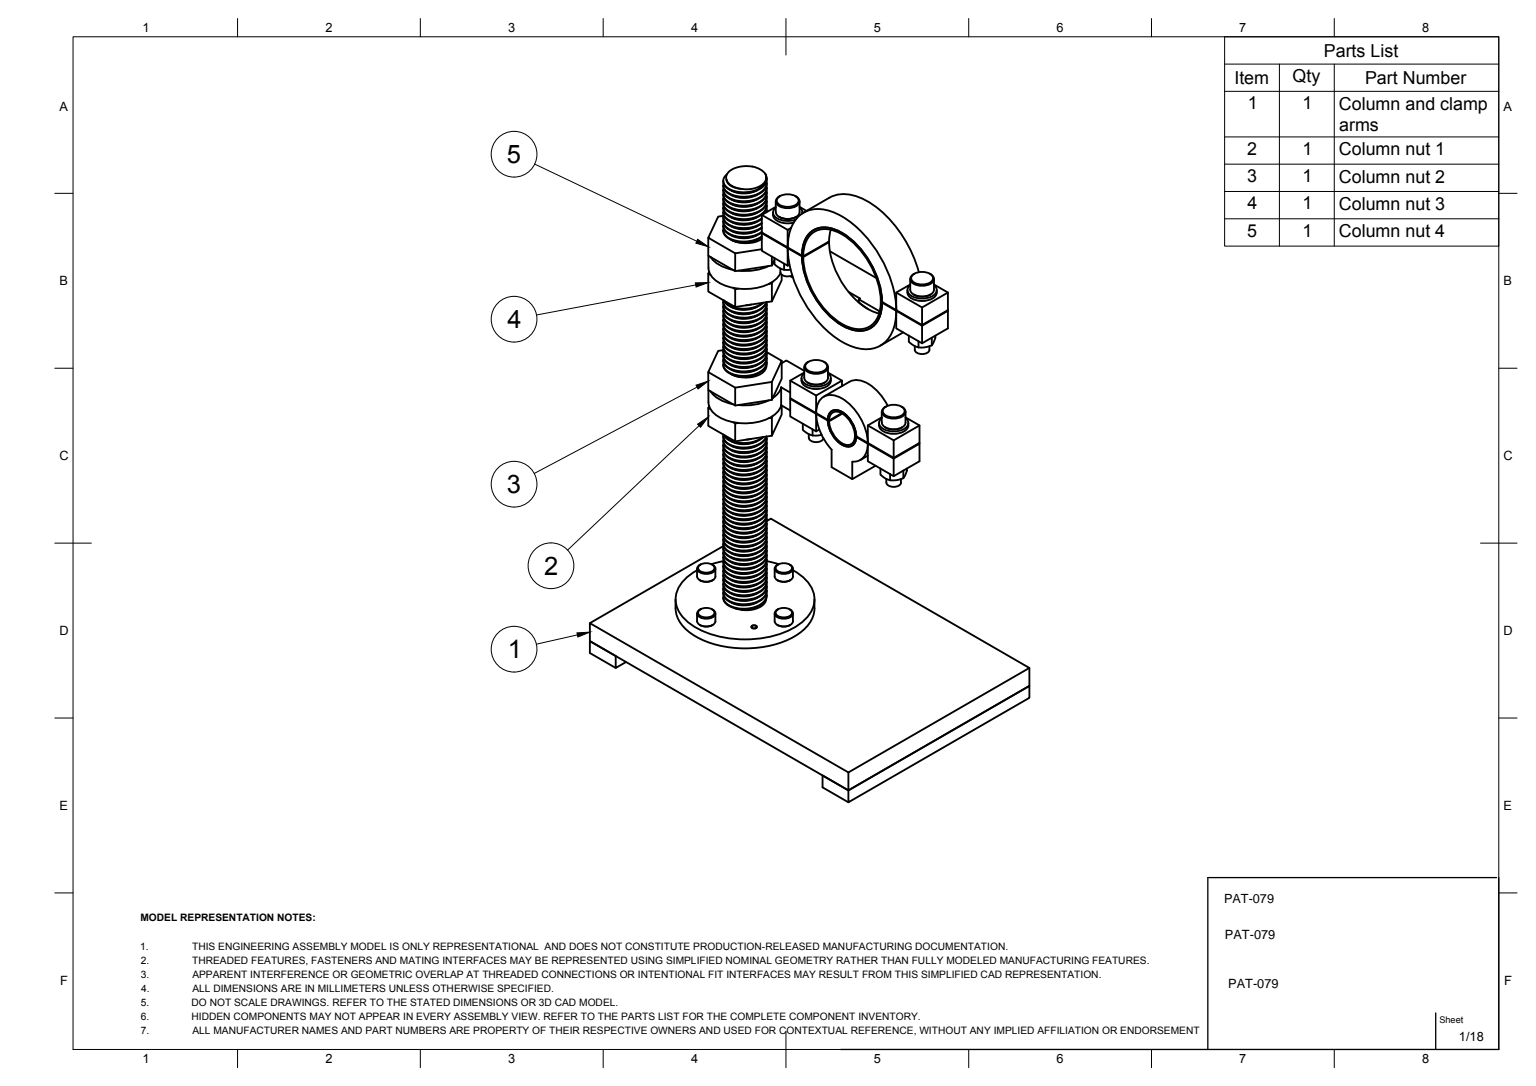
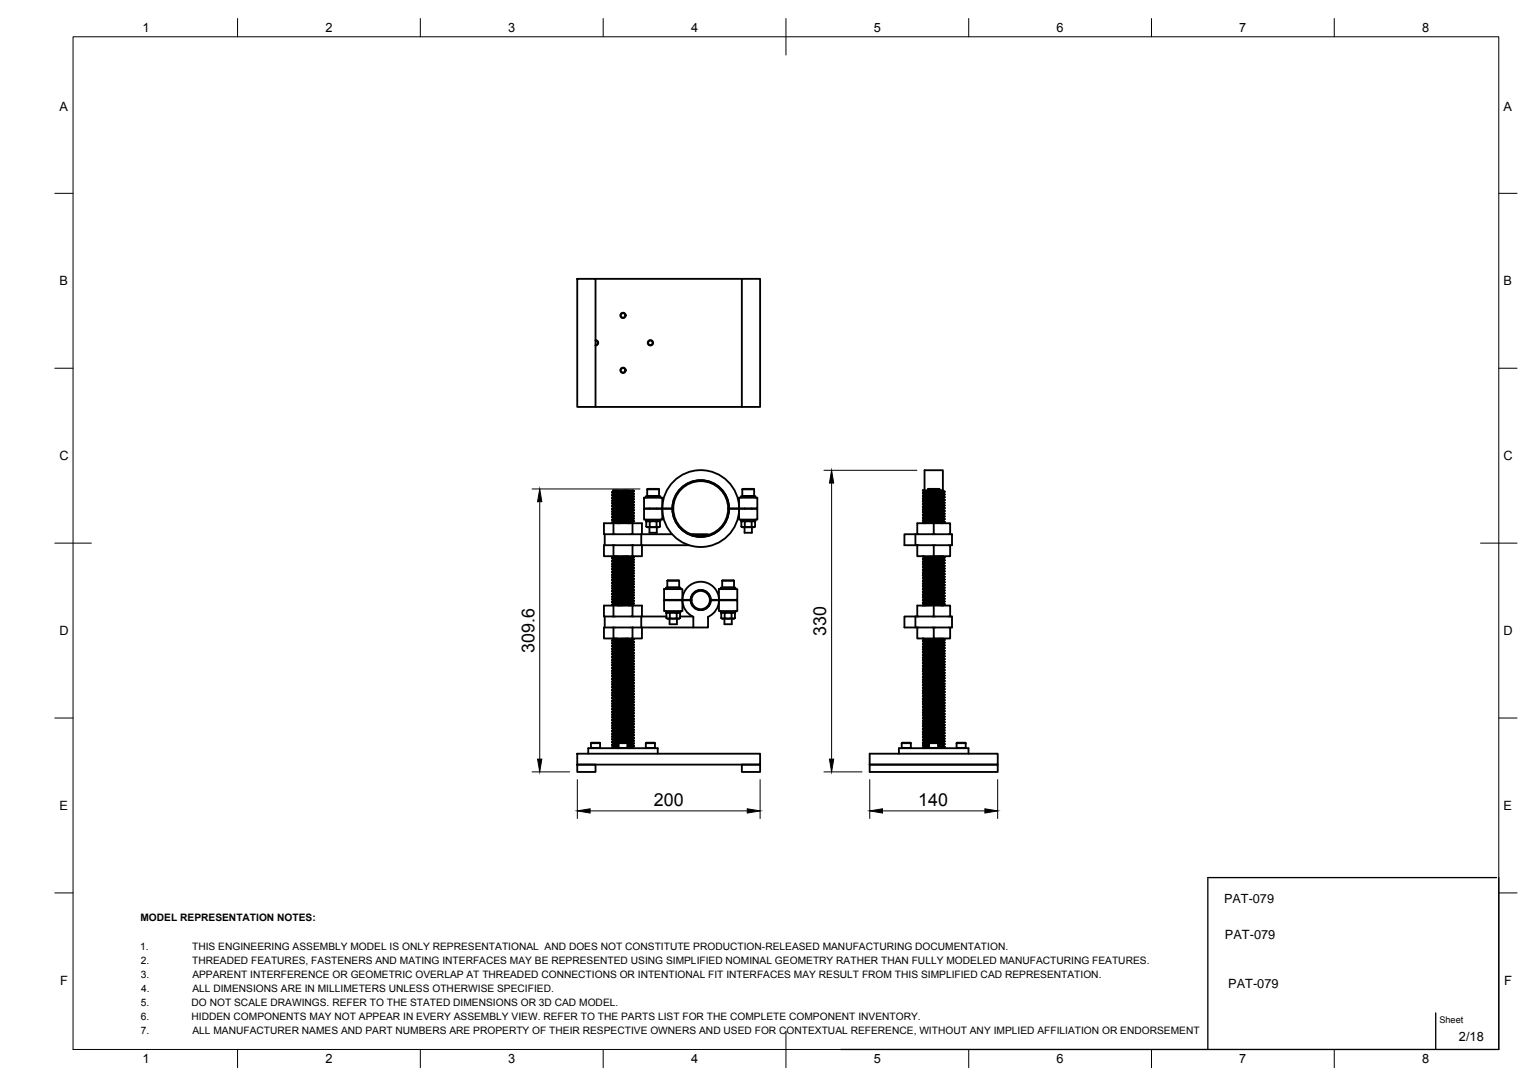
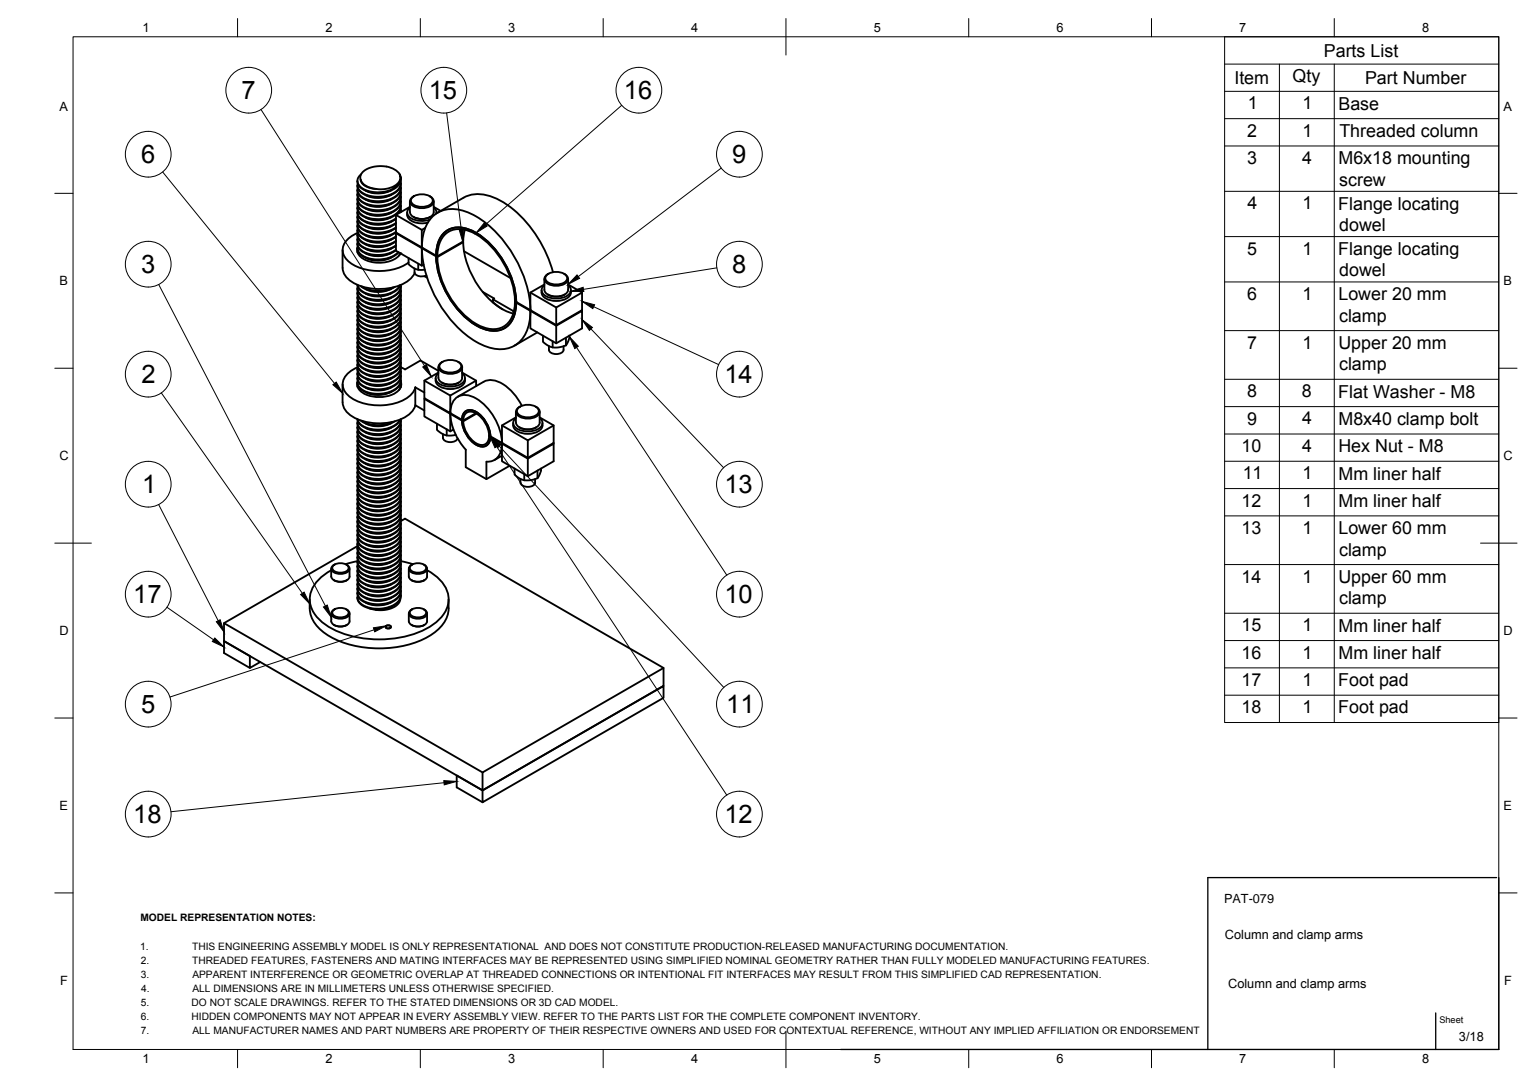
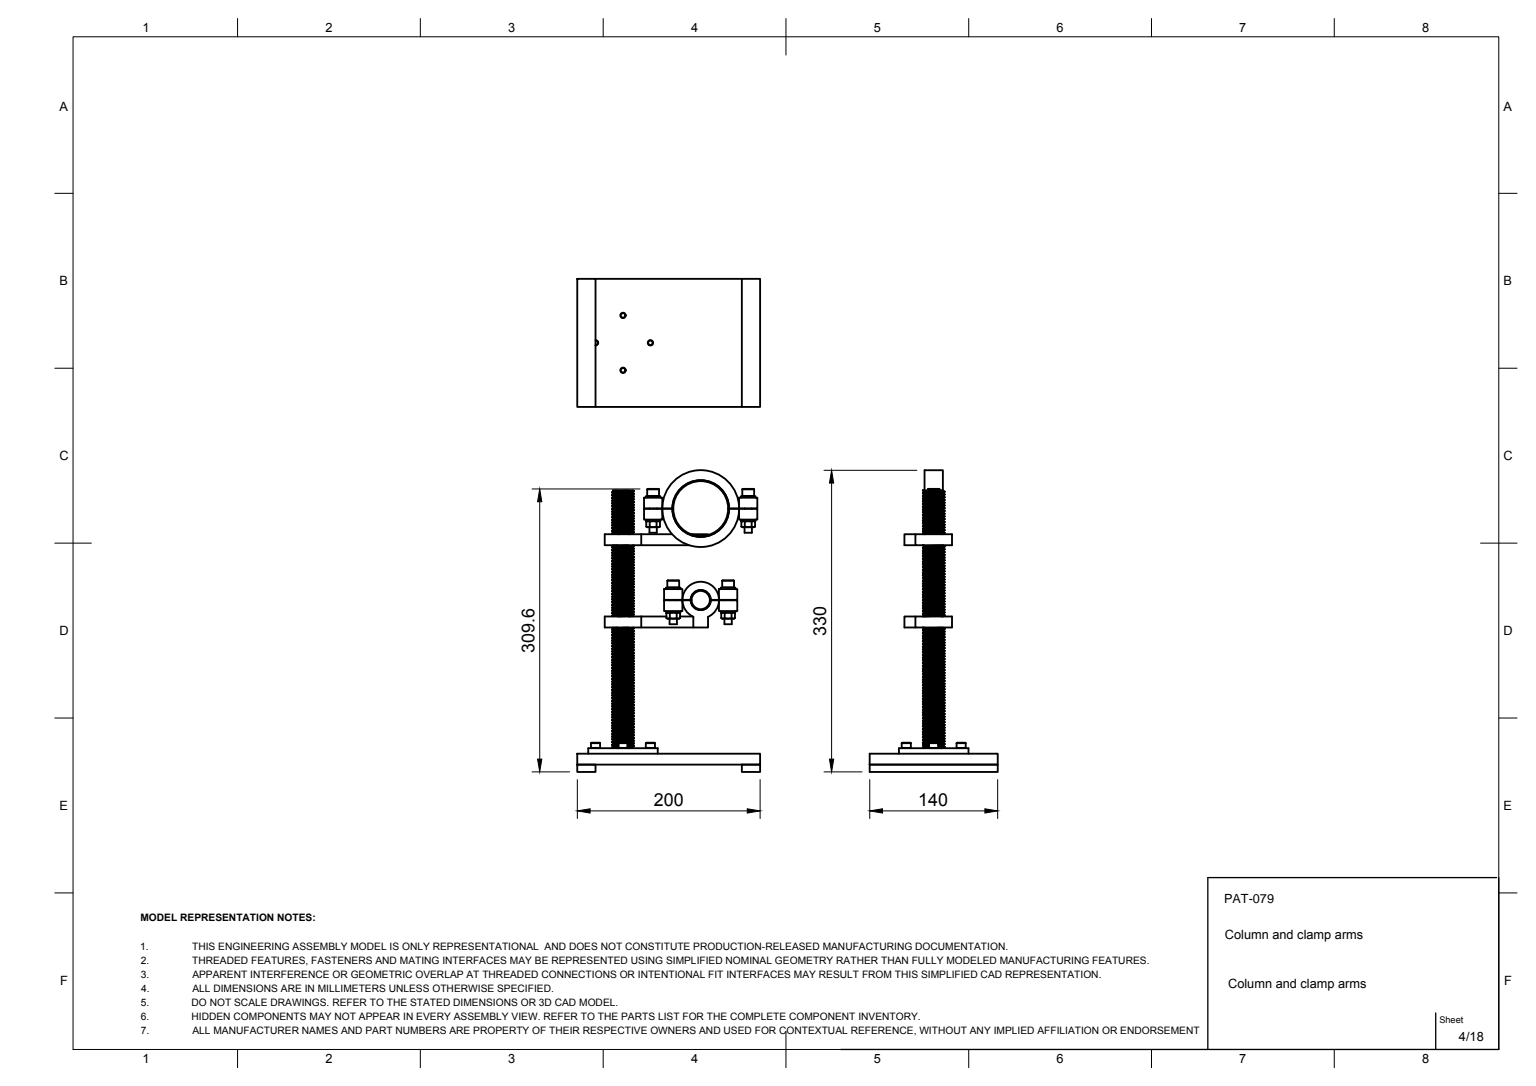
ISO-10303-21;
HEADER;
/* Generated by software containing ST-Developer
 * from STEP Tools, Inc. (www.steptools.com) 
 */

FILE_DESCRIPTION(
/* description */ ('Pipe clamp stand with threaded column'),
/* implementation_level */ '2;1');

FILE_NAME(
/* name */ 'PAT-079',
/* time_stamp */ '2026-10-27T10:55:48-07:00',
/* author */ (''),
/* organization */ (''),
/* preprocessor_version */ 'ST-DEVELOPER v20.2',
/* originating_system */ 'Autodesk Translation Framework v15.17.0.0',
/* authorisation */ '');

FILE_SCHEMA (('AUTOMOTIVE_DESIGN { 1 0 10303 214 3 1 1 }'));
ENDSEC;

DATA;
#10=MECHANICAL_DESIGN_GEOMETRIC_PRESENTATION_REPRESENTATION('',(#741,#742,
#743,#744,#745,#746,#747,#748,#749,#750,#751,#752,#753,#754,#755,#756,#757,
#758,#759,#760,#761,#762,#763,#764,#765,#766,#767,#768,#769,#770),#34433);
#11=ITEM_DEFINED_TRANSFORMATION($,$,#9045,#9586);
#12=ITEM_DEFINED_TRANSFORMATION($,$,#9072,#9587);
#13=ITEM_DEFINED_TRANSFORMATION($,$,#9291,#9588);
#14=ITEM_DEFINED_TRANSFORMATION($,$,#9297,#9589);
#15=ITEM_DEFINED_TRANSFORMATION($,$,#9303,#9590);
#16=ITEM_DEFINED_TRANSFORMATION($,$,#9348,#9591);
#17=ITEM_DEFINED_TRANSFORMATION($,$,#9377,#9592);
#18=ITEM_DEFINED_TRANSFORMATION($,$,#9388,#9593);
#19=ITEM_DEFINED_TRANSFORMATION($,$,#9399,#9594);
#20=ITEM_DEFINED_TRANSFORMATION($,$,#9444,#9595);
#21=ITEM_DEFINED_TRANSFORMATION($,$,#9473,#9596);
#22=ITEM_DEFINED_TRANSFORMATION($,$,#9484,#9597);
#23=ITEM_DEFINED_TRANSFORMATION($,$,#9495,#9598);
#24=ITEM_DEFINED_TRANSFORMATION($,$,#9502,#9599);
#25=ITEM_DEFINED_TRANSFORMATION($,$,#9509,#9600);
#26=ITEM_DEFINED_TRANSFORMATION($,$,#9509,#9601);
#27=ITEM_DEFINED_TRANSFORMATION($,$,#9509,#9602);
#28=ITEM_DEFINED_TRANSFORMATION($,$,#9509,#9603);
#29=ITEM_DEFINED_TRANSFORMATION($,$,#9561,#9604);
#30=ITEM_DEFINED_TRANSFORMATION($,$,#9533,#9605);
#31=ITEM_DEFINED_TRANSFORMATION($,$,#9561,#9606);
#32=ITEM_DEFINED_TRANSFORMATION($,$,#9570,#9607);
#33=ITEM_DEFINED_TRANSFORMATION($,$,#9561,#9608);
#34=ITEM_DEFINED_TRANSFORMATION($,$,#9533,#9609);
#35=ITEM_DEFINED_TRANSFORMATION($,$,#9561,#9610);
#36=ITEM_DEFINED_TRANSFORMATION($,$,#9570,#9611);
#37=ITEM_DEFINED_TRANSFORMATION($,$,#9561,#9612);
#38=ITEM_DEFINED_TRANSFORMATION($,$,#9533,#9613);
#39=ITEM_DEFINED_TRANSFORMATION($,$,#9561,#9614);
#40=ITEM_DEFINED_TRANSFORMATION($,$,#9570,#9615);
#41=ITEM_DEFINED_TRANSFORMATION($,$,#9561,#9616);
#42=ITEM_DEFINED_TRANSFORMATION($,$,#9533,#9617);
#43=ITEM_DEFINED_TRANSFORMATION($,$,#9561,#9618);
#44=ITEM_DEFINED_TRANSFORMATION($,$,#9570,#9619);
#45=ITEM_DEFINED_TRANSFORMATION($,$,#9621,#9644);
#46=ITEM_DEFINED_TRANSFORMATION($,$,#9646,#9669);
#47=ITEM_DEFINED_TRANSFORMATION($,$,#9671,#9694);
#48=ITEM_DEFINED_TRANSFORMATION($,$,#9696,#9719);
#49=ITEM_DEFINED_TRANSFORMATION($,$,#9044,#9720);
#50=ITEM_DEFINED_TRANSFORMATION($,$,#9620,#9721);
#51=ITEM_DEFINED_TRANSFORMATION($,$,#9645,#9722);
#52=ITEM_DEFINED_TRANSFORMATION($,$,#9670,#9723);
#53=ITEM_DEFINED_TRANSFORMATION($,$,#9695,#9724);
#54=(
REPRESENTATION_RELATIONSHIP($,$,#34539,#34538)
REPRESENTATION_RELATIONSHIP_WITH_TRANSFORMATION(#11)
SHAPE_REPRESENTATION_RELATIONSHIP()
);
#55=(
REPRESENTATION_RELATIONSHIP($,$,#34540,#34538)
REPRESENTATION_RELATIONSHIP_WITH_TRANSFORMATION(#12)
SHAPE_REPRESENTATION_RELATIONSHIP()
);
#56=(
REPRESENTATION_RELATIONSHIP($,$,#34541,#34538)
REPRESENTATION_RELATIONSHIP_WITH_TRANSFORMATION(#13)
SHAPE_REPRESENTATION_RELATIONSHIP()
);
#57=(
REPRESENTATION_RELATIONSHIP($,$,#34542,#34538)
REPRESENTATION_RELATIONSHIP_WITH_TRANSFORMATION(#14)
SHAPE_REPRESENTATION_RELATIONSHIP()
);
#58=(
REPRESENTATION_RELATIONSHIP($,$,#34543,#34538)
REPRESENTATION_RELATIONSHIP_WITH_TRANSFORMATION(#15)
SHAPE_REPRESENTATION_RELATIONSHIP()
);
#59=(
REPRESENTATION_RELATIONSHIP($,$,#34544,#34538)
REPRESENTATION_RELATIONSHIP_WITH_TRANSFORMATION(#16)
SHAPE_REPRESENTATION_RELATIONSHIP()
);
#60=(
REPRESENTATION_RELATIONSHIP($,$,#34545,#34538)
REPRESENTATION_RELATIONSHIP_WITH_TRANSFORMATION(#17)
SHAPE_REPRESENTATION_RELATIONSHIP()
);
#61=(
REPRESENTATION_RELATIONSHIP($,$,#34546,#34538)
REPRESENTATION_RELATIONSHIP_WITH_TRANSFORMATION(#18)
SHAPE_REPRESENTATION_RELATIONSHIP()
);
#62=(
REPRESENTATION_RELATIONSHIP($,$,#34547,#34538)
REPRESENTATION_RELATIONSHIP_WITH_TRANSFORMATION(#19)
SHAPE_REPRESENTATION_RELATIONSHIP()
);
#63=(
REPRESENTATION_RELATIONSHIP($,$,#34548,#34538)
REPRESENTATION_RELATIONSHIP_WITH_TRANSFORMATION(#20)
SHAPE_REPRESENTATION_RELATIONSHIP()
);
#64=(
REPRESENTATION_RELATIONSHIP($,$,#34549,#34538)
REPRESENTATION_RELATIONSHIP_WITH_TRANSFORMATION(#21)
SHAPE_REPRESENTATION_RELATIONSHIP()
);
#65=(
REPRESENTATION_RELATIONSHIP($,$,#34550,#34538)
REPRESENTATION_RELATIONSHIP_WITH_TRANSFORMATION(#22)
SHAPE_REPRESENTATION_RELATIONSHIP()
);
#66=(
REPRESENTATION_RELATIONSHIP($,$,#34551,#34538)
REPRESENTATION_RELATIONSHIP_WITH_TRANSFORMATION(#23)
SHAPE_REPRESENTATION_RELATIONSHIP()
);
#67=(
REPRESENTATION_RELATIONSHIP($,$,#34552,#34538)
REPRESENTATION_RELATIONSHIP_WITH_TRANSFORMATION(#24)
SHAPE_REPRESENTATION_RELATIONSHIP()
);
#68=(
REPRESENTATION_RELATIONSHIP($,$,#34553,#34538)
REPRESENTATION_RELATIONSHIP_WITH_TRANSFORMATION(#25)
SHAPE_REPRESENTATION_RELATIONSHIP()
);
#69=(
REPRESENTATION_RELATIONSHIP($,$,#34553,#34538)
REPRESENTATION_RELATIONSHIP_WITH_TRANSFORMATION(#26)
SHAPE_REPRESENTATION_RELATIONSHIP()
);
#70=(
REPRESENTATION_RELATIONSHIP($,$,#34553,#34538)
REPRESENTATION_RELATIONSHIP_WITH_TRANSFORMATION(#27)
SHAPE_REPRESENTATION_RELATIONSHIP()
);
#71=(
REPRESENTATION_RELATIONSHIP($,$,#34553,#34538)
REPRESENTATION_RELATIONSHIP_WITH_TRANSFORMATION(#28)
SHAPE_REPRESENTATION_RELATIONSHIP()
);
#72=(
REPRESENTATION_RELATIONSHIP($,$,#34555,#34538)
REPRESENTATION_RELATIONSHIP_WITH_TRANSFORMATION(#29)
SHAPE_REPRESENTATION_RELATIONSHIP()
);
#73=(
REPRESENTATION_RELATIONSHIP($,$,#34554,#34538)
REPRESENTATION_RELATIONSHIP_WITH_TRANSFORMATION(#30)
SHAPE_REPRESENTATION_RELATIONSHIP()
);
#74=(
REPRESENTATION_RELATIONSHIP($,$,#34555,#34538)
REPRESENTATION_RELATIONSHIP_WITH_TRANSFORMATION(#31)
SHAPE_REPRESENTATION_RELATIONSHIP()
);
#75=(
REPRESENTATION_RELATIONSHIP($,$,#34556,#34538)
REPRESENTATION_RELATIONSHIP_WITH_TRANSFORMATION(#32)
SHAPE_REPRESENTATION_RELATIONSHIP()
);
#76=(
REPRESENTATION_RELATIONSHIP($,$,#34555,#34538)
REPRESENTATION_RELATIONSHIP_WITH_TRANSFORMATION(#33)
SHAPE_REPRESENTATION_RELATIONSHIP()
);
#77=(
REPRESENTATION_RELATIONSHIP($,$,#34554,#34538)
REPRESENTATION_RELATIONSHIP_WITH_TRANSFORMATION(#34)
SHAPE_REPRESENTATION_RELATIONSHIP()
);
#78=(
REPRESENTATION_RELATIONSHIP($,$,#34555,#34538)
REPRESENTATION_RELATIONSHIP_WITH_TRANSFORMATION(#35)
SHAPE_REPRESENTATION_RELATIONSHIP()
);
#79=(
REPRESENTATION_RELATIONSHIP($,$,#34556,#34538)
REPRESENTATION_RELATIONSHIP_WITH_TRANSFORMATION(#36)
SHAPE_REPRESENTATION_RELATIONSHIP()
);
#80=(
REPRESENTATION_RELATIONSHIP($,$,#34555,#34538)
REPRESENTATION_RELATIONSHIP_WITH_TRANSFORMATION(#37)
SHAPE_REPRESENTATION_RELATIONSHIP()
);
#81=(
REPRESENTATION_RELATIONSHIP($,$,#34554,#34538)
REPRESENTATION_RELATIONSHIP_WITH_TRANSFORMATION(#38)
SHAPE_REPRESENTATION_RELATIONSHIP()
);
#82=(
REPRESENTATION_RELATIONSHIP($,$,#34555,#34538)
REPRESENTATION_RELATIONSHIP_WITH_TRANSFORMATION(#39)
SHAPE_REPRESENTATION_RELATIONSHIP()
);
#83=(
REPRESENTATION_RELATIONSHIP($,$,#34556,#34538)
REPRESENTATION_RELATIONSHIP_WITH_TRANSFORMATION(#40)
SHAPE_REPRESENTATION_RELATIONSHIP()
);
#84=(
REPRESENTATION_RELATIONSHIP($,$,#34555,#34538)
REPRESENTATION_RELATIONSHIP_WITH_TRANSFORMATION(#41)
SHAPE_REPRESENTATION_RELATIONSHIP()
);
#85=(
REPRESENTATION_RELATIONSHIP($,$,#34554,#34538)
REPRESENTATION_RELATIONSHIP_WITH_TRANSFORMATION(#42)
SHAPE_REPRESENTATION_RELATIONSHIP()
);
#86=(
REPRESENTATION_RELATIONSHIP($,$,#34555,#34538)
REPRESENTATION_RELATIONSHIP_WITH_TRANSFORMATION(#43)
SHAPE_REPRESENTATION_RELATIONSHIP()
);
#87=(
REPRESENTATION_RELATIONSHIP($,$,#34556,#34538)
REPRESENTATION_RELATIONSHIP_WITH_TRANSFORMATION(#44)
SHAPE_REPRESENTATION_RELATIONSHIP()
);
#88=(
REPRESENTATION_RELATIONSHIP($,$,#34558,#34557)
REPRESENTATION_RELATIONSHIP_WITH_TRANSFORMATION(#45)
SHAPE_REPRESENTATION_RELATIONSHIP()
);
#89=(
REPRESENTATION_RELATIONSHIP($,$,#34560,#34559)
REPRESENTATION_RELATIONSHIP_WITH_TRANSFORMATION(#46)
SHAPE_REPRESENTATION_RELATIONSHIP()
);
#90=(
REPRESENTATION_RELATIONSHIP($,$,#34562,#34561)
REPRESENTATION_RELATIONSHIP_WITH_TRANSFORMATION(#47)
SHAPE_REPRESENTATION_RELATIONSHIP()
);
#91=(
REPRESENTATION_RELATIONSHIP($,$,#34564,#34563)
REPRESENTATION_RELATIONSHIP_WITH_TRANSFORMATION(#48)
SHAPE_REPRESENTATION_RELATIONSHIP()
);
#92=(
REPRESENTATION_RELATIONSHIP($,$,#34538,#34537)
REPRESENTATION_RELATIONSHIP_WITH_TRANSFORMATION(#49)
SHAPE_REPRESENTATION_RELATIONSHIP()
);
#93=(
REPRESENTATION_RELATIONSHIP($,$,#34557,#34537)
REPRESENTATION_RELATIONSHIP_WITH_TRANSFORMATION(#50)
SHAPE_REPRESENTATION_RELATIONSHIP()
);
#94=(
REPRESENTATION_RELATIONSHIP($,$,#34559,#34537)
REPRESENTATION_RELATIONSHIP_WITH_TRANSFORMATION(#51)
SHAPE_REPRESENTATION_RELATIONSHIP()
);
#95=(
REPRESENTATION_RELATIONSHIP($,$,#34561,#34537)
REPRESENTATION_RELATIONSHIP_WITH_TRANSFORMATION(#52)
SHAPE_REPRESENTATION_RELATIONSHIP()
);
#96=(
REPRESENTATION_RELATIONSHIP($,$,#34563,#34537)
REPRESENTATION_RELATIONSHIP_WITH_TRANSFORMATION(#53)
SHAPE_REPRESENTATION_RELATIONSHIP()
);
#97=CONTEXT_DEPENDENT_SHAPE_REPRESENTATION(#54,#34486);
#98=CONTEXT_DEPENDENT_SHAPE_REPRESENTATION(#55,#34487);
#99=CONTEXT_DEPENDENT_SHAPE_REPRESENTATION(#56,#34488);
#100=CONTEXT_DEPENDENT_SHAPE_REPRESENTATION(#57,#34489);
#101=CONTEXT_DEPENDENT_SHAPE_REPRESENTATION(#58,#34490);
#102=CONTEXT_DEPENDENT_SHAPE_REPRESENTATION(#59,#34491);
#103=CONTEXT_DEPENDENT_SHAPE_REPRESENTATION(#60,#34492);
#104=CONTEXT_DEPENDENT_SHAPE_REPRESENTATION(#61,#34493);
#105=CONTEXT_DEPENDENT_SHAPE_REPRESENTATION(#62,#34494);
#106=CONTEXT_DEPENDENT_SHAPE_REPRESENTATION(#63,#34495);
#107=CONTEXT_DEPENDENT_SHAPE_REPRESENTATION(#64,#34496);
#108=CONTEXT_DEPENDENT_SHAPE_REPRESENTATION(#65,#34497);
#109=CONTEXT_DEPENDENT_SHAPE_REPRESENTATION(#66,#34498);
#110=CONTEXT_DEPENDENT_SHAPE_REPRESENTATION(#67,#34499);
#111=CONTEXT_DEPENDENT_SHAPE_REPRESENTATION(#68,#34500);
#112=CONTEXT_DEPENDENT_SHAPE_REPRESENTATION(#69,#34501);
#113=CONTEXT_DEPENDENT_SHAPE_REPRESENTATION(#70,#34502);
#114=CONTEXT_DEPENDENT_SHAPE_REPRESENTATION(#71,#34503);
#115=CONTEXT_DEPENDENT_SHAPE_REPRESENTATION(#72,#34504);
#116=CONTEXT_DEPENDENT_SHAPE_REPRESENTATION(#73,#34505);
#117=CONTEXT_DEPENDENT_SHAPE_REPRESENTATION(#74,#34506);
#118=CONTEXT_DEPENDENT_SHAPE_REPRESENTATION(#75,#34507);
#119=CONTEXT_DEPENDENT_SHAPE_REPRESENTATION(#76,#34508);
#120=CONTEXT_DEPENDENT_SHAPE_REPRESENTATION(#77,#34509);
#121=CONTEXT_DEPENDENT_SHAPE_REPRESENTATION(#78,#34510);
#122=CONTEXT_DEPENDENT_SHAPE_REPRESENTATION(#79,#34511);
#123=CONTEXT_DEPENDENT_SHAPE_REPRESENTATION(#80,#34512);
#124=CONTEXT_DEPENDENT_SHAPE_REPRESENTATION(#81,#34513);
#125=CONTEXT_DEPENDENT_SHAPE_REPRESENTATION(#82,#34514);
#126=CONTEXT_DEPENDENT_SHAPE_REPRESENTATION(#83,#34515);
#127=CONTEXT_DEPENDENT_SHAPE_REPRESENTATION(#84,#34516);
#128=CONTEXT_DEPENDENT_SHAPE_REPRESENTATION(#85,#34517);
#129=CONTEXT_DEPENDENT_SHAPE_REPRESENTATION(#86,#34518);
#130=CONTEXT_DEPENDENT_SHAPE_REPRESENTATION(#87,#34519);
#131=CONTEXT_DEPENDENT_SHAPE_REPRESENTATION(#88,#34522);
#132=CONTEXT_DEPENDENT_SHAPE_REPRESENTATION(#89,#34525);
#133=CONTEXT_DEPENDENT_SHAPE_REPRESENTATION(#90,#34528);
#134=CONTEXT_DEPENDENT_SHAPE_REPRESENTATION(#91,#34531);
#135=CONTEXT_DEPENDENT_SHAPE_REPRESENTATION(#92,#34532);
#136=CONTEXT_DEPENDENT_SHAPE_REPRESENTATION(#93,#34533);
#137=CONTEXT_DEPENDENT_SHAPE_REPRESENTATION(#94,#34534);
#138=CONTEXT_DEPENDENT_SHAPE_REPRESENTATION(#95,#34535);
#139=CONTEXT_DEPENDENT_SHAPE_REPRESENTATION(#96,#34536);
#140=NEXT_ASSEMBLY_USAGE_OCCURRENCE('Base:1','Base:1','Base:1',#34567,#34568,
'Base:1');
#141=NEXT_ASSEMBLY_USAGE_OCCURRENCE('Threaded column:1',
'Threaded column:1','Threaded column:1',#34567,#34569,
'Threaded column:1');
#142=NEXT_ASSEMBLY_USAGE_OCCURRENCE('Flange locating dowel:1',
'Flange locating dowel:1','Flange locating dowel:1',#34567,#34570,
'Flange locating dowel:1');
#143=NEXT_ASSEMBLY_USAGE_OCCURRENCE('Flange locating dowel (1):1',
'Flange locating dowel (1):1','Flange locating dowel (1):1',#34567,#34571,
'Flange locating dowel (1):1');
#144=NEXT_ASSEMBLY_USAGE_OCCURRENCE('Lower 20 mm clamp:1',
'Lower 20 mm clamp:1','Lower 20 mm clamp:1',#34567,#34572,
'Lower 20 mm clamp:1');
#145=NEXT_ASSEMBLY_USAGE_OCCURRENCE('Upper 20 mm clamp:1',
'Upper 20 mm clamp:1','Upper 20 mm clamp:1',#34567,#34573,
'Upper 20 mm clamp:1');
#146=NEXT_ASSEMBLY_USAGE_OCCURRENCE('mm liner half:1','mm liner half:1',
'mm liner half:1',#34567,#34574,'mm liner half:1');
#147=NEXT_ASSEMBLY_USAGE_OCCURRENCE('mm liner half (1):1',
'mm liner half (1):1','mm liner half (1):1',#34567,#34575,
'mm liner half (1):1');
#148=NEXT_ASSEMBLY_USAGE_OCCURRENCE('Lower 60 mm clamp:1',
'Lower 60 mm clamp:1','Lower 60 mm clamp:1',#34567,#34576,
'Lower 60 mm clamp:1');
#149=NEXT_ASSEMBLY_USAGE_OCCURRENCE('Upper 60 mm clamp:1',
'Upper 60 mm clamp:1','Upper 60 mm clamp:1',#34567,#34577,
'Upper 60 mm clamp:1');
#150=NEXT_ASSEMBLY_USAGE_OCCURRENCE('mm liner half (2):1',
'mm liner half (2):1','mm liner half (2):1',#34567,#34578,
'mm liner half (2):1');
#151=NEXT_ASSEMBLY_USAGE_OCCURRENCE('mm liner half (3):1',
'mm liner half (3):1','mm liner half (3):1',#34567,#34579,
'mm liner half (3):1');
#152=NEXT_ASSEMBLY_USAGE_OCCURRENCE('Foot pad:1','Foot pad:1',
'Foot pad:1',#34567,#34580,'Foot pad:1');
#153=NEXT_ASSEMBLY_USAGE_OCCURRENCE('Foot pad (1):1','Foot pad (1):1',
'Foot pad (1):1',#34567,#34581,'Foot pad (1):1');
#154=NEXT_ASSEMBLY_USAGE_OCCURRENCE('M6x18 mounting screw:2',
'M6x18 mounting screw:2','M6x18 mounting screw:2',#34567,#34582,
'M6x18 mounting screw:2');
#155=NEXT_ASSEMBLY_USAGE_OCCURRENCE('M6x18 mounting screw:3',
'M6x18 mounting screw:3','M6x18 mounting screw:3',#34567,#34582,
'M6x18 mounting screw:3');
#156=NEXT_ASSEMBLY_USAGE_OCCURRENCE('M6x18 mounting screw:4',
'M6x18 mounting screw:4','M6x18 mounting screw:4',#34567,#34582,
'M6x18 mounting screw:4');
#157=NEXT_ASSEMBLY_USAGE_OCCURRENCE('M6x18 mounting screw:5',
'M6x18 mounting screw:5','M6x18 mounting screw:5',#34567,#34582,
'M6x18 mounting screw:5');
#158=NEXT_ASSEMBLY_USAGE_OCCURRENCE('Flat Washer - M8:2',
'Flat Washer - M8:2','Flat Washer - M8:2',#34567,#34584,
'Flat Washer - M8:2');
#159=NEXT_ASSEMBLY_USAGE_OCCURRENCE('M8x40 clamp bolt:2',
'M8x40 clamp bolt:2','M8x40 clamp bolt:2',#34567,#34583,
'M8x40 clamp bolt:2');
#160=NEXT_ASSEMBLY_USAGE_OCCURRENCE('Flat Washer - M8:3',
'Flat Washer - M8:3','Flat Washer - M8:3',#34567,#34584,
'Flat Washer - M8:3');
#161=NEXT_ASSEMBLY_USAGE_OCCURRENCE('Hex Nut - M8:2','Hex Nut - M8:2',
'Hex Nut - M8:2',#34567,#34585,'Hex Nut - M8:2');
#162=NEXT_ASSEMBLY_USAGE_OCCURRENCE('Flat Washer - M8:4',
'Flat Washer - M8:4','Flat Washer - M8:4',#34567,#34584,
'Flat Washer - M8:4');
#163=NEXT_ASSEMBLY_USAGE_OCCURRENCE('M8x40 clamp bolt:3',
'M8x40 clamp bolt:3','M8x40 clamp bolt:3',#34567,#34583,
'M8x40 clamp bolt:3');
#164=NEXT_ASSEMBLY_USAGE_OCCURRENCE('Flat Washer - M8:5',
'Flat Washer - M8:5','Flat Washer - M8:5',#34567,#34584,
'Flat Washer - M8:5');
#165=NEXT_ASSEMBLY_USAGE_OCCURRENCE('Hex Nut - M8:3','Hex Nut - M8:3',
'Hex Nut - M8:3',#34567,#34585,'Hex Nut - M8:3');
#166=NEXT_ASSEMBLY_USAGE_OCCURRENCE('Flat Washer - M8:6',
'Flat Washer - M8:6','Flat Washer - M8:6',#34567,#34584,
'Flat Washer - M8:6');
#167=NEXT_ASSEMBLY_USAGE_OCCURRENCE('M8x40 clamp bolt:4',
'M8x40 clamp bolt:4','M8x40 clamp bolt:4',#34567,#34583,
'M8x40 clamp bolt:4');
#168=NEXT_ASSEMBLY_USAGE_OCCURRENCE('Flat Washer - M8:7',
'Flat Washer - M8:7','Flat Washer - M8:7',#34567,#34584,
'Flat Washer - M8:7');
#169=NEXT_ASSEMBLY_USAGE_OCCURRENCE('Hex Nut - M8:4','Hex Nut - M8:4',
'Hex Nut - M8:4',#34567,#34585,'Hex Nut - M8:4');
#170=NEXT_ASSEMBLY_USAGE_OCCURRENCE('Flat Washer - M8:8',
'Flat Washer - M8:8','Flat Washer - M8:8',#34567,#34584,
'Flat Washer - M8:8');
#171=NEXT_ASSEMBLY_USAGE_OCCURRENCE('M8x40 clamp bolt:5',
'M8x40 clamp bolt:5','M8x40 clamp bolt:5',#34567,#34583,
'M8x40 clamp bolt:5');
#172=NEXT_ASSEMBLY_USAGE_OCCURRENCE('Flat Washer - M8:9',
'Flat Washer - M8:9','Flat Washer - M8:9',#34567,#34584,
'Flat Washer - M8:9');
#173=NEXT_ASSEMBLY_USAGE_OCCURRENCE('Hex Nut - M8:5','Hex Nut - M8:5',
'Hex Nut - M8:5',#34567,#34585,'Hex Nut - M8:5');
#174=NEXT_ASSEMBLY_USAGE_OCCURRENCE('M24 adjustment nut:1',
'M24 adjustment nut:1','M24 adjustment nut:1',#34586,#34587,
'M24 adjustment nut:1');
#175=NEXT_ASSEMBLY_USAGE_OCCURRENCE('M24 adjustment nut (1):1',
'M24 adjustment nut (1):1','M24 adjustment nut (1):1',#34588,#34589,
'M24 adjustment nut (1):1');
#176=NEXT_ASSEMBLY_USAGE_OCCURRENCE('M24 adjustment nut (2):1',
'M24 adjustment nut (2):1','M24 adjustment nut (2):1',#34590,#34591,
'M24 adjustment nut (2):1');
#177=NEXT_ASSEMBLY_USAGE_OCCURRENCE('M24 adjustment nut (3):1',
'M24 adjustment nut (3):1','M24 adjustment nut (3):1',#34592,#34593,
'M24 adjustment nut (3):1');
#178=NEXT_ASSEMBLY_USAGE_OCCURRENCE('Column and clamp arms:1',
'Column and clamp arms:1','Column and clamp arms:1',#34566,#34567,
'Column and clamp arms:1');
#179=NEXT_ASSEMBLY_USAGE_OCCURRENCE('Column nut 1:1','Column nut 1:1',
'Column nut 1:1',#34566,#34586,'Column nut 1:1');
#180=NEXT_ASSEMBLY_USAGE_OCCURRENCE('Column nut 2:1','Column nut 2:1',
'Column nut 2:1',#34566,#34588,'Column nut 2:1');
#181=NEXT_ASSEMBLY_USAGE_OCCURRENCE('Column nut 3:1','Column nut 3:1',
'Column nut 3:1',#34566,#34590,'Column nut 3:1');
#182=NEXT_ASSEMBLY_USAGE_OCCURRENCE('Column nut 4:1','Column nut 4:1',
'Column nut 4:1',#34566,#34592,'Column nut 4:1');
#183=(
BOUNDED_CURVE()
B_SPLINE_CURVE(2,(#28836,#28837,#28838),.UNSPECIFIED.,.F.,.F.)
B_SPLINE_CURVE_WITH_KNOTS((3,3),(0.14973948338295,0.97160236658079),
 .UNSPECIFIED.)
CURVE()
GEOMETRIC_REPRESENTATION_ITEM()
RATIONAL_B_SPLINE_CURVE((1.07140024848292,1.23714644374248,1.07140024848292))
REPRESENTATION_ITEM('')
);
#184=(
BOUNDED_CURVE()
B_SPLINE_CURVE(2,(#28840,#28841,#28842),.UNSPECIFIED.,.F.,.F.)
B_SPLINE_CURVE_WITH_KNOTS((3,3),(0.14973948338295,0.971602366580789),
 .UNSPECIFIED.)
CURVE()
GEOMETRIC_REPRESENTATION_ITEM()
RATIONAL_B_SPLINE_CURVE((1.07140024848292,1.23714644374248,1.07140024848292))
REPRESENTATION_ITEM('')
);
#185=(
BOUNDED_CURVE()
B_SPLINE_CURVE(2,(#28847,#28848,#28849),.UNSPECIFIED.,.F.,.F.)
B_SPLINE_CURVE_WITH_KNOTS((3,3),(0.14973948338295,0.97160236658079),
 .UNSPECIFIED.)
CURVE()
GEOMETRIC_REPRESENTATION_ITEM()
RATIONAL_B_SPLINE_CURVE((1.07140024848292,1.23714644374248,1.07140024848292))
REPRESENTATION_ITEM('')
);
#186=(
BOUNDED_CURVE()
B_SPLINE_CURVE(2,(#28851,#28852,#28853),.UNSPECIFIED.,.F.,.F.)
B_SPLINE_CURVE_WITH_KNOTS((3,3),(0.14973948338295,0.97160236658079),
 .UNSPECIFIED.)
CURVE()
GEOMETRIC_REPRESENTATION_ITEM()
RATIONAL_B_SPLINE_CURVE((1.07140024848292,1.23714644374248,1.07140024848292))
REPRESENTATION_ITEM('')
);
#187=(
BOUNDED_CURVE()
B_SPLINE_CURVE(2,(#28855,#28856,#28857),.UNSPECIFIED.,.F.,.F.)
B_SPLINE_CURVE_WITH_KNOTS((3,3),(0.14973948338295,0.971602366580789),
 .UNSPECIFIED.)
CURVE()
GEOMETRIC_REPRESENTATION_ITEM()
RATIONAL_B_SPLINE_CURVE((1.07140024848292,1.23714644374248,1.07140024848292))
REPRESENTATION_ITEM('')
);
#188=(
BOUNDED_CURVE()
B_SPLINE_CURVE(2,(#28858,#28859,#28860),.UNSPECIFIED.,.F.,.F.)
B_SPLINE_CURVE_WITH_KNOTS((3,3),(0.14973948338295,0.97160236658079),
 .UNSPECIFIED.)
CURVE()
GEOMETRIC_REPRESENTATION_ITEM()
RATIONAL_B_SPLINE_CURVE((1.07140024848292,1.23714644374248,1.07140024848292))
REPRESENTATION_ITEM('')
);
#189=(
BOUNDED_CURVE()
B_SPLINE_CURVE(2,(#28867,#28868,#28869),.UNSPECIFIED.,.F.,.F.)
B_SPLINE_CURVE_WITH_KNOTS((3,3),(0.14973948338295,0.97160236658079),
 .UNSPECIFIED.)
CURVE()
GEOMETRIC_REPRESENTATION_ITEM()
RATIONAL_B_SPLINE_CURVE((1.07140024848292,1.23714644374248,1.07140024848292))
REPRESENTATION_ITEM('')
);
#190=(
BOUNDED_CURVE()
B_SPLINE_CURVE(2,(#28871,#28872,#28873),.UNSPECIFIED.,.F.,.F.)
B_SPLINE_CURVE_WITH_KNOTS((3,3),(0.14973948338295,0.97160236658079),
 .UNSPECIFIED.)
CURVE()
GEOMETRIC_REPRESENTATION_ITEM()
RATIONAL_B_SPLINE_CURVE((1.07140024848292,1.23714644374248,1.07140024848292))
REPRESENTATION_ITEM('')
);
#191=(
BOUNDED_CURVE()
B_SPLINE_CURVE(2,(#28875,#28876,#28877),.UNSPECIFIED.,.F.,.F.)
B_SPLINE_CURVE_WITH_KNOTS((3,3),(0.14973948338295,0.971602366580789),
 .UNSPECIFIED.)
CURVE()
GEOMETRIC_REPRESENTATION_ITEM()
RATIONAL_B_SPLINE_CURVE((1.07140024848292,1.23714644374248,1.07140024848292))
REPRESENTATION_ITEM('')
);
#192=(
BOUNDED_CURVE()
B_SPLINE_CURVE(2,(#28879,#28880,#28881),.UNSPECIFIED.,.F.,.F.)
B_SPLINE_CURVE_WITH_KNOTS((3,3),(0.14973948338295,0.97160236658079),
 .UNSPECIFIED.)
CURVE()
GEOMETRIC_REPRESENTATION_ITEM()
RATIONAL_B_SPLINE_CURVE((1.07140024848292,1.23714644374248,1.07140024848292))
REPRESENTATION_ITEM('')
);
#193=(
BOUNDED_CURVE()
B_SPLINE_CURVE(2,(#28883,#28884,#28885),.UNSPECIFIED.,.F.,.F.)
B_SPLINE_CURVE_WITH_KNOTS((3,3),(0.14973948338295,0.97160236658079),
 .UNSPECIFIED.)
CURVE()
GEOMETRIC_REPRESENTATION_ITEM()
RATIONAL_B_SPLINE_CURVE((1.07140024848292,1.23714644374248,1.07140024848292))
REPRESENTATION_ITEM('')
);
#194=(
BOUNDED_CURVE()
B_SPLINE_CURVE(2,(#28886,#28887,#28888),.UNSPECIFIED.,.F.,.F.)
B_SPLINE_CURVE_WITH_KNOTS((3,3),(0.14973948338295,0.971602366580789),
 .UNSPECIFIED.)
CURVE()
GEOMETRIC_REPRESENTATION_ITEM()
RATIONAL_B_SPLINE_CURVE((1.07140024848292,1.23714644374248,1.07140024848292))
REPRESENTATION_ITEM('')
);
#195=CONICAL_SURFACE('',#9522,0.475,0.785398163397449);
#196=CONICAL_SURFACE('',#9526,0.485,0.785398163397448);
#197=CONICAL_SURFACE('',#9530,0.31,0.463647609000806);
#198=CONICAL_SURFACE('',#9550,0.625,0.785398163397448);
#199=CONICAL_SURFACE('',#9554,0.635,0.785398163397449);
#200=CONICAL_SURFACE('',#9558,0.41,0.463647609000806);
#201=CONICAL_SURFACE('',#9571,0.734027674973257,1.0471975511966);
#202=CONICAL_SURFACE('',#9573,0.734027674973257,1.0471975511966);
#203=ORIENTED_CLOSED_SHELL('',*,#8790,.F.);
#204=ORIENTED_CLOSED_SHELL('',*,#8792,.F.);
#205=BREP_WITH_VOIDS('Body1',#8791,(#203));
#206=BREP_WITH_VOIDS('Body1',#8793,(#204));
#207=B_SPLINE_SURFACE_WITH_KNOTS('',3,3,((#22386,#22387,#22388,#22389,#22390,
#22391,#22392,#22393,#22394,#22395,#22396,#22397,#22398,#22399,#22400,#22401,
#22402,#22403,#22404,#22405,#22406,#22407,#22408,#22409,#22410,#22411,#22412,
#22413,#22414,#22415,#22416,#22417,#22418,#22419,#22420,#22421,#22422,#22423,
#22424,#22425,#22426,#22427,#22428,#22429,#22430,#22431,#22432,#22433,#22434,
#22435,#22436,#22437,#22438,#22439,#22440,#22441,#22442,#22443,#22444,#22445,
#22446,#22447,#22448,#22449,#22450,#22451,#22452,#22453,#22454,#22455,#22456,
#22457,#22458,#22459,#22460,#22461,#22462,#22463,#22464,#22465,#22466,#22467,
#22468,#22469,#22470,#22471,#22472,#22473,#22474,#22475,#22476,#22477,#22478,
#22479,#22480,#22481,#22482,#22483,#22484,#22485,#22486,#22487,#22488,#22489,
#22490,#22491,#22492,#22493,#22494,#22495,#22496,#22497,#22498,#22499,#22500,
#22501,#22502,#22503,#22504,#22505,#22506,#22507,#22508,#22509,#22510,#22511,
#22512,#22513,#22514,#22515,#22516,#22517,#22518,#22519,#22520,#22521,#22522,
#22523,#22524,#22525,#22526,#22527,#22528,#22529,#22530,#22531,#22532,#22533,
#22534,#22535,#22536,#22537,#22538,#22539,#22540,#22541,#22542,#22543,#22544,
#22545,#22546,#22547,#22548,#22549,#22550,#22551,#22552,#22553,#22554,#22555,
#22556,#22557,#22558,#22559,#22560,#22561,#22562,#22563,#22564,#22565,#22566,
#22567,#22568,#22569,#22570,#22571,#22572,#22573,#22574,#22575,#22576,#22577,
#22578,#22579,#22580,#22581,#22582,#22583,#22584,#22585,#22586,#22587,#22588,
#22589,#22590,#22591,#22592,#22593,#22594,#22595,#22596,#22597,#22598,#22599,
#22600,#22601,#22602,#22603,#22604,#22605,#22606,#22607,#22608,#22609,#22610,
#22611,#22612,#22613,#22614,#22615,#22616,#22617,#22618,#22619,#22620,#22621,
#22622,#22623,#22624,#22625,#22626,#22627,#22628,#22629,#22630,#22631,#22632,
#22633,#22634,#22635,#22636,#22637,#22638,#22639,#22640,#22641,#22642,#22643,
#22644,#22645,#22646,#22647,#22648,#22649,#22650,#22651,#22652,#22653,#22654,
#22655,#22656,#22657,#22658,#22659,#22660,#22661,#22662,#22663,#22664,#22665,
#22666,#22667,#22668,#22669,#22670,#22671,#22672,#22673,#22674,#22675,#22676,
#22677,#22678,#22679,#22680,#22681,#22682,#22683,#22684,#22685,#22686,#22687,
#22688,#22689,#22690,#22691,#22692,#22693,#22694,#22695,#22696,#22697,#22698,
#22699,#22700,#22701,#22702,#22703,#22704,#22705,#22706,#22707,#22708,#22709,
#22710,#22711,#22712,#22713,#22714,#22715,#22716,#22717,#22718,#22719,#22720,
#22721,#22722,#22723,#22724,#22725,#22726,#22727,#22728,#22729,#22730,#22731,
#22732,#22733,#22734,#22735,#22736,#22737,#22738,#22739,#22740,#22741,#22742,
#22743,#22744,#22745,#22746,#22747,#22748,#22749,#22750,#22751,#22752,#22753,
#22754,#22755,#22756,#22757,#22758,#22759,#22760,#22761,#22762,#22763,#22764,
#22765,#22766,#22767,#22768,#22769,#22770,#22771,#22772,#22773,#22774,#22775,
#22776,#22777,#22778,#22779,#22780,#22781,#22782,#22783,#22784,#22785,#22786,
#22787,#22788,#22789,#22790,#22791,#22792,#22793,#22794,#22795,#22796,#22797,
#22798,#22799,#22800,#22801,#22802,#22803,#22804,#22805,#22806,#22807,#22808,
#22809,#22810,#22811,#22812,#22813,#22814,#22815,#22816,#22817,#22818,#22819,
#22820,#22821,#22822,#22823,#22824,#22825,#22826,#22827,#22828,#22829,#22830,
#22831,#22832,#22833,#22834,#22835,#22836,#22837,#22838,#22839,#22840,#22841,
#22842,#22843,#22844,#22845,#22846,#22847,#22848,#22849,#22850,#22851,#22852,
#22853,#22854,#22855,#22856,#22857,#22858,#22859,#22860,#22861,#22862,#22863,
#22864,#22865,#22866,#22867,#22868,#22869,#22870,#22871,#22872,#22873,#22874,
#22875,#22876,#22877,#22878,#22879,#22880,#22881,#22882,#22883,#22884,#22885,
#22886,#22887,#22888,#22889,#22890,#22891,#22892,#22893,#22894,#22895,#22896,
#22897,#22898,#22899,#22900,#22901,#22902,#22903,#22904,#22905,#22906,#22907,
#22908,#22909,#22910,#22911,#22912,#22913,#22914,#22915,#22916,#22917,#22918,
#22919,#22920,#22921,#22922,#22923,#22924,#22925,#22926,#22927,#22928,#22929,
#22930,#22931,#22932,#22933,#22934,#22935,#22936,#22937,#22938,#22939,#22940,
#22941,#22942,#22943,#22944,#22945,#22946,#22947,#22948,#22949,#22950,#22951,
#22952,#22953,#22954,#22955,#22956,#22957,#22958,#22959,#22960,#22961,#22962,
#22963,#22964,#22965,#22966,#22967,#22968,#22969,#22970,#22971,#22972,#22973,
#22974,#22975,#22976,#22977,#22978,#22979,#22980,#22981,#22982,#22983,#22984,
#22985,#22986,#22987,#22988,#22989,#22990,#22991,#22992,#22993,#22994,#22995,
#22996,#22997,#22998,#22999,#23000,#23001,#23002,#23003,#23004,#23005,#23006,
#23007,#23008,#23009,#23010,#23011,#23012,#23013,#23014,#23015,#23016,#23017,
#23018,#23019,#23020,#23021,#23022,#23023,#23024,#23025,#23026,#23027,#23028,
#23029,#23030,#23031,#23032,#23033,#23034,#23035,#23036,#23037,#23038,#23039,
#23040,#23041,#23042,#23043,#23044,#23045,#23046,#23047,#23048,#23049,#23050,
#23051,#23052,#23053,#23054,#23055,#23056,#23057,#23058,#23059,#23060,#23061,
#23062,#23063,#23064,#23065,#23066,#23067),(#23068,#23069,#23070,#23071,
#23072,#23073,#23074,#23075,#23076,#23077,#23078,#23079,#23080,#23081,#23082,
#23083,#23084,#23085,#23086,#23087,#23088,#23089,#23090,#23091,#23092,#23093,
#23094,#23095,#23096,#23097,#23098,#23099,#23100,#23101,#23102,#23103,#23104,
#23105,#23106,#23107,#23108,#23109,#23110,#23111,#23112,#23113,#23114,#23115,
#23116,#23117,#23118,#23119,#23120,#23121,#23122,#23123,#23124,#23125,#23126,
#23127,#23128,#23129,#23130,#23131,#23132,#23133,#23134,#23135,#23136,#23137,
#23138,#23139,#23140,#23141,#23142,#23143,#23144,#23145,#23146,#23147,#23148,
#23149,#23150,#23151,#23152,#23153,#23154,#23155,#23156,#23157,#23158,#23159,
#23160,#23161,#23162,#23163,#23164,#23165,#23166,#23167,#23168,#23169,#23170,
#23171,#23172,#23173,#23174,#23175,#23176,#23177,#23178,#23179,#23180,#23181,
#23182,#23183,#23184,#23185,#23186,#23187,#23188,#23189,#23190,#23191,#23192,
#23193,#23194,#23195,#23196,#23197,#23198,#23199,#23200,#23201,#23202,#23203,
#23204,#23205,#23206,#23207,#23208,#23209,#23210,#23211,#23212,#23213,#23214,
#23215,#23216,#23217,#23218,#23219,#23220,#23221,#23222,#23223,#23224,#23225,
#23226,#23227,#23228,#23229,#23230,#23231,#23232,#23233,#23234,#23235,#23236,
#23237,#23238,#23239,#23240,#23241,#23242,#23243,#23244,#23245,#23246,#23247,
#23248,#23249,#23250,#23251,#23252,#23253,#23254,#23255,#23256,#23257,#23258,
#23259,#23260,#23261,#23262,#23263,#23264,#23265,#23266,#23267,#23268,#23269,
#23270,#23271,#23272,#23273,#23274,#23275,#23276,#23277,#23278,#23279,#23280,
#23281,#23282,#23283,#23284,#23285,#23286,#23287,#23288,#23289,#23290,#23291,
#23292,#23293,#23294,#23295,#23296,#23297,#23298,#23299,#23300,#23301,#23302,
#23303,#23304,#23305,#23306,#23307,#23308,#23309,#23310,#23311,#23312,#23313,
#23314,#23315,#23316,#23317,#23318,#23319,#23320,#23321,#23322,#23323,#23324,
#23325,#23326,#23327,#23328,#23329,#23330,#23331,#23332,#23333,#23334,#23335,
#23336,#23337,#23338,#23339,#23340,#23341,#23342,#23343,#23344,#23345,#23346,
#23347,#23348,#23349,#23350,#23351,#23352,#23353,#23354,#23355,#23356,#23357,
#23358,#23359,#23360,#23361,#23362,#23363,#23364,#23365,#23366,#23367,#23368,
#23369,#23370,#23371,#23372,#23373,#23374,#23375,#23376,#23377,#23378,#23379,
#23380,#23381,#23382,#23383,#23384,#23385,#23386,#23387,#23388,#23389,#23390,
#23391,#23392,#23393,#23394,#23395,#23396,#23397,#23398,#23399,#23400,#23401,
#23402,#23403,#23404,#23405,#23406,#23407,#23408,#23409,#23410,#23411,#23412,
#23413,#23414,#23415,#23416,#23417,#23418,#23419,#23420,#23421,#23422,#23423,
#23424,#23425,#23426,#23427,#23428,#23429,#23430,#23431,#23432,#23433,#23434,
#23435,#23436,#23437,#23438,#23439,#23440,#23441,#23442,#23443,#23444,#23445,
#23446,#23447,#23448,#23449,#23450,#23451,#23452,#23453,#23454,#23455,#23456,
#23457,#23458,#23459,#23460,#23461,#23462,#23463,#23464,#23465,#23466,#23467,
#23468,#23469,#23470,#23471,#23472,#23473,#23474,#23475,#23476,#23477,#23478,
#23479,#23480,#23481,#23482,#23483,#23484,#23485,#23486,#23487,#23488,#23489,
#23490,#23491,#23492,#23493,#23494,#23495,#23496,#23497,#23498,#23499,#23500,
#23501,#23502,#23503,#23504,#23505,#23506,#23507,#23508,#23509,#23510,#23511,
#23512,#23513,#23514,#23515,#23516,#23517,#23518,#23519,#23520,#23521,#23522,
#23523,#23524,#23525,#23526,#23527,#23528,#23529,#23530,#23531,#23532,#23533,
#23534,#23535,#23536,#23537,#23538,#23539,#23540,#23541,#23542,#23543,#23544,
#23545,#23546,#23547,#23548,#23549,#23550,#23551,#23552,#23553,#23554,#23555,
#23556,#23557,#23558,#23559,#23560,#23561,#23562,#23563,#23564,#23565,#23566,
#23567,#23568,#23569,#23570,#23571,#23572,#23573,#23574,#23575,#23576,#23577,
#23578,#23579,#23580,#23581,#23582,#23583,#23584,#23585,#23586,#23587,#23588,
#23589,#23590,#23591,#23592,#23593,#23594,#23595,#23596,#23597,#23598,#23599,
#23600,#23601,#23602,#23603,#23604,#23605,#23606,#23607,#23608,#23609,#23610,
#23611,#23612,#23613,#23614,#23615,#23616,#23617,#23618,#23619,#23620,#23621,
#23622,#23623,#23624,#23625,#23626,#23627,#23628,#23629,#23630,#23631,#23632,
#23633,#23634,#23635,#23636,#23637,#23638,#23639,#23640,#23641,#23642,#23643,
#23644,#23645,#23646,#23647,#23648,#23649,#23650,#23651,#23652,#23653,#23654,
#23655,#23656,#23657,#23658,#23659,#23660,#23661,#23662,#23663,#23664,#23665,
#23666,#23667,#23668,#23669,#23670,#23671,#23672,#23673,#23674,#23675,#23676,
#23677,#23678,#23679,#23680,#23681,#23682,#23683,#23684,#23685,#23686,#23687,
#23688,#23689,#23690,#23691,#23692,#23693,#23694,#23695,#23696,#23697,#23698,
#23699,#23700,#23701,#23702,#23703,#23704,#23705,#23706,#23707,#23708,#23709,
#23710,#23711,#23712,#23713,#23714,#23715,#23716,#23717,#23718,#23719,#23720,
#23721,#23722,#23723,#23724,#23725,#23726,#23727,#23728,#23729,#23730,#23731,
#23732,#23733,#23734,#23735,#23736,#23737,#23738,#23739,#23740,#23741,#23742,
#23743,#23744,#23745,#23746,#23747,#23748,#23749),(#23750,#23751,#23752,
#23753,#23754,#23755,#23756,#23757,#23758,#23759,#23760,#23761,#23762,#23763,
#23764,#23765,#23766,#23767,#23768,#23769,#23770,#23771,#23772,#23773,#23774,
#23775,#23776,#23777,#23778,#23779,#23780,#23781,#23782,#23783,#23784,#23785,
#23786,#23787,#23788,#23789,#23790,#23791,#23792,#23793,#23794,#23795,#23796,
#23797,#23798,#23799,#23800,#23801,#23802,#23803,#23804,#23805,#23806,#23807,
#23808,#23809,#23810,#23811,#23812,#23813,#23814,#23815,#23816,#23817,#23818,
#23819,#23820,#23821,#23822,#23823,#23824,#23825,#23826,#23827,#23828,#23829,
#23830,#23831,#23832,#23833,#23834,#23835,#23836,#23837,#23838,#23839,#23840,
#23841,#23842,#23843,#23844,#23845,#23846,#23847,#23848,#23849,#23850,#23851,
#23852,#23853,#23854,#23855,#23856,#23857,#23858,#23859,#23860,#23861,#23862,
#23863,#23864,#23865,#23866,#23867,#23868,#23869,#23870,#23871,#23872,#23873,
#23874,#23875,#23876,#23877,#23878,#23879,#23880,#23881,#23882,#23883,#23884,
#23885,#23886,#23887,#23888,#23889,#23890,#23891,#23892,#23893,#23894,#23895,
#23896,#23897,#23898,#23899,#23900,#23901,#23902,#23903,#23904,#23905,#23906,
#23907,#23908,#23909,#23910,#23911,#23912,#23913,#23914,#23915,#23916,#23917,
#23918,#23919,#23920,#23921,#23922,#23923,#23924,#23925,#23926,#23927,#23928,
#23929,#23930,#23931,#23932,#23933,#23934,#23935,#23936,#23937,#23938,#23939,
#23940,#23941,#23942,#23943,#23944,#23945,#23946,#23947,#23948,#23949,#23950,
#23951,#23952,#23953,#23954,#23955,#23956,#23957,#23958,#23959,#23960,#23961,
#23962,#23963,#23964,#23965,#23966,#23967,#23968,#23969,#23970,#23971,#23972,
#23973,#23974,#23975,#23976,#23977,#23978,#23979,#23980,#23981,#23982,#23983,
#23984,#23985,#23986,#23987,#23988,#23989,#23990,#23991,#23992,#23993,#23994,
#23995,#23996,#23997,#23998,#23999,#24000,#24001,#24002,#24003,#24004,#24005,
#24006,#24007,#24008,#24009,#24010,#24011,#24012,#24013,#24014,#24015,#24016,
#24017,#24018,#24019,#24020,#24021,#24022,#24023,#24024,#24025,#24026,#24027,
#24028,#24029,#24030,#24031,#24032,#24033,#24034,#24035,#24036,#24037,#24038,
#24039,#24040,#24041,#24042,#24043,#24044,#24045,#24046,#24047,#24048,#24049,
#24050,#24051,#24052,#24053,#24054,#24055,#24056,#24057,#24058,#24059,#24060,
#24061,#24062,#24063,#24064,#24065,#24066,#24067,#24068,#24069,#24070,#24071,
#24072,#24073,#24074,#24075,#24076,#24077,#24078,#24079,#24080,#24081,#24082,
#24083,#24084,#24085,#24086,#24087,#24088,#24089,#24090,#24091,#24092,#24093,
#24094,#24095,#24096,#24097,#24098,#24099,#24100,#24101,#24102,#24103,#24104,
#24105,#24106,#24107,#24108,#24109,#24110,#24111,#24112,#24113,#24114,#24115,
#24116,#24117,#24118,#24119,#24120,#24121,#24122,#24123,#24124,#24125,#24126,
#24127,#24128,#24129,#24130,#24131,#24132,#24133,#24134,#24135,#24136,#24137,
#24138,#24139,#24140,#24141,#24142,#24143,#24144,#24145,#24146,#24147,#24148,
#24149,#24150,#24151,#24152,#24153,#24154,#24155,#24156,#24157,#24158,#24159,
#24160,#24161,#24162,#24163,#24164,#24165,#24166,#24167,#24168,#24169,#24170,
#24171,#24172,#24173,#24174,#24175,#24176,#24177,#24178,#24179,#24180,#24181,
#24182,#24183,#24184,#24185,#24186,#24187,#24188,#24189,#24190,#24191,#24192,
#24193,#24194,#24195,#24196,#24197,#24198,#24199,#24200,#24201,#24202,#24203,
#24204,#24205,#24206,#24207,#24208,#24209,#24210,#24211,#24212,#24213,#24214,
#24215,#24216,#24217,#24218,#24219,#24220,#24221,#24222,#24223,#24224,#24225,
#24226,#24227,#24228,#24229,#24230,#24231,#24232,#24233,#24234,#24235,#24236,
#24237,#24238,#24239,#24240,#24241,#24242,#24243,#24244,#24245,#24246,#24247,
#24248,#24249,#24250,#24251,#24252,#24253,#24254,#24255,#24256,#24257,#24258,
#24259,#24260,#24261,#24262,#24263,#24264,#24265,#24266,#24267,#24268,#24269,
#24270,#24271,#24272,#24273,#24274,#24275,#24276,#24277,#24278,#24279,#24280,
#24281,#24282,#24283,#24284,#24285,#24286,#24287,#24288,#24289,#24290,#24291,
#24292,#24293,#24294,#24295,#24296,#24297,#24298,#24299,#24300,#24301,#24302,
#24303,#24304,#24305,#24306,#24307,#24308,#24309,#24310,#24311,#24312,#24313,
#24314,#24315,#24316,#24317,#24318,#24319,#24320,#24321,#24322,#24323,#24324,
#24325,#24326,#24327,#24328,#24329,#24330,#24331,#24332,#24333,#24334,#24335,
#24336,#24337,#24338,#24339,#24340,#24341,#24342,#24343,#24344,#24345,#24346,
#24347,#24348,#24349,#24350,#24351,#24352,#24353,#24354,#24355,#24356,#24357,
#24358,#24359,#24360,#24361,#24362,#24363,#24364,#24365,#24366,#24367,#24368,
#24369,#24370,#24371,#24372,#24373,#24374,#24375,#24376,#24377,#24378,#24379,
#24380,#24381,#24382,#24383,#24384,#24385,#24386,#24387,#24388,#24389,#24390,
#24391,#24392,#24393,#24394,#24395,#24396,#24397,#24398,#24399,#24400,#24401,
#24402,#24403,#24404,#24405,#24406,#24407,#24408,#24409,#24410,#24411,#24412,
#24413,#24414,#24415,#24416,#24417,#24418,#24419,#24420,#24421,#24422,#24423,
#24424,#24425,#24426,#24427,#24428,#24429,#24430,#24431),(#24432,#24433,
#24434,#24435,#24436,#24437,#24438,#24439,#24440,#24441,#24442,#24443,#24444,
#24445,#24446,#24447,#24448,#24449,#24450,#24451,#24452,#24453,#24454,#24455,
#24456,#24457,#24458,#24459,#24460,#24461,#24462,#24463,#24464,#24465,#24466,
#24467,#24468,#24469,#24470,#24471,#24472,#24473,#24474,#24475,#24476,#24477,
#24478,#24479,#24480,#24481,#24482,#24483,#24484,#24485,#24486,#24487,#24488,
#24489,#24490,#24491,#24492,#24493,#24494,#24495,#24496,#24497,#24498,#24499,
#24500,#24501,#24502,#24503,#24504,#24505,#24506,#24507,#24508,#24509,#24510,
#24511,#24512,#24513,#24514,#24515,#24516,#24517,#24518,#24519,#24520,#24521,
#24522,#24523,#24524,#24525,#24526,#24527,#24528,#24529,#24530,#24531,#24532,
#24533,#24534,#24535,#24536,#24537,#24538,#24539,#24540,#24541,#24542,#24543,
#24544,#24545,#24546,#24547,#24548,#24549,#24550,#24551,#24552,#24553,#24554,
#24555,#24556,#24557,#24558,#24559,#24560,#24561,#24562,#24563,#24564,#24565,
#24566,#24567,#24568,#24569,#24570,#24571,#24572,#24573,#24574,#24575,#24576,
#24577,#24578,#24579,#24580,#24581,#24582,#24583,#24584,#24585,#24586,#24587,
#24588,#24589,#24590,#24591,#24592,#24593,#24594,#24595,#24596,#24597,#24598,
#24599,#24600,#24601,#24602,#24603,#24604,#24605,#24606,#24607,#24608,#24609,
#24610,#24611,#24612,#24613,#24614,#24615,#24616,#24617,#24618,#24619,#24620,
#24621,#24622,#24623,#24624,#24625,#24626,#24627,#24628,#24629,#24630,#24631,
#24632,#24633,#24634,#24635,#24636,#24637,#24638,#24639,#24640,#24641,#24642,
#24643,#24644,#24645,#24646,#24647,#24648,#24649,#24650,#24651,#24652,#24653,
#24654,#24655,#24656,#24657,#24658,#24659,#24660,#24661,#24662,#24663,#24664,
#24665,#24666,#24667,#24668,#24669,#24670,#24671,#24672,#24673,#24674,#24675,
#24676,#24677,#24678,#24679,#24680,#24681,#24682,#24683,#24684,#24685,#24686,
#24687,#24688,#24689,#24690,#24691,#24692,#24693,#24694,#24695,#24696,#24697,
#24698,#24699,#24700,#24701,#24702,#24703,#24704,#24705,#24706,#24707,#24708,
#24709,#24710,#24711,#24712,#24713,#24714,#24715,#24716,#24717,#24718,#24719,
#24720,#24721,#24722,#24723,#24724,#24725,#24726,#24727,#24728,#24729,#24730,
#24731,#24732,#24733,#24734,#24735,#24736,#24737,#24738,#24739,#24740,#24741,
#24742,#24743,#24744,#24745,#24746,#24747,#24748,#24749,#24750,#24751,#24752,
#24753,#24754,#24755,#24756,#24757,#24758,#24759,#24760,#24761,#24762,#24763,
#24764,#24765,#24766,#24767,#24768,#24769,#24770,#24771,#24772,#24773,#24774,
#24775,#24776,#24777,#24778,#24779,#24780,#24781,#24782,#24783,#24784,#24785,
#24786,#24787,#24788,#24789,#24790,#24791,#24792,#24793,#24794,#24795,#24796,
#24797,#24798,#24799,#24800,#24801,#24802,#24803,#24804,#24805,#24806,#24807,
#24808,#24809,#24810,#24811,#24812,#24813,#24814,#24815,#24816,#24817,#24818,
#24819,#24820,#24821,#24822,#24823,#24824,#24825,#24826,#24827,#24828,#24829,
#24830,#24831,#24832,#24833,#24834,#24835,#24836,#24837,#24838,#24839,#24840,
#24841,#24842,#24843,#24844,#24845,#24846,#24847,#24848,#24849,#24850,#24851,
#24852,#24853,#24854,#24855,#24856,#24857,#24858,#24859,#24860,#24861,#24862,
#24863,#24864,#24865,#24866,#24867,#24868,#24869,#24870,#24871,#24872,#24873,
#24874,#24875,#24876,#24877,#24878,#24879,#24880,#24881,#24882,#24883,#24884,
#24885,#24886,#24887,#24888,#24889,#24890,#24891,#24892,#24893,#24894,#24895,
#24896,#24897,#24898,#24899,#24900,#24901,#24902,#24903,#24904,#24905,#24906,
#24907,#24908,#24909,#24910,#24911,#24912,#24913,#24914,#24915,#24916,#24917,
#24918,#24919,#24920,#24921,#24922,#24923,#24924,#24925,#24926,#24927,#24928,
#24929,#24930,#24931,#24932,#24933,#24934,#24935,#24936,#24937,#24938,#24939,
#24940,#24941,#24942,#24943,#24944,#24945,#24946,#24947,#24948,#24949,#24950,
#24951,#24952,#24953,#24954,#24955,#24956,#24957,#24958,#24959,#24960,#24961,
#24962,#24963,#24964,#24965,#24966,#24967,#24968,#24969,#24970,#24971,#24972,
#24973,#24974,#24975,#24976,#24977,#24978,#24979,#24980,#24981,#24982,#24983,
#24984,#24985,#24986,#24987,#24988,#24989,#24990,#24991,#24992,#24993,#24994,
#24995,#24996,#24997,#24998,#24999,#25000,#25001,#25002,#25003,#25004,#25005,
#25006,#25007,#25008,#25009,#25010,#25011,#25012,#25013,#25014,#25015,#25016,
#25017,#25018,#25019,#25020,#25021,#25022,#25023,#25024,#25025,#25026,#25027,
#25028,#25029,#25030,#25031,#25032,#25033,#25034,#25035,#25036,#25037,#25038,
#25039,#25040,#25041,#25042,#25043,#25044,#25045,#25046,#25047,#25048,#25049,
#25050,#25051,#25052,#25053,#25054,#25055,#25056,#25057,#25058,#25059,#25060,
#25061,#25062,#25063,#25064,#25065,#25066,#25067,#25068,#25069,#25070,#25071,
#25072,#25073,#25074,#25075,#25076,#25077,#25078,#25079,#25080,#25081,#25082,
#25083,#25084,#25085,#25086,#25087,#25088,#25089,#25090,#25091,#25092,#25093,
#25094,#25095,#25096,#25097,#25098,#25099,#25100,#25101,#25102,#25103,#25104,
#25105,#25106,#25107,#25108,#25109,#25110,#25111,#25112,#25113)),
 .UNSPECIFIED.,.F.,.F.,.F.,(4,4),(4,1,1,1,1,1,1,1,1,1,1,1,1,1,1,1,1,1,1,
1,1,1,1,1,1,1,1,1,1,1,1,1,1,1,1,1,1,1,1,1,1,1,1,1,1,1,1,1,1,1,1,1,1,1,1,
1,1,1,1,1,1,1,1,1,1,1,1,1,1,1,1,1,1,1,1,1,1,1,1,1,1,1,1,1,1,1,1,1,1,1,1,
1,1,1,1,1,1,1,1,1,1,1,1,1,1,1,1,1,1,1,1,1,1,1,1,1,1,1,1,1,1,1,1,1,1,1,1,
1,1,1,1,1,1,1,1,1,1,1,1,1,1,1,1,1,1,1,1,1,1,1,1,1,1,1,1,1,1,1,1,1,1,1,1,
1,1,1,1,1,1,1,1,1,1,1,1,1,1,1,1,1,1,1,1,1,1,1,1,1,1,1,1,1,1,1,1,1,1,1,1,
1,1,1,1,1,1,1,1,1,1,1,1,1,1,1,1,1,1,1,1,1,1,1,1,1,1,1,1,1,1,1,1,1,1,1,1,
1,1,1,1,1,1,1,1,1,1,1,1,1,1,1,1,1,1,1,1,1,1,1,1,1,1,1,1,1,1,1,1,1,1,1,1,
1,1,1,1,1,1,1,1,1,1,1,1,1,1,1,1,1,1,1,1,1,1,1,1,1,1,1,1,1,1,1,1,1,1,1,1,
1,1,1,1,1,1,1,1,1,1,1,1,1,1,1,1,1,1,1,1,1,1,1,1,1,1,1,1,1,1,1,1,1,1,1,1,
1,1,1,1,1,1,1,1,1,1,1,1,1,1,1,1,1,1,1,1,1,1,1,1,1,1,1,1,1,1,1,1,1,1,1,1,
1,1,1,1,1,1,1,1,1,1,1,1,1,1,1,1,1,1,1,1,1,1,1,1,1,1,1,1,1,1,1,1,1,1,1,1,
1,1,1,1,1,1,1,1,1,1,1,1,1,1,1,1,1,1,1,1,1,1,1,1,1,1,1,1,1,1,1,1,1,1,1,1,
1,1,1,1,1,1,1,1,1,1,1,1,1,1,1,1,1,1,1,1,1,1,1,1,1,1,1,1,1,1,1,1,1,1,1,1,
1,1,1,1,1,1,1,1,1,1,1,1,1,1,1,1,1,1,1,1,1,1,1,1,1,1,1,1,1,1,1,1,1,1,1,1,
1,1,1,1,1,1,1,1,1,1,1,1,1,1,1,1,1,1,1,1,1,1,1,1,1,1,1,1,1,1,1,1,1,1,1,1,
1,1,1,1,1,1,1,1,1,1,1,1,1,1,1,1,1,1,1,1,1,1,1,1,1,1,1,1,1,1,1,1,1,1,1,1,
1,1,1,1,1,1,1,1,1,1,1,1,1,1,1,1,1,1,1,1,1,1,1,1,1,1,1,1,1,1,1,1,1,1,1,1,
1,1,1,1,1,1,1,1,1,1,1,1,1,1,1,1,1,1,1,1,1,1,1,1,1,1,1,1,1,1,1,1,1,1,1,1,
1,1,1,1,1,1,1,1,1,1,1,1,4),(0.,0.198319817466637),(8.29931545526329,8.79905931626407,
9.29880317726486,10.2982908992664,11.297778621268,12.2972663432696,12.7970102042703,
13.2967540652711,14.2962417872727,15.2957295092743,16.2952172312758,17.2947049532774,
18.294192675279,18.7939365362798,19.2936803972805,20.2931681192821,21.2926558412837,
22.2921435632852,23.2916312852868,24.2911190072884,25.2906067292899,25.7903505902907,
26.2900944512915,27.2895821732931,28.2890698952946,29.2885576172962,30.2880453392978,
31.2875330612993,32.2870207833009,32.7867646443017,33.2865085053025,34.2859962273041,
35.2854839493056,36.2849716713072,37.2844593933088,38.2839471153103,39.2834348373119,
39.7831786983127,40.2829225593135,41.282410281315,42.2818980033166,43.2813857253182,
44.2808734473197,45.2803611693213,46.2798488913229,46.7795927523237,47.2793366133244,
48.278824335326,49.2783120573276,50.2777997793291,51.2772875013307,52.2767752233323,
53.2762629453338,53.7760068063346,54.2757506673354,55.275238389337,56.2747261113385,
57.2742138333401,58.2737015553417,59.2731892773432,60.2726769993448,60.7724208603456,
61.2721647213464,62.2716524433479,63.2711401653495,64.2706278873511,65.2701156093526,
66.2696033313542,67.2690910533558,67.7688349143566,68.2685787753574,69.2680664973589,
70.2675542193605,71.2670419413621,72.2665296633636,73.2660173853652,74.2655051073667,
74.7652489683675,75.2649928293683,76.2644805513699,77.2639682733715,78.263455995373,
79.2629437173746,80.2624314393762,81.2619191613777,81.7616630223785,82.2614068833793,
83.2608946053809,84.2603823273824,85.259870049384,86.2593577713856,87.2588454933872,
88.2583332153887,88.7580770763895,89.2578209373903,90.2573086593918,91.2567963813934,
92.256284103395,93.2557718253966,94.2552595473981,95.2547472693997,95.7544911304005,
96.2542349914013,97.2537227134028,98.2532104354044,99.2526981574059,100.252185879408,
101.251673601409,102.251161323411,102.750905184411,103.250649045412,104.250136767414,
105.249624489415,106.249112211417,107.248599933418,108.24808765542,109.247575377422,
109.747319238422,110.247063099423,111.246550821425,112.246038543426,113.245526265428,
114.245013987429,115.244501709431,116.243989431433,116.743733292433,117.243477153434,
118.242964875436,119.242452597437,120.241940319439,121.24142804144,122.240915763442,
123.240403485444,123.740147346444,124.239891207445,125.239378929447,126.238866651448,
127.23835437345,128.237842095451,129.237329817453,130.236817539455,130.736561400455,
131.236305261456,132.235792983458,133.235280705459,134.234768427461,135.234256149462,
136.233743871464,137.233231593466,137.732975454466,138.232719315467,139.232207037469,
140.23169475947,141.231182481472,142.230670203473,143.230157925475,144.229645647477,
144.729389508477,145.229133369478,146.22862109148,147.228108813481,148.227596535483,
149.227084257484,150.226571979486,151.226059701487,151.725803562488,152.225547423489,
153.225035145491,154.224522867492,155.224010589494,156.223498311495,157.222986033497,
158.222473755498,158.722217616499,159.2219614775,160.221449199502,161.220936921503,
162.220424643505,163.219912365506,164.219400087508,165.218887809509,165.71863167051,
166.218375531511,167.217863253513,168.217350975514,169.216838697516,170.216326419517,
171.215814141519,172.21530186352,172.715045724521,173.214789585522,174.214277307524,
175.213765029525,176.213252751527,177.212740473528,178.21222819553,179.211715917531,
179.711459778532,180.211203639533,181.210691361535,182.210179083536,183.209666805538,
184.209154527539,185.208642249541,186.208129971542,186.707873832543,187.207617693544,
188.207105415545,189.206593137547,190.206080859549,191.20556858155,192.205056303552,
193.204544025553,193.704287886554,194.204031747555,195.203519469556,196.203007191558,
197.20249491356,198.201982635561,199.201470357563,200.200958079564,200.700701940565,
201.200445801566,202.199933523567,203.199421245569,204.198908967571,205.198396689572,
206.197884411574,207.197372133575,207.697115994576,208.196859855577,209.196347577578,
210.19583529958,211.195323021582,212.194810743583,213.194298465585,214.193786187586,
214.693530048587,215.193273909588,216.192761631589,217.192249353591,218.191737075593,
219.191224797594,220.190712519596,221.190200241597,221.689944102598,222.189687963599,
223.1891756856,224.188663407602,225.188151129604,226.187638851605,227.187126573607,
228.186614295608,228.686358156609,229.18610201761,230.185589739611,231.185077461613,
232.184565183614,233.184052905616,234.183540627618,235.183028349619,235.68277221062,
236.182516071621,237.182003793622,238.181491515624,239.180979237625,240.180466959627,
241.179954681629,242.17944240363,242.679186264631,243.178930125632,244.178417847633,
245.177905569635,246.177393291636,247.176881013638,248.17636873564,249.175856457641,
249.675600318642,250.175344179643,251.174831901644,252.174319623646,253.173807345647,
254.173295067649,255.172782789651,256.172270511652,256.672014372653,257.171758233654,
258.171245955655,259.170733677657,260.170221399658,261.16970912166,262.169196843661,
263.168684565663,263.668428426664,264.168172287665,265.167660009666,266.167147731668,
267.166635453669,268.166123175671,269.165610897672,270.165098619674,270.664842480675,
271.164586341676,272.164074063677,273.163561785679,274.16304950768,275.162537229682,
276.162024951683,277.161512673685,277.661256534686,278.161000395687,279.160488117688,
280.15997583969,281.159463561691,282.158951283693,283.158439005694,284.157926727696,
284.657670588697,285.157414449698,286.156902171699,287.156389893701,288.155877615702,
289.155365337704,290.154853059705,291.154340781707,291.654084642708,292.153828503709,
293.15331622571,294.152803947712,295.152291669713,296.151779391715,297.151267113716,
298.150754835718,298.650498696719,299.15024255772,300.149730279721,301.149218001723,
302.148705723724,303.148193445726,304.147681167727,305.147168889729,306.146656611731,
307.146144333732,308.145632055734,309.145119777735,310.144607499737,310.644351360738,
311.144095221738,312.14358294374,313.143070665741,314.142558387743,315.142046109745,
316.141533831746,317.141021553748,317.640765414749,318.140509275749,319.139996997751,
320.139484719752,321.138972441754,322.138460163756,323.137947885757,324.137435607759,
324.63717946876,325.13692332976,326.136411051762,327.135898773763,328.135386495765,
329.134874217767,330.134361939768,331.13384966177,331.63359352277,332.133337383771,
333.132825105773,334.132312827774,335.131800549776,336.131288271778,337.130775993779,
338.130263715781,338.630007576781,339.129751437782,340.129239159784,341.128726881785,
342.128214603787,343.127702325789,344.12719004779,345.126677769792,345.626421630792,
346.126165491793,347.125653213795,348.125140935796,349.124628657798,350.124116379799,
351.123604101801,352.123091823803,352.622835684803,353.122579545804,354.122067267806,
355.121554989807,356.121042711809,357.12053043381,358.120018155812,359.119505877814,
359.619249738814,360.118993599815,361.118481321817,362.117969043818,363.11745676582,
364.116944487821,365.116432209823,366.115919931825,366.615663792825,367.115407653826,
368.114895375828,369.114383097829,370.113870819831,371.113358541832,372.112846263834,
373.112333985836,373.612077846836,374.111821707837,375.111309429839,376.11079715184,
377.110284873842,378.109772595843,379.109260317845,380.108748039846,380.608491900847,
381.108235761848,382.10772348385,383.107211205851,384.106698927853,385.106186649854,
386.105674371856,387.105162093857,387.604905954858,388.104649815859,389.104137537861,
390.103625259862,391.103112981864,392.102600703865,393.102088425867,394.101576147868,
394.601320008869,395.10106386987,396.100551591872,397.100039313873,398.099527035875,
399.099014757876,400.098502479878,401.097990201879,401.59773406288,402.097477923881,
403.096965645883,404.096453367884,405.095941089886,406.095428811887,407.094916533889,
408.09440425589,408.594148116891,409.093891977892,410.093379699894,411.092867421895,
412.092355143897,413.091842865898,414.0913305879,415.090818309901,415.590562170902,
416.090306031903,417.089793753905,418.089281475906,419.088769197908,420.088256919909,
421.087744641911,422.087232363912,422.586976224913,423.086720085914,424.086207807916,
425.085695529917,426.085183251919,427.08467097392,428.084158695922,429.083646417923,
429.583390278924,430.083134139925,431.082621861926,432.082109583928,433.08159730593,
434.081085027931,435.080572749933,436.080060471934,436.579804332935,437.079548193936,
438.079035915937,439.078523637939,440.078011359941,441.077499081942,442.076986803944,
443.076474525945,443.576218386946,444.075962247947,445.075449969948,446.07493769195,
447.074425413952,448.073913135953,449.073400857955,450.072888579956,450.572632440957,
451.072376301958,452.071864023959,453.071351745961,454.070839467963,455.070327189964,
456.069814911966,457.069302633967,457.569046494968,458.068790355969,459.06827807797,
460.067765799972,461.067253521973,462.066741243975,463.066228965977,464.065716687978,
464.565460548979,465.06520440998,466.064692131981,467.064179853983,468.063667575984,
469.063155297986,470.062643019988,471.062130741989,471.56187460299,472.061618463991,
473.061106185992,474.060593907994,475.060081629995,476.059569351997,477.059057073999,
478.058544796,478.558288657001,479.058032518002,480.057520240003,481.057007962005,
482.056495684006,483.055983406008,484.05547112801,485.054958850011,485.554702711012,
486.054446572013,487.053934294014,488.053422016016,489.052909738017,490.052397460019,
491.051885182021,492.051372904022,492.551116765023,493.050860626024,494.050348348025,
495.049836070027,496.049323792028,497.04881151403,498.048299236031,499.047786958033,
499.547530819034,500.047274680035,501.046762402036,502.046250124038,503.045737846039,
504.045225568041,505.044713290042,506.044201012044,506.543944873045,507.043688734046,
508.043176456047,509.042664178049,510.04215190005,511.041639622052,512.041127344053,
513.040615066055,513.540358927056,514.040102788057,515.039590510058,516.03907823206,
517.038565954061,518.038053676063,519.037541398064,520.037029120066,520.536772981067,
521.036516842067,522.036004564069,523.035492286071,524.034980008072,525.034467730074,
526.033955452075,527.033443174077,527.533187035078,528.032930896078,529.03241861808,
530.031906340082,531.031394062083,532.030881784085,533.030369506086,534.029857228088,
534.529601089089,535.029344950089,536.028832672091,537.028320394093,538.027808116094,
539.027295838096,540.026783560097,541.026271282099,541.5260151431,542.0257590041,
543.025246726102,544.024734448104,545.024222170105,546.023709892107,547.023197614108,
548.02268533611,548.522429197111,549.022173058111,550.021660780113,551.021148502115,
552.020636224116,553.020123946118,554.019611668119,555.019099390121,555.518843251122,
556.018587112122,557.018074834124,558.017562556126,559.017050278127,560.016538000129,
561.01602572213,562.015513444132,562.515257305133,563.015001166133,564.014488888135,
565.013976610137,566.013464332138,567.01295205414,568.012439776141,569.011927498143,
569.511671359144,570.011415220144,571.010902942146,572.010390664148,573.009878386149,
574.009366108151,575.008853830152,576.008341552154,576.508085413155,577.007829274155,
578.007316996157,579.006804718158,580.00629244016,581.005780162162,582.005267884163,
583.004755606165,583.504499467165,584.004243328166,585.003731050168,586.003218772169,
587.002706494171,588.002194216173,589.001681938174,590.001169660176,590.500913521176,
591.000657382177,592.000145104179,592.99963282618,593.999120548182,594.998608270183,
595.998095992185,596.497839853186,596.997583714187,597.997071436188,598.99655915819,
599.996046880191,600.495790741192,600.995534602193),.UNSPECIFIED.);
#208=B_SPLINE_SURFACE_WITH_KNOTS('',3,3,((#25249,#25250,#25251,#25252,#25253,
#25254,#25255,#25256,#25257,#25258,#25259,#25260,#25261,#25262,#25263,#25264,
#25265,#25266,#25267,#25268,#25269,#25270,#25271,#25272,#25273,#25274,#25275,
#25276,#25277,#25278,#25279,#25280,#25281,#25282,#25283,#25284,#25285,#25286,
#25287,#25288,#25289,#25290,#25291,#25292,#25293,#25294,#25295,#25296,#25297,
#25298,#25299,#25300,#25301,#25302,#25303,#25304,#25305,#25306,#25307,#25308,
#25309,#25310,#25311,#25312,#25313,#25314,#25315,#25316,#25317,#25318,#25319,
#25320,#25321,#25322,#25323,#25324,#25325,#25326,#25327,#25328,#25329,#25330,
#25331,#25332,#25333,#25334,#25335,#25336,#25337,#25338,#25339,#25340,#25341,
#25342,#25343,#25344,#25345,#25346,#25347,#25348,#25349,#25350,#25351,#25352,
#25353,#25354,#25355,#25356,#25357,#25358,#25359,#25360,#25361,#25362,#25363,
#25364,#25365,#25366,#25367,#25368,#25369,#25370,#25371,#25372,#25373,#25374,
#25375,#25376,#25377,#25378,#25379,#25380,#25381,#25382,#25383,#25384,#25385,
#25386,#25387,#25388,#25389,#25390,#25391,#25392,#25393,#25394,#25395,#25396,
#25397,#25398,#25399,#25400,#25401,#25402,#25403,#25404,#25405,#25406,#25407,
#25408,#25409,#25410,#25411,#25412,#25413,#25414,#25415,#25416,#25417,#25418,
#25419,#25420,#25421,#25422,#25423,#25424,#25425,#25426,#25427,#25428,#25429,
#25430,#25431,#25432,#25433,#25434,#25435,#25436,#25437,#25438,#25439,#25440,
#25441,#25442,#25443,#25444,#25445,#25446,#25447,#25448,#25449,#25450,#25451,
#25452,#25453,#25454,#25455,#25456,#25457,#25458,#25459,#25460,#25461,#25462,
#25463,#25464,#25465,#25466,#25467,#25468,#25469,#25470,#25471,#25472,#25473,
#25474,#25475,#25476,#25477,#25478,#25479,#25480,#25481,#25482,#25483,#25484,
#25485,#25486,#25487,#25488,#25489,#25490,#25491,#25492,#25493,#25494,#25495,
#25496,#25497,#25498,#25499,#25500,#25501,#25502,#25503,#25504,#25505,#25506,
#25507,#25508,#25509,#25510,#25511,#25512,#25513,#25514,#25515,#25516,#25517,
#25518,#25519,#25520,#25521,#25522,#25523,#25524,#25525,#25526,#25527,#25528,
#25529,#25530,#25531,#25532,#25533,#25534,#25535,#25536,#25537,#25538,#25539,
#25540,#25541,#25542,#25543,#25544,#25545,#25546,#25547,#25548,#25549,#25550,
#25551,#25552,#25553,#25554,#25555,#25556,#25557,#25558,#25559,#25560,#25561,
#25562,#25563,#25564,#25565,#25566,#25567,#25568,#25569,#25570,#25571,#25572,
#25573,#25574,#25575,#25576,#25577,#25578,#25579,#25580,#25581,#25582,#25583,
#25584,#25585,#25586,#25587,#25588,#25589,#25590,#25591,#25592,#25593,#25594,
#25595,#25596,#25597,#25598,#25599,#25600,#25601,#25602,#25603,#25604,#25605,
#25606,#25607,#25608,#25609,#25610,#25611,#25612,#25613,#25614,#25615,#25616,
#25617,#25618,#25619,#25620,#25621,#25622,#25623,#25624,#25625,#25626,#25627,
#25628,#25629,#25630,#25631,#25632,#25633,#25634,#25635,#25636,#25637,#25638,
#25639,#25640,#25641,#25642,#25643,#25644,#25645,#25646,#25647,#25648,#25649,
#25650,#25651,#25652,#25653,#25654,#25655,#25656,#25657,#25658,#25659,#25660,
#25661,#25662,#25663,#25664,#25665,#25666,#25667,#25668,#25669,#25670,#25671,
#25672,#25673,#25674,#25675,#25676,#25677,#25678,#25679,#25680,#25681,#25682,
#25683,#25684,#25685,#25686,#25687,#25688,#25689,#25690,#25691,#25692,#25693,
#25694,#25695,#25696,#25697,#25698,#25699,#25700,#25701,#25702,#25703,#25704,
#25705,#25706,#25707,#25708,#25709,#25710,#25711,#25712,#25713,#25714,#25715,
#25716,#25717,#25718,#25719,#25720,#25721,#25722,#25723,#25724,#25725,#25726,
#25727,#25728,#25729,#25730,#25731,#25732,#25733,#25734,#25735,#25736,#25737,
#25738,#25739,#25740,#25741,#25742,#25743,#25744,#25745,#25746,#25747,#25748,
#25749,#25750,#25751,#25752,#25753,#25754,#25755,#25756,#25757,#25758,#25759,
#25760,#25761,#25762,#25763,#25764,#25765,#25766,#25767,#25768,#25769,#25770,
#25771,#25772,#25773,#25774,#25775,#25776,#25777,#25778,#25779,#25780,#25781,
#25782,#25783,#25784,#25785,#25786,#25787,#25788,#25789,#25790,#25791,#25792,
#25793,#25794,#25795,#25796,#25797,#25798,#25799,#25800,#25801,#25802,#25803,
#25804,#25805,#25806,#25807,#25808,#25809,#25810,#25811,#25812,#25813,#25814,
#25815,#25816,#25817,#25818,#25819,#25820,#25821,#25822,#25823,#25824,#25825,
#25826,#25827,#25828,#25829,#25830,#25831,#25832,#25833,#25834,#25835,#25836,
#25837,#25838,#25839,#25840,#25841,#25842,#25843,#25844,#25845,#25846,#25847,
#25848,#25849,#25850,#25851,#25852,#25853,#25854,#25855,#25856,#25857,#25858,
#25859,#25860,#25861,#25862,#25863,#25864,#25865,#25866,#25867,#25868,#25869,
#25870,#25871,#25872,#25873,#25874,#25875,#25876,#25877,#25878,#25879,#25880,
#25881,#25882,#25883,#25884,#25885,#25886,#25887,#25888,#25889,#25890,#25891,
#25892,#25893,#25894,#25895,#25896,#25897,#25898,#25899,#25900,#25901,#25902,
#25903,#25904,#25905,#25906,#25907,#25908,#25909,#25910,#25911,#25912,#25913,
#25914,#25915,#25916,#25917,#25918,#25919,#25920,#25921,#25922,#25923,#25924,
#25925,#25926,#25927,#25928,#25929,#25930),(#25931,#25932,#25933,#25934,
#25935,#25936,#25937,#25938,#25939,#25940,#25941,#25942,#25943,#25944,#25945,
#25946,#25947,#25948,#25949,#25950,#25951,#25952,#25953,#25954,#25955,#25956,
#25957,#25958,#25959,#25960,#25961,#25962,#25963,#25964,#25965,#25966,#25967,
#25968,#25969,#25970,#25971,#25972,#25973,#25974,#25975,#25976,#25977,#25978,
#25979,#25980,#25981,#25982,#25983,#25984,#25985,#25986,#25987,#25988,#25989,
#25990,#25991,#25992,#25993,#25994,#25995,#25996,#25997,#25998,#25999,#26000,
#26001,#26002,#26003,#26004,#26005,#26006,#26007,#26008,#26009,#26010,#26011,
#26012,#26013,#26014,#26015,#26016,#26017,#26018,#26019,#26020,#26021,#26022,
#26023,#26024,#26025,#26026,#26027,#26028,#26029,#26030,#26031,#26032,#26033,
#26034,#26035,#26036,#26037,#26038,#26039,#26040,#26041,#26042,#26043,#26044,
#26045,#26046,#26047,#26048,#26049,#26050,#26051,#26052,#26053,#26054,#26055,
#26056,#26057,#26058,#26059,#26060,#26061,#26062,#26063,#26064,#26065,#26066,
#26067,#26068,#26069,#26070,#26071,#26072,#26073,#26074,#26075,#26076,#26077,
#26078,#26079,#26080,#26081,#26082,#26083,#26084,#26085,#26086,#26087,#26088,
#26089,#26090,#26091,#26092,#26093,#26094,#26095,#26096,#26097,#26098,#26099,
#26100,#26101,#26102,#26103,#26104,#26105,#26106,#26107,#26108,#26109,#26110,
#26111,#26112,#26113,#26114,#26115,#26116,#26117,#26118,#26119,#26120,#26121,
#26122,#26123,#26124,#26125,#26126,#26127,#26128,#26129,#26130,#26131,#26132,
#26133,#26134,#26135,#26136,#26137,#26138,#26139,#26140,#26141,#26142,#26143,
#26144,#26145,#26146,#26147,#26148,#26149,#26150,#26151,#26152,#26153,#26154,
#26155,#26156,#26157,#26158,#26159,#26160,#26161,#26162,#26163,#26164,#26165,
#26166,#26167,#26168,#26169,#26170,#26171,#26172,#26173,#26174,#26175,#26176,
#26177,#26178,#26179,#26180,#26181,#26182,#26183,#26184,#26185,#26186,#26187,
#26188,#26189,#26190,#26191,#26192,#26193,#26194,#26195,#26196,#26197,#26198,
#26199,#26200,#26201,#26202,#26203,#26204,#26205,#26206,#26207,#26208,#26209,
#26210,#26211,#26212,#26213,#26214,#26215,#26216,#26217,#26218,#26219,#26220,
#26221,#26222,#26223,#26224,#26225,#26226,#26227,#26228,#26229,#26230,#26231,
#26232,#26233,#26234,#26235,#26236,#26237,#26238,#26239,#26240,#26241,#26242,
#26243,#26244,#26245,#26246,#26247,#26248,#26249,#26250,#26251,#26252,#26253,
#26254,#26255,#26256,#26257,#26258,#26259,#26260,#26261,#26262,#26263,#26264,
#26265,#26266,#26267,#26268,#26269,#26270,#26271,#26272,#26273,#26274,#26275,
#26276,#26277,#26278,#26279,#26280,#26281,#26282,#26283,#26284,#26285,#26286,
#26287,#26288,#26289,#26290,#26291,#26292,#26293,#26294,#26295,#26296,#26297,
#26298,#26299,#26300,#26301,#26302,#26303,#26304,#26305,#26306,#26307,#26308,
#26309,#26310,#26311,#26312,#26313,#26314,#26315,#26316,#26317,#26318,#26319,
#26320,#26321,#26322,#26323,#26324,#26325,#26326,#26327,#26328,#26329,#26330,
#26331,#26332,#26333,#26334,#26335,#26336,#26337,#26338,#26339,#26340,#26341,
#26342,#26343,#26344,#26345,#26346,#26347,#26348,#26349,#26350,#26351,#26352,
#26353,#26354,#26355,#26356,#26357,#26358,#26359,#26360,#26361,#26362,#26363,
#26364,#26365,#26366,#26367,#26368,#26369,#26370,#26371,#26372,#26373,#26374,
#26375,#26376,#26377,#26378,#26379,#26380,#26381,#26382,#26383,#26384,#26385,
#26386,#26387,#26388,#26389,#26390,#26391,#26392,#26393,#26394,#26395,#26396,
#26397,#26398,#26399,#26400,#26401,#26402,#26403,#26404,#26405,#26406,#26407,
#26408,#26409,#26410,#26411,#26412,#26413,#26414,#26415,#26416,#26417,#26418,
#26419,#26420,#26421,#26422,#26423,#26424,#26425,#26426,#26427,#26428,#26429,
#26430,#26431,#26432,#26433,#26434,#26435,#26436,#26437,#26438,#26439,#26440,
#26441,#26442,#26443,#26444,#26445,#26446,#26447,#26448,#26449,#26450,#26451,
#26452,#26453,#26454,#26455,#26456,#26457,#26458,#26459,#26460,#26461,#26462,
#26463,#26464,#26465,#26466,#26467,#26468,#26469,#26470,#26471,#26472,#26473,
#26474,#26475,#26476,#26477,#26478,#26479,#26480,#26481,#26482,#26483,#26484,
#26485,#26486,#26487,#26488,#26489,#26490,#26491,#26492,#26493,#26494,#26495,
#26496,#26497,#26498,#26499,#26500,#26501,#26502,#26503,#26504,#26505,#26506,
#26507,#26508,#26509,#26510,#26511,#26512,#26513,#26514,#26515,#26516,#26517,
#26518,#26519,#26520,#26521,#26522,#26523,#26524,#26525,#26526,#26527,#26528,
#26529,#26530,#26531,#26532,#26533,#26534,#26535,#26536,#26537,#26538,#26539,
#26540,#26541,#26542,#26543,#26544,#26545,#26546,#26547,#26548,#26549,#26550,
#26551,#26552,#26553,#26554,#26555,#26556,#26557,#26558,#26559,#26560,#26561,
#26562,#26563,#26564,#26565,#26566,#26567,#26568,#26569,#26570,#26571,#26572,
#26573,#26574,#26575,#26576,#26577,#26578,#26579,#26580,#26581,#26582,#26583,
#26584,#26585,#26586,#26587,#26588,#26589,#26590,#26591,#26592,#26593,#26594,
#26595,#26596,#26597,#26598,#26599,#26600,#26601,#26602,#26603,#26604,#26605,
#26606,#26607,#26608,#26609,#26610,#26611,#26612),(#26613,#26614,#26615,
#26616,#26617,#26618,#26619,#26620,#26621,#26622,#26623,#26624,#26625,#26626,
#26627,#26628,#26629,#26630,#26631,#26632,#26633,#26634,#26635,#26636,#26637,
#26638,#26639,#26640,#26641,#26642,#26643,#26644,#26645,#26646,#26647,#26648,
#26649,#26650,#26651,#26652,#26653,#26654,#26655,#26656,#26657,#26658,#26659,
#26660,#26661,#26662,#26663,#26664,#26665,#26666,#26667,#26668,#26669,#26670,
#26671,#26672,#26673,#26674,#26675,#26676,#26677,#26678,#26679,#26680,#26681,
#26682,#26683,#26684,#26685,#26686,#26687,#26688,#26689,#26690,#26691,#26692,
#26693,#26694,#26695,#26696,#26697,#26698,#26699,#26700,#26701,#26702,#26703,
#26704,#26705,#26706,#26707,#26708,#26709,#26710,#26711,#26712,#26713,#26714,
#26715,#26716,#26717,#26718,#26719,#26720,#26721,#26722,#26723,#26724,#26725,
#26726,#26727,#26728,#26729,#26730,#26731,#26732,#26733,#26734,#26735,#26736,
#26737,#26738,#26739,#26740,#26741,#26742,#26743,#26744,#26745,#26746,#26747,
#26748,#26749,#26750,#26751,#26752,#26753,#26754,#26755,#26756,#26757,#26758,
#26759,#26760,#26761,#26762,#26763,#26764,#26765,#26766,#26767,#26768,#26769,
#26770,#26771,#26772,#26773,#26774,#26775,#26776,#26777,#26778,#26779,#26780,
#26781,#26782,#26783,#26784,#26785,#26786,#26787,#26788,#26789,#26790,#26791,
#26792,#26793,#26794,#26795,#26796,#26797,#26798,#26799,#26800,#26801,#26802,
#26803,#26804,#26805,#26806,#26807,#26808,#26809,#26810,#26811,#26812,#26813,
#26814,#26815,#26816,#26817,#26818,#26819,#26820,#26821,#26822,#26823,#26824,
#26825,#26826,#26827,#26828,#26829,#26830,#26831,#26832,#26833,#26834,#26835,
#26836,#26837,#26838,#26839,#26840,#26841,#26842,#26843,#26844,#26845,#26846,
#26847,#26848,#26849,#26850,#26851,#26852,#26853,#26854,#26855,#26856,#26857,
#26858,#26859,#26860,#26861,#26862,#26863,#26864,#26865,#26866,#26867,#26868,
#26869,#26870,#26871,#26872,#26873,#26874,#26875,#26876,#26877,#26878,#26879,
#26880,#26881,#26882,#26883,#26884,#26885,#26886,#26887,#26888,#26889,#26890,
#26891,#26892,#26893,#26894,#26895,#26896,#26897,#26898,#26899,#26900,#26901,
#26902,#26903,#26904,#26905,#26906,#26907,#26908,#26909,#26910,#26911,#26912,
#26913,#26914,#26915,#26916,#26917,#26918,#26919,#26920,#26921,#26922,#26923,
#26924,#26925,#26926,#26927,#26928,#26929,#26930,#26931,#26932,#26933,#26934,
#26935,#26936,#26937,#26938,#26939,#26940,#26941,#26942,#26943,#26944,#26945,
#26946,#26947,#26948,#26949,#26950,#26951,#26952,#26953,#26954,#26955,#26956,
#26957,#26958,#26959,#26960,#26961,#26962,#26963,#26964,#26965,#26966,#26967,
#26968,#26969,#26970,#26971,#26972,#26973,#26974,#26975,#26976,#26977,#26978,
#26979,#26980,#26981,#26982,#26983,#26984,#26985,#26986,#26987,#26988,#26989,
#26990,#26991,#26992,#26993,#26994,#26995,#26996,#26997,#26998,#26999,#27000,
#27001,#27002,#27003,#27004,#27005,#27006,#27007,#27008,#27009,#27010,#27011,
#27012,#27013,#27014,#27015,#27016,#27017,#27018,#27019,#27020,#27021,#27022,
#27023,#27024,#27025,#27026,#27027,#27028,#27029,#27030,#27031,#27032,#27033,
#27034,#27035,#27036,#27037,#27038,#27039,#27040,#27041,#27042,#27043,#27044,
#27045,#27046,#27047,#27048,#27049,#27050,#27051,#27052,#27053,#27054,#27055,
#27056,#27057,#27058,#27059,#27060,#27061,#27062,#27063,#27064,#27065,#27066,
#27067,#27068,#27069,#27070,#27071,#27072,#27073,#27074,#27075,#27076,#27077,
#27078,#27079,#27080,#27081,#27082,#27083,#27084,#27085,#27086,#27087,#27088,
#27089,#27090,#27091,#27092,#27093,#27094,#27095,#27096,#27097,#27098,#27099,
#27100,#27101,#27102,#27103,#27104,#27105,#27106,#27107,#27108,#27109,#27110,
#27111,#27112,#27113,#27114,#27115,#27116,#27117,#27118,#27119,#27120,#27121,
#27122,#27123,#27124,#27125,#27126,#27127,#27128,#27129,#27130,#27131,#27132,
#27133,#27134,#27135,#27136,#27137,#27138,#27139,#27140,#27141,#27142,#27143,
#27144,#27145,#27146,#27147,#27148,#27149,#27150,#27151,#27152,#27153,#27154,
#27155,#27156,#27157,#27158,#27159,#27160,#27161,#27162,#27163,#27164,#27165,
#27166,#27167,#27168,#27169,#27170,#27171,#27172,#27173,#27174,#27175,#27176,
#27177,#27178,#27179,#27180,#27181,#27182,#27183,#27184,#27185,#27186,#27187,
#27188,#27189,#27190,#27191,#27192,#27193,#27194,#27195,#27196,#27197,#27198,
#27199,#27200,#27201,#27202,#27203,#27204,#27205,#27206,#27207,#27208,#27209,
#27210,#27211,#27212,#27213,#27214,#27215,#27216,#27217,#27218,#27219,#27220,
#27221,#27222,#27223,#27224,#27225,#27226,#27227,#27228,#27229,#27230,#27231,
#27232,#27233,#27234,#27235,#27236,#27237,#27238,#27239,#27240,#27241,#27242,
#27243,#27244,#27245,#27246,#27247,#27248,#27249,#27250,#27251,#27252,#27253,
#27254,#27255,#27256,#27257,#27258,#27259,#27260,#27261,#27262,#27263,#27264,
#27265,#27266,#27267,#27268,#27269,#27270,#27271,#27272,#27273,#27274,#27275,
#27276,#27277,#27278,#27279,#27280,#27281,#27282,#27283,#27284,#27285,#27286,
#27287,#27288,#27289,#27290,#27291,#27292,#27293,#27294),(#27295,#27296,
#27297,#27298,#27299,#27300,#27301,#27302,#27303,#27304,#27305,#27306,#27307,
#27308,#27309,#27310,#27311,#27312,#27313,#27314,#27315,#27316,#27317,#27318,
#27319,#27320,#27321,#27322,#27323,#27324,#27325,#27326,#27327,#27328,#27329,
#27330,#27331,#27332,#27333,#27334,#27335,#27336,#27337,#27338,#27339,#27340,
#27341,#27342,#27343,#27344,#27345,#27346,#27347,#27348,#27349,#27350,#27351,
#27352,#27353,#27354,#27355,#27356,#27357,#27358,#27359,#27360,#27361,#27362,
#27363,#27364,#27365,#27366,#27367,#27368,#27369,#27370,#27371,#27372,#27373,
#27374,#27375,#27376,#27377,#27378,#27379,#27380,#27381,#27382,#27383,#27384,
#27385,#27386,#27387,#27388,#27389,#27390,#27391,#27392,#27393,#27394,#27395,
#27396,#27397,#27398,#27399,#27400,#27401,#27402,#27403,#27404,#27405,#27406,
#27407,#27408,#27409,#27410,#27411,#27412,#27413,#27414,#27415,#27416,#27417,
#27418,#27419,#27420,#27421,#27422,#27423,#27424,#27425,#27426,#27427,#27428,
#27429,#27430,#27431,#27432,#27433,#27434,#27435,#27436,#27437,#27438,#27439,
#27440,#27441,#27442,#27443,#27444,#27445,#27446,#27447,#27448,#27449,#27450,
#27451,#27452,#27453,#27454,#27455,#27456,#27457,#27458,#27459,#27460,#27461,
#27462,#27463,#27464,#27465,#27466,#27467,#27468,#27469,#27470,#27471,#27472,
#27473,#27474,#27475,#27476,#27477,#27478,#27479,#27480,#27481,#27482,#27483,
#27484,#27485,#27486,#27487,#27488,#27489,#27490,#27491,#27492,#27493,#27494,
#27495,#27496,#27497,#27498,#27499,#27500,#27501,#27502,#27503,#27504,#27505,
#27506,#27507,#27508,#27509,#27510,#27511,#27512,#27513,#27514,#27515,#27516,
#27517,#27518,#27519,#27520,#27521,#27522,#27523,#27524,#27525,#27526,#27527,
#27528,#27529,#27530,#27531,#27532,#27533,#27534,#27535,#27536,#27537,#27538,
#27539,#27540,#27541,#27542,#27543,#27544,#27545,#27546,#27547,#27548,#27549,
#27550,#27551,#27552,#27553,#27554,#27555,#27556,#27557,#27558,#27559,#27560,
#27561,#27562,#27563,#27564,#27565,#27566,#27567,#27568,#27569,#27570,#27571,
#27572,#27573,#27574,#27575,#27576,#27577,#27578,#27579,#27580,#27581,#27582,
#27583,#27584,#27585,#27586,#27587,#27588,#27589,#27590,#27591,#27592,#27593,
#27594,#27595,#27596,#27597,#27598,#27599,#27600,#27601,#27602,#27603,#27604,
#27605,#27606,#27607,#27608,#27609,#27610,#27611,#27612,#27613,#27614,#27615,
#27616,#27617,#27618,#27619,#27620,#27621,#27622,#27623,#27624,#27625,#27626,
#27627,#27628,#27629,#27630,#27631,#27632,#27633,#27634,#27635,#27636,#27637,
#27638,#27639,#27640,#27641,#27642,#27643,#27644,#27645,#27646,#27647,#27648,
#27649,#27650,#27651,#27652,#27653,#27654,#27655,#27656,#27657,#27658,#27659,
#27660,#27661,#27662,#27663,#27664,#27665,#27666,#27667,#27668,#27669,#27670,
#27671,#27672,#27673,#27674,#27675,#27676,#27677,#27678,#27679,#27680,#27681,
#27682,#27683,#27684,#27685,#27686,#27687,#27688,#27689,#27690,#27691,#27692,
#27693,#27694,#27695,#27696,#27697,#27698,#27699,#27700,#27701,#27702,#27703,
#27704,#27705,#27706,#27707,#27708,#27709,#27710,#27711,#27712,#27713,#27714,
#27715,#27716,#27717,#27718,#27719,#27720,#27721,#27722,#27723,#27724,#27725,
#27726,#27727,#27728,#27729,#27730,#27731,#27732,#27733,#27734,#27735,#27736,
#27737,#27738,#27739,#27740,#27741,#27742,#27743,#27744,#27745,#27746,#27747,
#27748,#27749,#27750,#27751,#27752,#27753,#27754,#27755,#27756,#27757,#27758,
#27759,#27760,#27761,#27762,#27763,#27764,#27765,#27766,#27767,#27768,#27769,
#27770,#27771,#27772,#27773,#27774,#27775,#27776,#27777,#27778,#27779,#27780,
#27781,#27782,#27783,#27784,#27785,#27786,#27787,#27788,#27789,#27790,#27791,
#27792,#27793,#27794,#27795,#27796,#27797,#27798,#27799,#27800,#27801,#27802,
#27803,#27804,#27805,#27806,#27807,#27808,#27809,#27810,#27811,#27812,#27813,
#27814,#27815,#27816,#27817,#27818,#27819,#27820,#27821,#27822,#27823,#27824,
#27825,#27826,#27827,#27828,#27829,#27830,#27831,#27832,#27833,#27834,#27835,
#27836,#27837,#27838,#27839,#27840,#27841,#27842,#27843,#27844,#27845,#27846,
#27847,#27848,#27849,#27850,#27851,#27852,#27853,#27854,#27855,#27856,#27857,
#27858,#27859,#27860,#27861,#27862,#27863,#27864,#27865,#27866,#27867,#27868,
#27869,#27870,#27871,#27872,#27873,#27874,#27875,#27876,#27877,#27878,#27879,
#27880,#27881,#27882,#27883,#27884,#27885,#27886,#27887,#27888,#27889,#27890,
#27891,#27892,#27893,#27894,#27895,#27896,#27897,#27898,#27899,#27900,#27901,
#27902,#27903,#27904,#27905,#27906,#27907,#27908,#27909,#27910,#27911,#27912,
#27913,#27914,#27915,#27916,#27917,#27918,#27919,#27920,#27921,#27922,#27923,
#27924,#27925,#27926,#27927,#27928,#27929,#27930,#27931,#27932,#27933,#27934,
#27935,#27936,#27937,#27938,#27939,#27940,#27941,#27942,#27943,#27944,#27945,
#27946,#27947,#27948,#27949,#27950,#27951,#27952,#27953,#27954,#27955,#27956,
#27957,#27958,#27959,#27960,#27961,#27962,#27963,#27964,#27965,#27966,#27967,
#27968,#27969,#27970,#27971,#27972,#27973,#27974,#27975,#27976)),
 .UNSPECIFIED.,.F.,.F.,.F.,(4,4),(4,1,1,1,1,1,1,1,1,1,1,1,1,1,1,1,1,1,1,
1,1,1,1,1,1,1,1,1,1,1,1,1,1,1,1,1,1,1,1,1,1,1,1,1,1,1,1,1,1,1,1,1,1,1,1,
1,1,1,1,1,1,1,1,1,1,1,1,1,1,1,1,1,1,1,1,1,1,1,1,1,1,1,1,1,1,1,1,1,1,1,1,
1,1,1,1,1,1,1,1,1,1,1,1,1,1,1,1,1,1,1,1,1,1,1,1,1,1,1,1,1,1,1,1,1,1,1,1,
1,1,1,1,1,1,1,1,1,1,1,1,1,1,1,1,1,1,1,1,1,1,1,1,1,1,1,1,1,1,1,1,1,1,1,1,
1,1,1,1,1,1,1,1,1,1,1,1,1,1,1,1,1,1,1,1,1,1,1,1,1,1,1,1,1,1,1,1,1,1,1,1,
1,1,1,1,1,1,1,1,1,1,1,1,1,1,1,1,1,1,1,1,1,1,1,1,1,1,1,1,1,1,1,1,1,1,1,1,
1,1,1,1,1,1,1,1,1,1,1,1,1,1,1,1,1,1,1,1,1,1,1,1,1,1,1,1,1,1,1,1,1,1,1,1,
1,1,1,1,1,1,1,1,1,1,1,1,1,1,1,1,1,1,1,1,1,1,1,1,1,1,1,1,1,1,1,1,1,1,1,1,
1,1,1,1,1,1,1,1,1,1,1,1,1,1,1,1,1,1,1,1,1,1,1,1,1,1,1,1,1,1,1,1,1,1,1,1,
1,1,1,1,1,1,1,1,1,1,1,1,1,1,1,1,1,1,1,1,1,1,1,1,1,1,1,1,1,1,1,1,1,1,1,1,
1,1,1,1,1,1,1,1,1,1,1,1,1,1,1,1,1,1,1,1,1,1,1,1,1,1,1,1,1,1,1,1,1,1,1,1,
1,1,1,1,1,1,1,1,1,1,1,1,1,1,1,1,1,1,1,1,1,1,1,1,1,1,1,1,1,1,1,1,1,1,1,1,
1,1,1,1,1,1,1,1,1,1,1,1,1,1,1,1,1,1,1,1,1,1,1,1,1,1,1,1,1,1,1,1,1,1,1,1,
1,1,1,1,1,1,1,1,1,1,1,1,1,1,1,1,1,1,1,1,1,1,1,1,1,1,1,1,1,1,1,1,1,1,1,1,
1,1,1,1,1,1,1,1,1,1,1,1,1,1,1,1,1,1,1,1,1,1,1,1,1,1,1,1,1,1,1,1,1,1,1,1,
1,1,1,1,1,1,1,1,1,1,1,1,1,1,1,1,1,1,1,1,1,1,1,1,1,1,1,1,1,1,1,1,1,1,1,1,
1,1,1,1,1,1,1,1,1,1,1,1,1,1,1,1,1,1,1,1,1,1,1,1,1,1,1,1,1,1,1,1,1,1,1,1,
1,1,1,1,1,1,1,1,1,1,1,1,1,1,1,1,1,1,1,1,1,1,1,1,1,1,1,1,1,1,1,1,1,1,1,1,
1,1,1,1,1,1,1,1,1,1,1,1,4),(0.,0.198319817466637),(11.6150328478198,12.1147767088206,
12.6145205698214,13.614008291823,14.6134960138245,15.6129837358261,16.1127275968269,
16.6124714578277,17.6119591798292,18.6114469018308,19.6109346238324,20.6104223458339,
21.6099100678355,22.1096539288363,22.6093977898371,23.6088855118386,24.6083732338402,
25.6078609558418,26.6073486778433,27.6068363998449,28.6063241218465,29.1060679828472,
29.605811843848,30.6052995658496,31.6047872878512,32.6042750098527,33.6037627318543,
34.6032504538559,35.6027381758574,36.1024820368582,36.602225897859,37.6017136198606,
38.6012013418621,39.6006890638637,40.6001767858653,41.5996645078668,42.5991522298684,
43.0988960908692,43.59863995187,44.5981276738715,45.5976153958731,46.5971031178747,
47.5965908398762,48.5960785618778,49.5955662838794,50.0953101448802,50.5950540058809,
51.5945417278825,52.5940294498841,53.5935171718856,54.5930048938872,55.5924926158888,
56.5919803378903,57.0917241988911,57.5914680598919,58.5909557818935,59.590443503895,
60.5899312258966,61.5894189478982,62.5889066698997,63.5883943919013,64.0881382529021,
64.5878821139029,65.5873698359044,66.586857557906,67.5863452799076,68.5858330019091,
69.5853207239107,70.5848084459123,71.0845523069131,71.5842961679138,72.5837838899154,
73.583271611917,74.5827593339185,75.5822470559201,76.5817347779217,77.5812224999232,
78.080966360924,78.5807102219248,79.5801979439264,80.5796856659279,81.5791733879295,
82.5786611099311,83.5781488319326,84.5776365539342,85.077380414935,85.5771242759358,
86.5766119979373,87.5760997199389,88.5755874419405,89.575075163942,90.5745628859436,
91.5740506079452,92.073794468946,92.5735383299467,93.5730260519483,94.5725137739499,
95.5720014959514,96.571489217953,97.5709769399546,98.5704646619562,99.0702085229569,
99.5699523839577,100.569440105959,101.568927827961,102.568415549962,103.567903271964,
104.567390993966,105.566878715967,106.066622576968,106.566366437969,107.56585415997,
108.565341881972,109.564829603973,110.564317325975,111.563805047977,112.563292769978,
113.063036630979,113.56278049198,114.562268213981,115.561755935983,116.561243657984,
117.560731379986,118.560219101987,119.559706823989,120.05945068499,120.559194545991,
121.558682267992,122.558169989994,123.557657711995,124.557145433997,125.556633155998,
126.556120878,127.055864739001,127.555608600002,128.555096322003,129.554584044005,
130.554071766006,131.553559488008,132.553047210009,133.552534932011,134.052278793012,
134.552022654013,135.551510376014,136.550998098016,137.550485820017,138.549973542019,
139.54946126402,140.548948986022,141.048692847023,141.548436708024,142.547924430025,
143.547412152027,144.546899874028,145.54638759603,146.545875318031,147.545363040033,
148.045106901034,148.544850762035,149.544338484036,150.543826206038,151.543313928039,
152.542801650041,153.542289372042,154.541777094044,155.041520955045,155.541264816045,
156.540752538047,157.540240260049,158.53972798205,159.539215704052,160.538703426053,
161.538191148055,162.037935009056,162.537678870056,163.537166592058,164.53665431406,
165.536142036061,166.535629758063,167.535117480064,168.534605202066,169.034349063067,
169.534092924067,170.533580646069,171.533068368071,172.532556090072,173.532043812074,
174.531531534075,175.531019256077,176.030763117078,176.530506978078,177.52999470008,
178.529482422082,179.528970144083,180.528457866085,181.527945588086,182.527433310088,
183.027177171089,183.526921032089,184.526408754091,185.525896476092,186.525384198094,
187.524871920096,188.524359642097,189.523847364099,190.0235912251,190.5233350861,
191.522822808102,192.522310530103,193.521798252105,194.521285974107,195.520773696108,
196.52026141811,197.020005279111,197.519749140111,198.519236862113,199.518724584114,
200.518212306116,201.517700028118,202.517187750119,203.516675472121,204.016419333121,
204.516163194122,205.515650916124,206.515138638125,207.514626360127,208.514114082129,
209.51360180413,210.513089526132,211.012833387132,211.512577248133,212.512064970135,
213.511552692136,214.511040414138,215.510528136139,216.510015858141,217.509503580143,
218.009247441143,218.508991302144,219.508479024146,220.507966746147,221.507454468149,
222.50694219015,223.506429912152,224.505917634154,225.005661495154,225.505405356155,
226.504893078157,227.504380800158,228.50386852216,229.503356244161,230.502843966163,
231.502331688165,232.002075549165,232.501819410166,233.501307132168,234.500794854169,
235.500282576171,236.499770298172,237.499258020174,238.498745742176,238.998489603176,
239.498233464177,240.497721186179,241.49720890818,242.496696630182,243.496184352183,
244.495672074185,245.495159796186,245.994903657187,246.494647518188,247.49413524019,
248.493622962191,249.493110684193,250.492598406194,251.492086128196,252.491573850197,
252.991317711198,253.491061572199,254.490549294201,255.490037016202,256.489524738204,
257.489012460205,258.488500182207,259.487987904208,259.987731765209,260.48747562621,
261.486963348212,262.486451070213,263.485938792215,264.485426514216,265.484914236218,
266.484401958219,266.98414581922,267.483889680221,268.483377402223,269.482865124224,
270.482352846226,271.481840568227,272.481328290229,273.48081601223,273.980559873231,
274.480303734232,275.479791456233,276.479279178235,277.478766900237,278.478254622238,
279.47774234424,280.477230066241,280.976973927242,281.476717788243,282.476205510244,
283.475693232246,284.475180954248,285.474668676249,286.474156398251,287.473644120252,
287.973387981253,288.473131842254,289.472619564255,290.472107286257,291.471595008259,
292.47108273026,293.470570452262,294.470058174263,294.969802035264,295.469545896265,
296.469033618266,297.468521340268,298.46800906227,299.467496784271,300.466984506273,
301.466472228274,301.966216089275,302.465959950276,303.465447672277,304.464935394279,
305.46442311628,306.463910838282,307.463398560284,308.462886282285,309.462374004287,
310.461861726288,311.46134944829,312.460837170291,313.460324892293,313.960068753294,
314.459812614295,315.459300336296,316.458788058298,317.458275780299,318.457763502301,
319.457251224302,320.456738946304,320.956482807305,321.456226668306,322.455714390307,
323.455202112309,324.45468983431,325.454177556312,326.453665278313,327.453153000315,
327.952896861316,328.452640722317,329.452128444318,330.45161616632,331.451103888321,
332.450591610323,333.450079332324,334.449567054326,334.949310915327,335.449054776328,
336.448542498329,337.448030220331,338.447517942332,339.447005664334,340.446493386335,
341.445981108337,341.945724969338,342.445468830338,343.44495655234,344.444444274342,
345.443931996343,346.443419718345,347.442907440346,348.442395162348,348.942139023349,
349.441882884349,350.441370606351,351.440858328353,352.440346050354,353.439833772356,
354.439321494357,355.438809216359,355.93855307736,356.43829693836,357.437784660362,
358.437272382364,359.436760104365,360.436247826367,361.435735548368,362.43522327037,
362.934967131371,363.434710992371,364.434198714373,365.433686436375,366.433174158376,
367.432661880378,368.432149602379,369.431637324381,369.931381185382,370.431125046382,
371.430612768384,372.430100490385,373.429588212387,374.429075934389,375.42856365639,
376.428051378392,376.927795239393,377.427539100393,378.427026822395,379.426514544396,
380.426002266398,381.4254899884,382.424977710401,383.424465432403,383.924209293403,
384.423953154404,385.423440876406,386.422928598407,387.422416320409,388.421904042411,
389.421391764412,390.420879486414,390.920623347414,391.420367208415,392.419854930417,
393.419342652418,394.41883037442,395.418318096422,396.417805818423,397.417293540425,
397.917037401425,398.416781262426,399.416268984428,400.415756706429,401.415244428431,
402.414732150432,403.414219872434,404.413707594436,404.913451455436,405.413195316437,
406.412683038439,407.41217076044,408.411658482442,409.411146204443,410.410633926445,
411.410121648447,411.909865509447,412.409609370448,413.40909709245,414.408584814451,
415.408072536453,416.407560258454,417.407047980456,418.406535702458,418.906279563458,
419.406023424459,420.405511146461,421.404998868462,422.404486590464,423.403974312465,
424.403462034467,425.402949756469,425.902693617469,426.40243747847,427.401925200472,
428.401412922473,429.400900644475,430.400388366476,431.399876088478,432.399363810479,
432.89910767148,433.398851532481,434.398339254483,435.397826976484,436.397314698486,
437.396802420487,438.396290142489,439.39577786449,439.895521725491,440.395265586492,
441.394753308494,442.394241030495,443.393728752497,444.393216474498,445.3927041965,
446.392191918501,446.891935779502,447.391679640503,448.391167362505,449.390655084506,
450.390142806508,451.389630528509,452.389118250511,453.388605972512,453.888349833513,
454.388093694514,455.387581416516,456.387069138517,457.386556860519,458.38604458252,
459.385532304522,460.385020026523,460.884763887524,461.384507748525,462.383995470527,
463.383483192528,464.38297091453,465.382458636531,466.381946358533,467.381434080534,
467.881177941535,468.380921802536,469.380409524537,470.379897246539,471.379384968541,
472.378872690542,473.378360412544,474.377848134545,474.877591995546,475.377335856547,
476.376823578548,477.37631130055,478.375799022552,479.375286744553,480.374774466555,
481.374262188556,481.874006049557,482.373749910558,483.373237632559,484.372725354561,
485.372213076563,486.371700798564,487.371188520566,488.370676242567,488.870420103568,
489.370163964569,490.36965168657,491.369139408572,492.368627130574,493.368114852575,
494.367602574577,495.367090296578,495.866834157579,496.36657801858,497.366065740581,
498.365553462583,499.365041184584,500.364528906586,501.364016628588,502.363504350589,
502.86324821159,503.362992072591,504.362479794592,505.361967516594,506.361455238595,
507.360942960597,508.360430682599,509.3599184046,509.859662265601,510.359406126602,
511.358893848603,512.358381570605,513.357869292606,514.357357014608,515.35684473661,
516.356332458611,516.856076319612,517.355820180613,518.355307902614,519.354795624616,
520.354283346617,521.353771068619,522.353258790621,523.352746512622,523.852490373623,
524.352234234624,525.351721956625,526.351209678627,527.350697400628,528.35018512263,
529.349672844632,530.349160566633,530.848904427634,531.348648288635,532.348136010636,
533.347623732638,534.347111454639,535.346599176641,536.346086898643,537.345574620644,
537.845318481645,538.345062342646,539.344550064647,540.344037786649,541.34352550865,
542.343013230652,543.342500952653,544.341988674655,544.841732535656,545.341476396657,
546.340964118658,547.34045184066,548.339939562661,549.339427284663,550.338915006664,
551.338402728666,551.838146589667,552.337890450668,553.337378172669,554.336865894671,
555.336353616672,556.335841338674,557.335329060675,558.334816782677,558.834560643678,
559.334304504679,560.33379222668,561.333279948682,562.332767670683,563.332255392685,
564.331743114686,565.331230836688,565.830974697689,566.33071855869,567.330206280691,
568.329694002693,569.329181724694,570.328669446696,571.328157168697,572.327644890699,
572.8273887517,573.327132612701,574.326620334702,575.326108056704,576.325595778705,
577.325083500707,578.324571222708,579.32405894471,579.823802805711,580.323546666712,
581.323034388713,582.322522110715,583.322009832716,584.321497554718,585.320985276719,
586.320472998721,586.820216859722,587.319960720722,588.319448442724,589.318936164726,
590.318423886727,591.317911608729,592.31739933073,593.316887052732,593.816630913733,
594.316374774733,595.315862496735,596.315350218737,597.314837940738,598.31432566274,
599.313813384741,599.813557245742,600.313301106743,601.312788828744,602.312276550746,
603.311764272747,603.811508133748,604.311251994749),.UNSPECIFIED.);
#209=B_SPLINE_SURFACE_WITH_KNOTS('',3,3,((#29392,#29393,#29394,#29395,#29396,
#29397,#29398,#29399,#29400,#29401,#29402,#29403,#29404,#29405,#29406,#29407,
#29408,#29409,#29410,#29411,#29412,#29413,#29414,#29415,#29416,#29417,#29418,
#29419,#29420,#29421,#29422,#29423,#29424,#29425,#29426,#29427,#29428,#29429,
#29430,#29431,#29432,#29433,#29434,#29435,#29436,#29437,#29438,#29439,#29440,
#29441,#29442,#29443,#29444,#29445,#29446,#29447,#29448,#29449,#29450),
(#29451,#29452,#29453,#29454,#29455,#29456,#29457,#29458,#29459,#29460,
#29461,#29462,#29463,#29464,#29465,#29466,#29467,#29468,#29469,#29470,#29471,
#29472,#29473,#29474,#29475,#29476,#29477,#29478,#29479,#29480,#29481,#29482,
#29483,#29484,#29485,#29486,#29487,#29488,#29489,#29490,#29491,#29492,#29493,
#29494,#29495,#29496,#29497,#29498,#29499,#29500,#29501,#29502,#29503,#29504,
#29505,#29506,#29507,#29508,#29509),(#29510,#29511,#29512,#29513,#29514,
#29515,#29516,#29517,#29518,#29519,#29520,#29521,#29522,#29523,#29524,#29525,
#29526,#29527,#29528,#29529,#29530,#29531,#29532,#29533,#29534,#29535,#29536,
#29537,#29538,#29539,#29540,#29541,#29542,#29543,#29544,#29545,#29546,#29547,
#29548,#29549,#29550,#29551,#29552,#29553,#29554,#29555,#29556,#29557,#29558,
#29559,#29560,#29561,#29562,#29563,#29564,#29565,#29566,#29567,#29568),
(#29569,#29570,#29571,#29572,#29573,#29574,#29575,#29576,#29577,#29578,
#29579,#29580,#29581,#29582,#29583,#29584,#29585,#29586,#29587,#29588,#29589,
#29590,#29591,#29592,#29593,#29594,#29595,#29596,#29597,#29598,#29599,#29600,
#29601,#29602,#29603,#29604,#29605,#29606,#29607,#29608,#29609,#29610,#29611,
#29612,#29613,#29614,#29615,#29616,#29617,#29618,#29619,#29620,#29621,#29622,
#29623,#29624,#29625,#29626,#29627)),.UNSPECIFIED.,.F.,.F.,.F.,(4,4),(4,
1,1,1,1,1,1,1,1,1,1,1,1,1,1,1,1,1,1,1,1,1,1,1,1,1,1,1,1,1,1,1,1,1,1,1,1,
1,1,1,1,1,1,1,1,1,1,1,1,1,1,1,1,1,1,1,4),(0.,0.193239135097769),(11.8520359647449,
12.3369705490202,12.8219051332955,13.3068397175708,13.7917743018461,14.2767088861213,
14.7616434703966,15.2465780546719,15.7315126389472,16.2164472232225,16.7013818074977,
17.186316391773,17.6712509760483,18.1561855603236,18.6411201445989,19.1260547288741,
19.6109893131494,20.0959238974247,20.5808584817,21.0657930659752,21.5507276502505,
22.0356622345258,22.5205968188011,23.0055314030764,23.4904659873516,23.9754005716269,
24.4603351559022,24.9452697401775,25.4302043244528,25.915138908728,26.4000734930033,
26.8850080772786,27.3699426615539,27.8548772458292,28.3398118301044,28.8247464143797,
29.309680998655,29.7946155829303,30.2795501672055,30.7644847514808,31.2494193357561,
31.7343539200314,32.2192885043067,32.7042230885819,33.1891576728572,33.6740922571325,
34.1590268414078,34.6439614256831,35.1288960099583,35.6138305942336,36.0987651785089,
36.5836997627842,37.0686343470595,37.5535689313347,38.03850351561,38.5234380998853,
39.0083726841606),.UNSPECIFIED.);
#210=B_SPLINE_SURFACE_WITH_KNOTS('',3,3,((#29826,#29827,#29828,#29829,#29830,
#29831,#29832,#29833,#29834,#29835,#29836,#29837,#29838,#29839,#29840,#29841,
#29842,#29843,#29844,#29845,#29846,#29847,#29848,#29849,#29850,#29851,#29852,
#29853,#29854,#29855,#29856,#29857,#29858,#29859,#29860,#29861,#29862,#29863,
#29864,#29865,#29866,#29867,#29868,#29869,#29870,#29871,#29872,#29873,#29874,
#29875,#29876,#29877,#29878,#29879,#29880,#29881,#29882,#29883,#29884),
(#29885,#29886,#29887,#29888,#29889,#29890,#29891,#29892,#29893,#29894,
#29895,#29896,#29897,#29898,#29899,#29900,#29901,#29902,#29903,#29904,#29905,
#29906,#29907,#29908,#29909,#29910,#29911,#29912,#29913,#29914,#29915,#29916,
#29917,#29918,#29919,#29920,#29921,#29922,#29923,#29924,#29925,#29926,#29927,
#29928,#29929,#29930,#29931,#29932,#29933,#29934,#29935,#29936,#29937,#29938,
#29939,#29940,#29941,#29942,#29943),(#29944,#29945,#29946,#29947,#29948,
#29949,#29950,#29951,#29952,#29953,#29954,#29955,#29956,#29957,#29958,#29959,
#29960,#29961,#29962,#29963,#29964,#29965,#29966,#29967,#29968,#29969,#29970,
#29971,#29972,#29973,#29974,#29975,#29976,#29977,#29978,#29979,#29980,#29981,
#29982,#29983,#29984,#29985,#29986,#29987,#29988,#29989,#29990,#29991,#29992,
#29993,#29994,#29995,#29996,#29997,#29998,#29999,#30000,#30001,#30002),
(#30003,#30004,#30005,#30006,#30007,#30008,#30009,#30010,#30011,#30012,
#30013,#30014,#30015,#30016,#30017,#30018,#30019,#30020,#30021,#30022,#30023,
#30024,#30025,#30026,#30027,#30028,#30029,#30030,#30031,#30032,#30033,#30034,
#30035,#30036,#30037,#30038,#30039,#30040,#30041,#30042,#30043,#30044,#30045,
#30046,#30047,#30048,#30049,#30050,#30051,#30052,#30053,#30054,#30055,#30056,
#30057,#30058,#30059,#30060,#30061)),.UNSPECIFIED.,.F.,.F.,.F.,(4,4),(4,
1,1,1,1,1,1,1,1,1,1,1,1,1,1,1,1,1,1,1,1,1,1,1,1,1,1,1,1,1,1,1,1,1,1,1,1,
1,1,1,1,1,1,1,1,1,1,1,1,1,1,1,1,1,1,1,4),(0.,0.193239135097769),(14.3987024268659,
14.8836370111412,15.3685715954165,15.8535061796917,16.338440763967,16.8233753482423,
17.3083099325176,17.7932445167929,18.2781791010681,18.7631136853434,19.2480482696187,
19.732982853894,20.2179174381693,20.7028520224445,21.1877866067198,21.6727211909951,
22.1576557752704,22.6425903595457,23.1275249438209,23.6124595280962,24.0973941123715,
24.5823286966468,25.067263280922,25.5521978651973,26.0371324494726,26.5220670337479,
27.0070016180232,27.4919362022984,27.9768707865737,28.461805370849,28.9467399551243,
29.4316745393996,29.9166091236748,30.4015437079501,30.8864782922254,31.3714128765007,
31.856347460776,32.3412820450512,32.8262166293265,33.3111512136018,33.7960857978771,
34.2810203821523,34.7659549664276,35.2508895507029,35.7358241349782,36.2207587192535,
36.7056933035287,37.190627887804,37.6755624720793,38.1604970563546,38.6454316406299,
39.1303662249051,39.6153008091804,40.1002353934557,40.585169977731,41.0701045620063,
41.5550391462815),.UNSPECIFIED.);
#211=B_SPLINE_SURFACE_WITH_KNOTS('',3,3,((#30749,#30750,#30751,#30752,#30753,
#30754,#30755,#30756,#30757,#30758,#30759,#30760,#30761,#30762,#30763,#30764,
#30765,#30766,#30767,#30768,#30769,#30770,#30771,#30772,#30773,#30774,#30775,
#30776,#30777,#30778,#30779,#30780,#30781,#30782,#30783,#30784,#30785,#30786,
#30787,#30788,#30789,#30790,#30791,#30792,#30793,#30794,#30795,#30796,#30797,
#30798,#30799,#30800,#30801,#30802,#30803,#30804,#30805,#30806,#30807),
(#30808,#30809,#30810,#30811,#30812,#30813,#30814,#30815,#30816,#30817,
#30818,#30819,#30820,#30821,#30822,#30823,#30824,#30825,#30826,#30827,#30828,
#30829,#30830,#30831,#30832,#30833,#30834,#30835,#30836,#30837,#30838,#30839,
#30840,#30841,#30842,#30843,#30844,#30845,#30846,#30847,#30848,#30849,#30850,
#30851,#30852,#30853,#30854,#30855,#30856,#30857,#30858,#30859,#30860,#30861,
#30862,#30863,#30864,#30865,#30866),(#30867,#30868,#30869,#30870,#30871,
#30872,#30873,#30874,#30875,#30876,#30877,#30878,#30879,#30880,#30881,#30882,
#30883,#30884,#30885,#30886,#30887,#30888,#30889,#30890,#30891,#30892,#30893,
#30894,#30895,#30896,#30897,#30898,#30899,#30900,#30901,#30902,#30903,#30904,
#30905,#30906,#30907,#30908,#30909,#30910,#30911,#30912,#30913,#30914,#30915,
#30916,#30917,#30918,#30919,#30920,#30921,#30922,#30923,#30924,#30925),
(#30926,#30927,#30928,#30929,#30930,#30931,#30932,#30933,#30934,#30935,
#30936,#30937,#30938,#30939,#30940,#30941,#30942,#30943,#30944,#30945,#30946,
#30947,#30948,#30949,#30950,#30951,#30952,#30953,#30954,#30955,#30956,#30957,
#30958,#30959,#30960,#30961,#30962,#30963,#30964,#30965,#30966,#30967,#30968,
#30969,#30970,#30971,#30972,#30973,#30974,#30975,#30976,#30977,#30978,#30979,
#30980,#30981,#30982,#30983,#30984)),.UNSPECIFIED.,.F.,.F.,.F.,(4,4),(4,
1,1,1,1,1,1,1,1,1,1,1,1,1,1,1,1,1,1,1,1,1,1,1,1,1,1,1,1,1,1,1,1,1,1,1,1,
1,1,1,1,1,1,1,1,1,1,1,1,1,1,1,1,1,1,1,4),(0.,0.193239135097767),(11.852035964745,
12.3369705490203,12.8219051332956,13.3068397175709,13.7917743018461,14.2767088861214,
14.7616434703967,15.246578054672,15.7315126389472,16.2164472232225,16.7013818074978,
17.1863163917731,17.6712509760483,18.1561855603236,18.6411201445989,19.1260547288742,
19.6109893131495,20.0959238974247,20.5808584817,21.0657930659753,21.5507276502506,
22.0356622345258,22.5205968188011,23.0055314030764,23.4904659873517,23.9754005716269,
24.4603351559022,24.9452697401775,25.4302043244528,25.9151389087281,26.4000734930033,
26.8850080772786,27.3699426615539,27.8548772458292,28.3398118301044,28.8247464143797,
29.309680998655,29.7946155829303,30.2795501672055,30.7644847514808,31.2494193357561,
31.7343539200314,32.2192885043067,32.7042230885819,33.1891576728572,33.6740922571325,
34.1590268414078,34.643961425683,35.1288960099583,35.6138305942336,36.0987651785089,
36.5836997627841,37.0686343470594,37.5535689313347,38.03850351561,38.5234380998853,
39.0083726841605),.UNSPECIFIED.);
#212=B_SPLINE_SURFACE_WITH_KNOTS('',3,3,((#31183,#31184,#31185,#31186,#31187,
#31188,#31189,#31190,#31191,#31192,#31193,#31194,#31195,#31196,#31197,#31198,
#31199,#31200,#31201,#31202,#31203,#31204,#31205,#31206,#31207,#31208,#31209,
#31210,#31211,#31212,#31213,#31214,#31215,#31216,#31217,#31218,#31219,#31220,
#31221,#31222,#31223,#31224,#31225,#31226,#31227,#31228,#31229,#31230,#31231,
#31232,#31233,#31234,#31235,#31236,#31237,#31238,#31239,#31240,#31241),
(#31242,#31243,#31244,#31245,#31246,#31247,#31248,#31249,#31250,#31251,
#31252,#31253,#31254,#31255,#31256,#31257,#31258,#31259,#31260,#31261,#31262,
#31263,#31264,#31265,#31266,#31267,#31268,#31269,#31270,#31271,#31272,#31273,
#31274,#31275,#31276,#31277,#31278,#31279,#31280,#31281,#31282,#31283,#31284,
#31285,#31286,#31287,#31288,#31289,#31290,#31291,#31292,#31293,#31294,#31295,
#31296,#31297,#31298,#31299,#31300),(#31301,#31302,#31303,#31304,#31305,
#31306,#31307,#31308,#31309,#31310,#31311,#31312,#31313,#31314,#31315,#31316,
#31317,#31318,#31319,#31320,#31321,#31322,#31323,#31324,#31325,#31326,#31327,
#31328,#31329,#31330,#31331,#31332,#31333,#31334,#31335,#31336,#31337,#31338,
#31339,#31340,#31341,#31342,#31343,#31344,#31345,#31346,#31347,#31348,#31349,
#31350,#31351,#31352,#31353,#31354,#31355,#31356,#31357,#31358,#31359),
(#31360,#31361,#31362,#31363,#31364,#31365,#31366,#31367,#31368,#31369,
#31370,#31371,#31372,#31373,#31374,#31375,#31376,#31377,#31378,#31379,#31380,
#31381,#31382,#31383,#31384,#31385,#31386,#31387,#31388,#31389,#31390,#31391,
#31392,#31393,#31394,#31395,#31396,#31397,#31398,#31399,#31400,#31401,#31402,
#31403,#31404,#31405,#31406,#31407,#31408,#31409,#31410,#31411,#31412,#31413,
#31414,#31415,#31416,#31417,#31418)),.UNSPECIFIED.,.F.,.F.,.F.,(4,4),(4,
1,1,1,1,1,1,1,1,1,1,1,1,1,1,1,1,1,1,1,1,1,1,1,1,1,1,1,1,1,1,1,1,1,1,1,1,
1,1,1,1,1,1,1,1,1,1,1,1,1,1,1,1,1,1,1,4),(0.,0.193239135097767),(14.398702426866,
14.8836370111412,15.3685715954165,15.8535061796918,16.3384407639671,16.8233753482423,
17.3083099325176,17.7932445167929,18.2781791010682,18.7631136853434,19.2480482696187,
19.732982853894,20.2179174381693,20.7028520224446,21.1877866067198,21.6727211909951,
22.1576557752704,22.6425903595457,23.1275249438209,23.6124595280962,24.0973941123715,
24.5823286966468,25.0672632809221,25.5521978651973,26.0371324494726,26.5220670337479,
27.0070016180232,27.4919362022984,27.9768707865737,28.461805370849,28.9467399551243,
29.4316745393996,29.9166091236748,30.4015437079501,30.8864782922254,31.3714128765007,
31.8563474607759,32.3412820450512,32.8262166293265,33.3111512136018,33.796085797877,
34.2810203821523,34.7659549664276,35.2508895507029,35.7358241349782,36.2207587192534,
36.7056933035287,37.190627887804,37.6755624720793,38.1604970563545,38.6454316406298,
39.1303662249051,39.6153008091804,40.1002353934557,40.5851699777309,41.0701045620062,
41.5550391462815),.UNSPECIFIED.);
#213=B_SPLINE_SURFACE_WITH_KNOTS('',3,3,((#32106,#32107,#32108,#32109,#32110,
#32111,#32112,#32113,#32114,#32115,#32116,#32117,#32118,#32119,#32120,#32121,
#32122,#32123,#32124,#32125,#32126,#32127,#32128,#32129,#32130,#32131,#32132,
#32133,#32134,#32135,#32136,#32137,#32138,#32139,#32140,#32141,#32142,#32143,
#32144,#32145,#32146,#32147,#32148,#32149,#32150,#32151,#32152,#32153,#32154,
#32155,#32156,#32157,#32158,#32159,#32160,#32161,#32162,#32163,#32164),
(#32165,#32166,#32167,#32168,#32169,#32170,#32171,#32172,#32173,#32174,
#32175,#32176,#32177,#32178,#32179,#32180,#32181,#32182,#32183,#32184,#32185,
#32186,#32187,#32188,#32189,#32190,#32191,#32192,#32193,#32194,#32195,#32196,
#32197,#32198,#32199,#32200,#32201,#32202,#32203,#32204,#32205,#32206,#32207,
#32208,#32209,#32210,#32211,#32212,#32213,#32214,#32215,#32216,#32217,#32218,
#32219,#32220,#32221,#32222,#32223),(#32224,#32225,#32226,#32227,#32228,
#32229,#32230,#32231,#32232,#32233,#32234,#32235,#32236,#32237,#32238,#32239,
#32240,#32241,#32242,#32243,#32244,#32245,#32246,#32247,#32248,#32249,#32250,
#32251,#32252,#32253,#32254,#32255,#32256,#32257,#32258,#32259,#32260,#32261,
#32262,#32263,#32264,#32265,#32266,#32267,#32268,#32269,#32270,#32271,#32272,
#32273,#32274,#32275,#32276,#32277,#32278,#32279,#32280,#32281,#32282),
(#32283,#32284,#32285,#32286,#32287,#32288,#32289,#32290,#32291,#32292,
#32293,#32294,#32295,#32296,#32297,#32298,#32299,#32300,#32301,#32302,#32303,
#32304,#32305,#32306,#32307,#32308,#32309,#32310,#32311,#32312,#32313,#32314,
#32315,#32316,#32317,#32318,#32319,#32320,#32321,#32322,#32323,#32324,#32325,
#32326,#32327,#32328,#32329,#32330,#32331,#32332,#32333,#32334,#32335,#32336,
#32337,#32338,#32339,#32340,#32341)),.UNSPECIFIED.,.F.,.F.,.F.,(4,4),(4,
1,1,1,1,1,1,1,1,1,1,1,1,1,1,1,1,1,1,1,1,1,1,1,1,1,1,1,1,1,1,1,1,1,1,1,1,
1,1,1,1,1,1,1,1,1,1,1,1,1,1,1,1,1,1,1,4),(0.,0.193239135097767),(11.8520359647451,
12.3369705490203,12.8219051332956,13.3068397175709,13.7917743018462,14.2767088861214,
14.7616434703967,15.246578054672,15.7315126389473,16.2164472232226,16.7013818074978,
17.1863163917731,17.6712509760484,18.1561855603237,18.6411201445989,19.1260547288742,
19.6109893131495,20.0959238974248,20.5808584817,21.0657930659753,21.5507276502506,
22.0356622345259,22.5205968188012,23.0055314030764,23.4904659873517,23.975400571627,
24.4603351559023,24.9452697401775,25.4302043244528,25.9151389087281,26.4000734930034,
26.8850080772787,27.3699426615539,27.8548772458292,28.3398118301045,28.8247464143798,
29.309680998655,29.7946155829303,30.2795501672056,30.7644847514809,31.2494193357561,
31.7343539200314,32.2192885043067,32.704223088582,33.1891576728573,33.6740922571325,
34.1590268414078,34.6439614256831,35.1288960099584,35.6138305942336,36.0987651785089,
36.5836997627842,37.0686343470595,37.5535689313348,38.03850351561,38.5234380998853,
39.0083726841606),.UNSPECIFIED.);
#214=B_SPLINE_SURFACE_WITH_KNOTS('',3,3,((#32540,#32541,#32542,#32543,#32544,
#32545,#32546,#32547,#32548,#32549,#32550,#32551,#32552,#32553,#32554,#32555,
#32556,#32557,#32558,#32559,#32560,#32561,#32562,#32563,#32564,#32565,#32566,
#32567,#32568,#32569,#32570,#32571,#32572,#32573,#32574,#32575,#32576,#32577,
#32578,#32579,#32580,#32581,#32582,#32583,#32584,#32585,#32586,#32587,#32588,
#32589,#32590,#32591,#32592,#32593,#32594,#32595,#32596,#32597,#32598),
(#32599,#32600,#32601,#32602,#32603,#32604,#32605,#32606,#32607,#32608,
#32609,#32610,#32611,#32612,#32613,#32614,#32615,#32616,#32617,#32618,#32619,
#32620,#32621,#32622,#32623,#32624,#32625,#32626,#32627,#32628,#32629,#32630,
#32631,#32632,#32633,#32634,#32635,#32636,#32637,#32638,#32639,#32640,#32641,
#32642,#32643,#32644,#32645,#32646,#32647,#32648,#32649,#32650,#32651,#32652,
#32653,#32654,#32655,#32656,#32657),(#32658,#32659,#32660,#32661,#32662,
#32663,#32664,#32665,#32666,#32667,#32668,#32669,#32670,#32671,#32672,#32673,
#32674,#32675,#32676,#32677,#32678,#32679,#32680,#32681,#32682,#32683,#32684,
#32685,#32686,#32687,#32688,#32689,#32690,#32691,#32692,#32693,#32694,#32695,
#32696,#32697,#32698,#32699,#32700,#32701,#32702,#32703,#32704,#32705,#32706,
#32707,#32708,#32709,#32710,#32711,#32712,#32713,#32714,#32715,#32716),
(#32717,#32718,#32719,#32720,#32721,#32722,#32723,#32724,#32725,#32726,
#32727,#32728,#32729,#32730,#32731,#32732,#32733,#32734,#32735,#32736,#32737,
#32738,#32739,#32740,#32741,#32742,#32743,#32744,#32745,#32746,#32747,#32748,
#32749,#32750,#32751,#32752,#32753,#32754,#32755,#32756,#32757,#32758,#32759,
#32760,#32761,#32762,#32763,#32764,#32765,#32766,#32767,#32768,#32769,#32770,
#32771,#32772,#32773,#32774,#32775)),.UNSPECIFIED.,.F.,.F.,.F.,(4,4),(4,
1,1,1,1,1,1,1,1,1,1,1,1,1,1,1,1,1,1,1,1,1,1,1,1,1,1,1,1,1,1,1,1,1,1,1,1,
1,1,1,1,1,1,1,1,1,1,1,1,1,1,1,1,1,1,1,4),(0.,0.193239135097767),(14.398702426866,
14.8836370111413,15.3685715954165,15.8535061796918,16.3384407639671,16.8233753482424,
17.3083099325176,17.7932445167929,18.2781791010682,18.7631136853435,19.2480482696188,
19.732982853894,20.2179174381693,20.7028520224446,21.1877866067199,21.6727211909951,
22.1576557752704,22.6425903595457,23.127524943821,23.6124595280962,24.0973941123715,
24.5823286966468,25.0672632809221,25.5521978651974,26.0371324494726,26.5220670337479,
27.0070016180232,27.4919362022985,27.9768707865737,28.461805370849,28.9467399551243,
29.4316745393996,29.9166091236749,30.4015437079501,30.8864782922254,31.3714128765007,
31.856347460776,32.3412820450512,32.8262166293265,33.3111512136018,33.7960857978771,
34.2810203821523,34.7659549664276,35.2508895507029,35.7358241349782,36.2207587192535,
36.7056933035287,37.190627887804,37.6755624720793,38.1604970563546,38.6454316406299,
39.1303662249051,39.6153008091804,40.1002353934557,40.585169977731,41.0701045620062,
41.5550391462815),.UNSPECIFIED.);
#215=B_SPLINE_SURFACE_WITH_KNOTS('',3,3,((#33463,#33464,#33465,#33466,#33467,
#33468,#33469,#33470,#33471,#33472,#33473,#33474,#33475,#33476,#33477,#33478,
#33479,#33480,#33481,#33482,#33483,#33484,#33485,#33486,#33487,#33488,#33489,
#33490,#33491,#33492,#33493,#33494,#33495,#33496,#33497,#33498,#33499,#33500,
#33501,#33502,#33503,#33504,#33505,#33506,#33507,#33508,#33509,#33510,#33511,
#33512,#33513,#33514,#33515,#33516,#33517,#33518,#33519,#33520,#33521),
(#33522,#33523,#33524,#33525,#33526,#33527,#33528,#33529,#33530,#33531,
#33532,#33533,#33534,#33535,#33536,#33537,#33538,#33539,#33540,#33541,#33542,
#33543,#33544,#33545,#33546,#33547,#33548,#33549,#33550,#33551,#33552,#33553,
#33554,#33555,#33556,#33557,#33558,#33559,#33560,#33561,#33562,#33563,#33564,
#33565,#33566,#33567,#33568,#33569,#33570,#33571,#33572,#33573,#33574,#33575,
#33576,#33577,#33578,#33579,#33580),(#33581,#33582,#33583,#33584,#33585,
#33586,#33587,#33588,#33589,#33590,#33591,#33592,#33593,#33594,#33595,#33596,
#33597,#33598,#33599,#33600,#33601,#33602,#33603,#33604,#33605,#33606,#33607,
#33608,#33609,#33610,#33611,#33612,#33613,#33614,#33615,#33616,#33617,#33618,
#33619,#33620,#33621,#33622,#33623,#33624,#33625,#33626,#33627,#33628,#33629,
#33630,#33631,#33632,#33633,#33634,#33635,#33636,#33637,#33638,#33639),
(#33640,#33641,#33642,#33643,#33644,#33645,#33646,#33647,#33648,#33649,
#33650,#33651,#33652,#33653,#33654,#33655,#33656,#33657,#33658,#33659,#33660,
#33661,#33662,#33663,#33664,#33665,#33666,#33667,#33668,#33669,#33670,#33671,
#33672,#33673,#33674,#33675,#33676,#33677,#33678,#33679,#33680,#33681,#33682,
#33683,#33684,#33685,#33686,#33687,#33688,#33689,#33690,#33691,#33692,#33693,
#33694,#33695,#33696,#33697,#33698)),.UNSPECIFIED.,.F.,.F.,.F.,(4,4),(4,
1,1,1,1,1,1,1,1,1,1,1,1,1,1,1,1,1,1,1,1,1,1,1,1,1,1,1,1,1,1,1,1,1,1,1,1,
1,1,1,1,1,1,1,1,1,1,1,1,1,1,1,1,1,1,1,4),(0.,0.193239135097767),(11.852035964745,
12.3369705490203,12.8219051332955,13.3068397175708,13.7917743018461,14.2767088861214,
14.7616434703967,15.2465780546719,15.7315126389472,16.2164472232225,16.7013818074978,
17.1863163917731,17.6712509760483,18.1561855603236,18.6411201445989,19.1260547288742,
19.6109893131494,20.0959238974247,20.5808584817,21.0657930659753,21.5507276502506,
22.0356622345258,22.5205968188011,23.0055314030764,23.4904659873517,23.9754005716269,
24.4603351559022,24.9452697401775,25.4302043244528,25.9151389087281,26.4000734930033,
26.8850080772786,27.3699426615539,27.8548772458292,28.3398118301045,28.8247464143797,
29.309680998655,29.7946155829303,30.2795501672056,30.7644847514808,31.2494193357561,
31.7343539200314,32.2192885043067,32.704223088582,33.1891576728572,33.6740922571325,
34.1590268414078,34.6439614256831,35.1288960099583,35.6138305942336,36.0987651785089,
36.5836997627842,37.0686343470595,37.5535689313347,38.03850351561,38.5234380998853,
39.0083726841606),.UNSPECIFIED.);
#216=B_SPLINE_SURFACE_WITH_KNOTS('',3,3,((#33897,#33898,#33899,#33900,#33901,
#33902,#33903,#33904,#33905,#33906,#33907,#33908,#33909,#33910,#33911,#33912,
#33913,#33914,#33915,#33916,#33917,#33918,#33919,#33920,#33921,#33922,#33923,
#33924,#33925,#33926,#33927,#33928,#33929,#33930,#33931,#33932,#33933,#33934,
#33935,#33936,#33937,#33938,#33939,#33940,#33941,#33942,#33943,#33944,#33945,
#33946,#33947,#33948,#33949,#33950,#33951,#33952,#33953,#33954,#33955),
(#33956,#33957,#33958,#33959,#33960,#33961,#33962,#33963,#33964,#33965,
#33966,#33967,#33968,#33969,#33970,#33971,#33972,#33973,#33974,#33975,#33976,
#33977,#33978,#33979,#33980,#33981,#33982,#33983,#33984,#33985,#33986,#33987,
#33988,#33989,#33990,#33991,#33992,#33993,#33994,#33995,#33996,#33997,#33998,
#33999,#34000,#34001,#34002,#34003,#34004,#34005,#34006,#34007,#34008,#34009,
#34010,#34011,#34012,#34013,#34014),(#34015,#34016,#34017,#34018,#34019,
#34020,#34021,#34022,#34023,#34024,#34025,#34026,#34027,#34028,#34029,#34030,
#34031,#34032,#34033,#34034,#34035,#34036,#34037,#34038,#34039,#34040,#34041,
#34042,#34043,#34044,#34045,#34046,#34047,#34048,#34049,#34050,#34051,#34052,
#34053,#34054,#34055,#34056,#34057,#34058,#34059,#34060,#34061,#34062,#34063,
#34064,#34065,#34066,#34067,#34068,#34069,#34070,#34071,#34072,#34073),
(#34074,#34075,#34076,#34077,#34078,#34079,#34080,#34081,#34082,#34083,
#34084,#34085,#34086,#34087,#34088,#34089,#34090,#34091,#34092,#34093,#34094,
#34095,#34096,#34097,#34098,#34099,#34100,#34101,#34102,#34103,#34104,#34105,
#34106,#34107,#34108,#34109,#34110,#34111,#34112,#34113,#34114,#34115,#34116,
#34117,#34118,#34119,#34120,#34121,#34122,#34123,#34124,#34125,#34126,#34127,
#34128,#34129,#34130,#34131,#34132)),.UNSPECIFIED.,.F.,.F.,.F.,(4,4),(4,
1,1,1,1,1,1,1,1,1,1,1,1,1,1,1,1,1,1,1,1,1,1,1,1,1,1,1,1,1,1,1,1,1,1,1,1,
1,1,1,1,1,1,1,1,1,1,1,1,1,1,1,1,1,1,1,4),(0.,0.193239135097767),(14.3987024268659,
14.8836370111412,15.3685715954165,15.8535061796917,16.338440763967,16.8233753482423,
17.3083099325176,17.7932445167929,18.2781791010681,18.7631136853434,19.2480482696187,
19.732982853894,20.2179174381693,20.7028520224445,21.1877866067198,21.6727211909951,
22.1576557752704,22.6425903595456,23.1275249438209,23.6124595280962,24.0973941123715,
24.5823286966468,25.067263280922,25.5521978651973,26.0371324494726,26.5220670337479,
27.0070016180232,27.4919362022984,27.9768707865737,28.461805370849,28.9467399551243,
29.4316745393995,29.9166091236748,30.4015437079501,30.8864782922254,31.3714128765007,
31.8563474607759,32.3412820450512,32.8262166293265,33.3111512136018,33.7960857978771,
34.2810203821523,34.7659549664276,35.2508895507029,35.7358241349782,36.2207587192535,
36.7056933035287,37.190627887804,37.6755624720793,38.1604970563546,38.6454316406298,
39.1303662249051,39.6153008091804,40.1002353934557,40.585169977731,41.0701045620062,
41.5550391462815),.UNSPECIFIED.);
#217=B_SPLINE_CURVE_WITH_KNOTS('',3,(#11779,#11780,#11781,#11782,#11783,
#11784,#11785,#11786,#11787,#11788),.UNSPECIFIED.,.F.,.F.,(4,3,3,4),(-4.09293042013064,
-3.3387479513909,-2.58456548265116,-2.07680027204819),.UNSPECIFIED.);
#218=B_SPLINE_CURVE_WITH_KNOTS('',3,(#11791,#11792,#11793,#11794,#11795,
#11796,#11797,#11798,#11799,#11800),.UNSPECIFIED.,.F.,.F.,(4,3,3,4),(0.,
0.49974386100078,0.99948772200156,1.12546250550931),.UNSPECIFIED.);
#219=B_SPLINE_CURVE_WITH_KNOTS('',3,(#11805,#11806,#11807,#11808,#11809,
#11810,#11811,#11812,#11813,#11814,#11815,#11816,#11817,#11818,#11819,#11820,
#11821,#11822,#11823,#11824,#11825,#11826,#11827,#11828,#11829),
 .UNSPECIFIED.,.F.,.F.,(4,3,3,3,3,3,3,3,4),(-10.3761157273102,-9.99487722001567,
-8.9953894980141,-7.99590177601253,-6.99641405401097,-5.9969263320094,-4.99743861000784,
-4.49769474900705,-4.09293042013064),.UNSPECIFIED.);
#220=B_SPLINE_CURVE_WITH_KNOTS('',3,(#11830,#11831,#11832,#11833,#11834,
#11835,#11836,#11837,#11838,#11839,#11840,#11841,#11842,#11843,#11844,#11845,
#11846,#11847,#11848,#11849,#11850,#11851,#11852,#11853,#11854),
 .UNSPECIFIED.,.F.,.F.,(4,3,3,3,3,3,3,3,4),(1.12546250550931,1.99897544400314,
2.99846316600472,3.99795088800629,4.49769474900708,4.99743861000787,5.99692633200945,
6.99641405401103,7.4086478126889),.UNSPECIFIED.);
#221=B_SPLINE_CURVE_WITH_KNOTS('',3,(#11859,#11860,#11861,#11862,#11863,
#11864,#11865,#11866,#11867,#11868,#11869,#11870,#11871,#11872,#11873,#11874,
#11875,#11876,#11877,#11878,#11879,#11880,#11881,#11882,#11883,#11884,#11885,
#11886),.UNSPECIFIED.,.F.,.F.,(4,3,3,3,3,3,3,3,3,4),(-16.6593010344898,
-15.9051185657501,-15.1509360970104,-14.3967536282706,-13.6425711595309,
-12.8883886907912,-12.1342062220514,-11.3800237533117,-10.625841284572,
-10.3761157273102),.UNSPECIFIED.);
#222=B_SPLINE_CURVE_WITH_KNOTS('',3,(#11887,#11888,#11889,#11890,#11891,
#11892,#11893,#11894,#11895,#11896,#11897,#11898,#11899,#11900,#11901,#11902,
#11903,#11904,#11905,#11906,#11907,#11908,#11909,#11910,#11911,#11912,#11913,
#11914),.UNSPECIFIED.,.F.,.F.,(4,3,3,3,3,3,3,3,3,4),(7.4086478126889,8.16283028142863,
8.91701275016836,9.67119521890809,10.4253776876478,11.1795601563876,11.9337426251273,
12.687925093867,13.4421075626068,13.6918331198685),.UNSPECIFIED.);
#223=B_SPLINE_CURVE_WITH_KNOTS('',3,(#11919,#11920,#11921,#11922,#11923,
#11924,#11925,#11926,#11927,#11928,#11929,#11930,#11931,#11932,#11933,#11934,
#11935,#11936,#11937,#11938,#11939,#11940,#11941,#11942,#11943,#11944,#11945,
#11946),.UNSPECIFIED.,.F.,.F.,(4,3,3,3,3,3,3,3,3,4),(-22.9424863416694,
-22.1883038729297,-21.4341214041899,-20.6799389354502,-19.9257564667105,
-19.1715739979707,-18.417391529231,-17.6632090604913,-16.9090265917515,
-16.6593010344898),.UNSPECIFIED.);
#224=B_SPLINE_CURVE_WITH_KNOTS('',3,(#11947,#11948,#11949,#11950,#11951,
#11952,#11953,#11954,#11955,#11956,#11957,#11958,#11959,#11960,#11961,#11962,
#11963,#11964,#11965,#11966,#11967,#11968,#11969,#11970,#11971),
 .UNSPECIFIED.,.F.,.F.,(4,3,3,3,3,3,3,3,4),(13.6918331198685,13.9928281080218,
14.9923158300234,15.991803552025,16.9912912740266,17.4910351350274,17.9907789960282,
18.9902667180298,19.9750184270481),.UNSPECIFIED.);
#225=B_SPLINE_CURVE_WITH_KNOTS('',3,(#11976,#11977,#11978,#11979,#11980,
#11981,#11982,#11983,#11984,#11985,#11986,#11987,#11988,#11989,#11990,#11991,
#11992,#11993,#11994,#11995,#11996,#11997,#11998,#11999,#12000,#12001,#12002,
#12003),.UNSPECIFIED.,.F.,.F.,(4,3,3,3,3,3,3,3,3,4),(-29.225671648849,-28.4714891801093,
-27.7173067113695,-26.9631242426298,-26.2089417738901,-25.4547593051504,
-24.7005768364106,-23.9463943676709,-23.1922118989312,-22.9424863416694),
 .UNSPECIFIED.);
#226=B_SPLINE_CURVE_WITH_KNOTS('',3,(#12004,#12005,#12006,#12007,#12008,
#12009,#12010,#12011,#12012,#12013,#12014,#12015,#12016,#12017,#12018,#12019,
#12020,#12021,#12022,#12023,#12024,#12025,#12026,#12027,#12028,#12029,#12030,
#12031),.UNSPECIFIED.,.F.,.F.,(4,3,3,3,3,3,3,3,3,4),(19.9750184270481,20.7292008957878,
21.4833833645275,22.2375658332673,22.991748302007,23.7459307707468,24.5001132394865,
25.2542957082262,26.008478176966,26.2582037342277),.UNSPECIFIED.);
#227=B_SPLINE_CURVE_WITH_KNOTS('',3,(#12036,#12037,#12038,#12039,#12040,
#12041,#12042,#12043,#12044,#12045,#12046,#12047,#12048,#12049,#12050,#12051,
#12052,#12053,#12054,#12055,#12056,#12057,#12058,#12059,#12060,#12061,#12062,
#12063),.UNSPECIFIED.,.F.,.F.,(4,3,3,3,3,3,3,3,3,4),(-35.5088569560286,
-34.7546744872888,-34.0004920185491,-33.2463095498094,-32.4921270810696,
-31.7379446123299,-30.9837621435901,-30.2295796748504,-29.4753972061106,
-29.225671648849),.UNSPECIFIED.);
#228=B_SPLINE_CURVE_WITH_KNOTS('',3,(#12064,#12065,#12066,#12067,#12068,
#12069,#12070,#12071,#12072,#12073,#12074,#12075,#12076,#12077,#12078,#12079,
#12080,#12081,#12082,#12083,#12084,#12085,#12086,#12087,#12088,#12089,#12090,
#12091),.UNSPECIFIED.,.F.,.F.,(4,3,3,3,3,3,3,3,3,4),(26.2582037342277,27.0123862029674,
27.7665686717072,28.5207511404469,29.2749336091866,30.0291160779264,30.7832985466661,
31.5374810154059,32.2916634841456,32.5413890414072),.UNSPECIFIED.);
#229=B_SPLINE_CURVE_WITH_KNOTS('',3,(#12096,#12097,#12098,#12099,#12100,
#12101,#12102,#12103,#12104,#12105,#12106,#12107,#12108,#12109,#12110,#12111,
#12112,#12113,#12114,#12115,#12116,#12117,#12118,#12119,#12120),
 .UNSPECIFIED.,.F.,.F.,(4,3,3,3,3,3,3,3,4),(-41.7920422632082,-40.9789966020643,
-39.9795088800627,-38.9800211580611,-38.4802772970603,-37.9805334360596,
-36.981045714058,-35.9815579920564,-35.5088569560286),.UNSPECIFIED.);
#230=B_SPLINE_CURVE_WITH_KNOTS('',3,(#12121,#12122,#12123,#12124,#12125,
#12126,#12127,#12128,#12129,#12130,#12131,#12132,#12133,#12134,#12135,#12136,
#12137,#12138,#12139,#12140,#12141,#12142,#12143,#12144,#12145,#12146,#12147,
#12148),.UNSPECIFIED.,.F.,.F.,(4,3,3,3,3,3,3,3,3,4),(32.5413890414072,33.295571510147,
34.0497539788867,34.8039364476264,35.5581189163662,36.3123013851059,37.0664838538456,
37.8206663225853,38.5748487913251,38.8245743485868),.UNSPECIFIED.);
#231=B_SPLINE_CURVE_WITH_KNOTS('',3,(#12153,#12154,#12155,#12156,#12157,
#12158,#12159,#12160,#12161,#12162,#12163,#12164,#12165,#12166,#12167,#12168,
#12169,#12170,#12171,#12172,#12173,#12174,#12175,#12176,#12177,#12178,#12179,
#12180),.UNSPECIFIED.,.F.,.F.,(4,3,3,3,3,3,3,3,3,4),(-48.0752275703878,
-47.321045101648,-46.5668626329083,-45.8126801641685,-45.0584976954288,
-44.304315226689,-43.5501327579493,-42.7959502892096,-42.0417678204698,
-41.7920422632082),.UNSPECIFIED.);
#232=B_SPLINE_CURVE_WITH_KNOTS('',3,(#12181,#12182,#12183,#12184,#12185,
#12186,#12187,#12188,#12189,#12190,#12191,#12192,#12193,#12194,#12195,#12196,
#12197,#12198,#12199,#12200,#12201,#12202,#12203,#12204,#12205,#12206,#12207,
#12208),.UNSPECIFIED.,.F.,.F.,(4,3,3,3,3,3,3,3,3,4),(38.8245743485868,39.5787568173266,
40.3329392860663,41.087121754806,41.8413042235457,42.5954866922855,43.3496691610252,
44.1038516297649,44.8580340985047,45.1077596557664),.UNSPECIFIED.);
#233=B_SPLINE_CURVE_WITH_KNOTS('',3,(#12213,#12214,#12215,#12216,#12217,
#12218,#12219,#12220,#12221,#12222,#12223,#12224,#12225,#12226,#12227,#12228,
#12229,#12230,#12231,#12232,#12233,#12234,#12235,#12236,#12237,#12238,#12239,
#12240),.UNSPECIFIED.,.F.,.F.,(4,3,3,3,3,3,3,3,3,4),(-54.3584128775674,
-53.6042304088276,-52.8500479400879,-52.0958654713482,-51.3416830026084,
-50.5875005338687,-49.833318065129,-49.0791355963893,-48.3249531276495,
-48.0752275703878),.UNSPECIFIED.);
#234=B_SPLINE_CURVE_WITH_KNOTS('',3,(#12241,#12242,#12243,#12244,#12245,
#12246,#12247,#12248,#12249,#12250,#12251,#12252,#12253,#12254,#12255,#12256,
#12257,#12258,#12259,#12260,#12261,#12262,#12263,#12264,#12265,#12266,#12267,
#12268),.UNSPECIFIED.,.F.,.F.,(4,3,3,3,3,3,3,3,3,4),(45.1077596557664,45.8619421245062,
46.6161245932459,47.3703070619856,48.1244895307253,48.8786719994651,49.6328544682048,
50.3870369369445,51.1412194056842,51.390944962946),.UNSPECIFIED.);
#235=B_SPLINE_CURVE_WITH_KNOTS('',3,(#12273,#12274,#12275,#12276,#12277,
#12278,#12279,#12280,#12281,#12282,#12283,#12284,#12285,#12286,#12287,#12288,
#12289,#12290,#12291,#12292,#12293,#12294,#12295,#12296,#12297,#12298,#12299,
#12300),.UNSPECIFIED.,.F.,.F.,(4,3,3,3,3,3,3,3,3,4),(-60.6415981847469,
-59.8874157160072,-59.1332332472675,-58.3790507785277,-57.624868309788,
-56.8706858410483,-56.1165033723085,-55.3623209035688,-54.6081384348291,
-54.3584128775674),.UNSPECIFIED.);
#236=B_SPLINE_CURVE_WITH_KNOTS('',3,(#12301,#12302,#12303,#12304,#12305,
#12306,#12307,#12308,#12309,#12310,#12311,#12312,#12313,#12314,#12315,#12316,
#12317,#12318,#12319,#12320,#12321,#12322,#12323,#12324,#12325,#12326,#12327,
#12328),.UNSPECIFIED.,.F.,.F.,(4,3,3,3,3,3,3,3,3,4),(51.390944962946,52.1451274316857,
52.8993099004255,53.6534923691652,54.4076748379049,55.1618573066447,55.9160397753844,
56.6702222441241,57.4244047128638,57.6741302701256),.UNSPECIFIED.);
#237=B_SPLINE_CURVE_WITH_KNOTS('',3,(#12333,#12334,#12335,#12336,#12337,
#12338,#12339,#12340,#12341,#12342,#12343,#12344,#12345,#12346,#12347,#12348,
#12349,#12350,#12351,#12352,#12353,#12354,#12355,#12356,#12357,#12358,#12359,
#12360),.UNSPECIFIED.,.F.,.F.,(4,3,3,3,3,3,3,3,3,4),(-66.9247834919265,
-66.1706010231868,-65.4164185544471,-64.6622360857073,-63.9080536169676,
-63.1538711482279,-62.3996886794882,-61.6455062107484,-60.8913237420087,
-60.6415981847469),.UNSPECIFIED.);
#238=B_SPLINE_CURVE_WITH_KNOTS('',3,(#12361,#12362,#12363,#12364,#12365,
#12366,#12367,#12368,#12369,#12370,#12371,#12372,#12373,#12374,#12375,#12376,
#12377,#12378,#12379,#12380,#12381,#12382,#12383,#12384,#12385,#12386,#12387,
#12388),.UNSPECIFIED.,.F.,.F.,(4,3,3,3,3,3,3,3,3,4),(57.6741302701256,58.4283127388654,
59.1824952076051,59.9366776763448,60.6908601450845,61.4450426138243,62.199225082564,
62.9534075513037,63.7075900200434,63.9573155773052),.UNSPECIFIED.);
#239=B_SPLINE_CURVE_WITH_KNOTS('',3,(#12393,#12394,#12395,#12396,#12397,
#12398,#12399,#12400,#12401,#12402,#12403,#12404,#12405,#12406,#12407,#12408,
#12409,#12410,#12411,#12412,#12413,#12414,#12415,#12416,#12417,#12418,#12419,
#12420),.UNSPECIFIED.,.F.,.F.,(4,3,3,3,3,3,3,3,3,4),(-73.2079687991061,
-72.4537863303664,-71.6996038616266,-70.9454213928869,-70.1912389241472,
-69.4370564554074,-68.6828739866677,-67.9286915179279,-67.1745090491882,
-66.9247834919265),.UNSPECIFIED.);
#240=B_SPLINE_CURVE_WITH_KNOTS('',3,(#12421,#12422,#12423,#12424,#12425,
#12426,#12427,#12428,#12429,#12430,#12431,#12432,#12433,#12434,#12435,#12436,
#12437,#12438,#12439,#12440,#12441,#12442,#12443,#12444,#12445,#12446,#12447,
#12448),.UNSPECIFIED.,.F.,.F.,(4,3,3,3,3,3,3,3,3,4),(63.9573155773052,63.9672142081004,
64.9667019301019,65.9661896521034,66.4659335131042,66.965677374105,67.9651650961065,
68.9646528181081,69.9641405401096,70.2405008844848),.UNSPECIFIED.);
#241=B_SPLINE_CURVE_WITH_KNOTS('',3,(#12453,#12454,#12455,#12456,#12457,
#12458,#12459,#12460,#12461,#12462,#12463,#12464,#12465,#12466,#12467,#12468,
#12469,#12470,#12471,#12472,#12473,#12474,#12475,#12476,#12477,#12478,#12479,
#12480),.UNSPECIFIED.,.F.,.F.,(4,3,3,3,3,3,3,3,3,4),(-79.4911541062857,
-78.736971637546,-77.9827891688063,-77.2286067000665,-76.4744242313268,
-75.7202417625871,-74.9660592938474,-74.2118768251076,-73.4576943563679,
-73.2079687991061),.UNSPECIFIED.);
#242=B_SPLINE_CURVE_WITH_KNOTS('',3,(#12481,#12482,#12483,#12484,#12485,
#12486,#12487,#12488,#12489,#12490,#12491,#12492,#12493,#12494,#12495,#12496,
#12497,#12498,#12499,#12500,#12501,#12502,#12503,#12504,#12505),
 .UNSPECIFIED.,.F.,.F.,(4,3,3,3,3,3,3,3,4),(70.2405008844848,70.9636282621112,
71.9631159841128,72.9626037061144,73.4623475671152,73.962091428116,74.9615791501176,
75.9610668721191,76.5236861916644),.UNSPECIFIED.);
#243=B_SPLINE_CURVE_WITH_KNOTS('',3,(#12510,#12511,#12512,#12513,#12514,
#12515,#12516,#12517,#12518,#12519,#12520,#12521,#12522,#12523,#12524,#12525,
#12526,#12527,#12528,#12529,#12530,#12531,#12532,#12533,#12534,#12535,#12536,
#12537),.UNSPECIFIED.,.F.,.F.,(4,3,3,3,3,3,3,3,3,4),(-85.7743394134653,
-85.0201569447256,-84.2659744759859,-83.5117920072462,-82.7576095385065,
-82.0034270697667,-81.249244601027,-80.4950621322873,-79.7408796635476,
-79.4911541062857),.UNSPECIFIED.);
#244=B_SPLINE_CURVE_WITH_KNOTS('',3,(#12538,#12539,#12540,#12541,#12542,
#12543,#12544,#12545,#12546,#12547,#12548,#12549,#12550,#12551,#12552,#12553,
#12554,#12555,#12556,#12557,#12558,#12559,#12560,#12561,#12562,#12563,#12564,
#12565),.UNSPECIFIED.,.F.,.F.,(4,3,3,3,3,3,3,3,3,4),(76.5236861916644,77.2778686604041,
78.0320511291438,78.7862335978835,79.5404160666232,80.2945985353629,81.0487810041027,
81.8029634728424,82.5571459415821,82.806871498844),.UNSPECIFIED.);
#245=B_SPLINE_CURVE_WITH_KNOTS('',3,(#12570,#12571,#12572,#12573,#12574,
#12575,#12576,#12577,#12578,#12579,#12580,#12581,#12582,#12583,#12584,#12585,
#12586,#12587,#12588,#12589,#12590,#12591,#12592,#12593,#12594,#12595,#12596,
#12597),.UNSPECIFIED.,.F.,.F.,(4,3,3,3,3,3,3,3,3,4),(-92.0575247206449,
-91.3033422519052,-90.5491597831655,-89.7949773144257,-89.040794845686,
-88.2866123769463,-87.5324299082066,-86.7782474394668,-86.0240649707271,
-85.7743394134653),.UNSPECIFIED.);
#246=B_SPLINE_CURVE_WITH_KNOTS('',3,(#12598,#12599,#12600,#12601,#12602,
#12603,#12604,#12605,#12606,#12607,#12608,#12609,#12610,#12611,#12612,#12613,
#12614,#12615,#12616,#12617,#12618,#12619,#12620,#12621,#12622,#12623,#12624,
#12625),.UNSPECIFIED.,.F.,.F.,(4,3,3,3,3,3,3,3,3,4),(82.806871498844,83.5610539675837,
84.3152364363234,85.0694189050632,85.8236013738029,86.5777838425426,87.3319663112823,
88.0861487800221,88.8403312487618,89.0900568060236),.UNSPECIFIED.);
#247=B_SPLINE_CURVE_WITH_KNOTS('',3,(#12630,#12631,#12632,#12633,#12634,
#12635,#12636,#12637,#12638,#12639,#12640,#12641,#12642,#12643,#12644,#12645,
#12646,#12647,#12648,#12649,#12650,#12651,#12652,#12653,#12654,#12655,#12656,
#12657),.UNSPECIFIED.,.F.,.F.,(4,3,3,3,3,3,3,3,3,4),(-98.3407100278245,
-97.5865275590848,-96.832345090345,-96.0781626216053,-95.3239801528655,
-94.5697976841258,-93.8156152153861,-93.0614327466463,-92.3072502779066,
-92.0575247206449),.UNSPECIFIED.);
#248=B_SPLINE_CURVE_WITH_KNOTS('',3,(#12658,#12659,#12660,#12661,#12662,
#12663,#12664,#12665,#12666,#12667,#12668,#12669,#12670,#12671,#12672,#12673,
#12674,#12675,#12676,#12677,#12678,#12679,#12680,#12681,#12682,#12683,#12684,
#12685),.UNSPECIFIED.,.F.,.F.,(4,3,3,3,3,3,3,3,3,4),(89.0900568060236,89.8442392747633,
90.598421743503,91.3526042122428,92.1067866809825,92.8609691497222,93.615151618462,
94.3693340872017,95.1235165559414,95.3732421132032),.UNSPECIFIED.);
#249=B_SPLINE_CURVE_WITH_KNOTS('',3,(#12690,#12691,#12692,#12693,#12694,
#12695,#12696,#12697,#12698,#12699,#12700,#12701,#12702,#12703,#12704,#12705,
#12706,#12707,#12708,#12709,#12710,#12711,#12712,#12713,#12714,#12715,#12716,
#12717),.UNSPECIFIED.,.F.,.F.,(4,3,3,3,3,3,3,3,3,4),(-104.623895335004,
-103.869712866264,-103.115530397525,-102.361347928785,-101.607165460045,
-100.852982991305,-100.098800522566,-99.344618053826,-98.5904355850863,
-98.3407100278245),.UNSPECIFIED.);
#250=B_SPLINE_CURVE_WITH_KNOTS('',3,(#12718,#12719,#12720,#12721,#12722,
#12723,#12724,#12725,#12726,#12727,#12728,#12729,#12730,#12731,#12732,#12733,
#12734,#12735,#12736,#12737,#12738,#12739,#12740,#12741,#12742,#12743,#12744,
#12745),.UNSPECIFIED.,.F.,.F.,(4,3,3,3,3,3,3,3,3,4),(95.3732421132032,96.1274245819429,
96.8816070506826,97.6357895194223,98.389971988162,99.1441544569017,99.8983369256415,
100.652519394381,101.406701863121,101.656427420383),.UNSPECIFIED.);
#251=B_SPLINE_CURVE_WITH_KNOTS('',3,(#12750,#12751,#12752,#12753,#12754,
#12755,#12756,#12757,#12758,#12759,#12760,#12761,#12762,#12763,#12764,#12765,
#12766,#12767,#12768,#12769,#12770,#12771,#12772,#12773,#12774),
 .UNSPECIFIED.,.F.,.F.,(4,3,3,3,3,3,3,3,4),(-110.907080642184,-109.943649420172,
-108.944161698171,-108.44441783717,-107.944673976169,-106.945186254168,
-105.945698532166,-104.946210810165,-104.623895335004),.UNSPECIFIED.);
#252=B_SPLINE_CURVE_WITH_KNOTS('',3,(#12775,#12776,#12777,#12778,#12779,
#12780,#12781,#12782,#12783,#12784,#12785,#12786,#12787,#12788,#12789,#12790,
#12791,#12792,#12793,#12794,#12795,#12796,#12797,#12798,#12799,#12800,#12801,
#12802),.UNSPECIFIED.,.F.,.F.,(4,3,3,3,3,3,3,3,3,4),(101.656427420383,102.410609889122,
103.164792357862,103.918974826602,104.673157295342,105.427339764081,106.181522232821,
106.935704701561,107.689887170301,107.939612727562),.UNSPECIFIED.);
#253=B_SPLINE_CURVE_WITH_KNOTS('',3,(#12807,#12808,#12809,#12810,#12811,
#12812,#12813,#12814,#12815,#12816,#12817,#12818,#12819,#12820,#12821,#12822,
#12823,#12824,#12825,#12826,#12827,#12828,#12829,#12830,#12831,#12832,#12833,
#12834),.UNSPECIFIED.,.F.,.F.,(4,3,3,3,3,3,3,3,3,4),(-117.190265949363,
-116.436083480624,-115.681901011884,-114.927718543144,-114.173536074404,
-113.419353605665,-112.665171136925,-111.910988668185,-111.156806199445,
-110.907080642184),.UNSPECIFIED.);
#254=B_SPLINE_CURVE_WITH_KNOTS('',3,(#12835,#12836,#12837,#12838,#12839,
#12840,#12841,#12842,#12843,#12844,#12845,#12846,#12847,#12848,#12849,#12850,
#12851,#12852,#12853,#12854,#12855,#12856,#12857,#12858,#12859,#12860,#12861,
#12862),.UNSPECIFIED.,.F.,.F.,(4,3,3,3,3,3,3,3,3,4),(107.939612727562,108.693795196302,
109.447977665042,110.202160133782,110.956342602521,111.710525071261,112.464707540001,
113.21889000874,113.97307247748,114.222798034742),.UNSPECIFIED.);
#255=B_SPLINE_CURVE_WITH_KNOTS('',3,(#12867,#12868,#12869,#12870,#12871,
#12872,#12873,#12874,#12875,#12876,#12877,#12878,#12879,#12880,#12881,#12882,
#12883,#12884,#12885,#12886,#12887,#12888,#12889,#12890,#12891,#12892,#12893,
#12894),.UNSPECIFIED.,.F.,.F.,(4,3,3,3,3,3,3,3,3,4),(-123.473451256543,
-122.719268787803,-121.965086319063,-121.210903850324,-120.456721381584,
-119.702538912844,-118.948356444104,-118.194173975365,-117.439991506625,
-117.190265949363),.UNSPECIFIED.);
#256=B_SPLINE_CURVE_WITH_KNOTS('',3,(#12895,#12896,#12897,#12898,#12899,
#12900,#12901,#12902,#12903,#12904,#12905,#12906,#12907,#12908,#12909,#12910,
#12911,#12912,#12913,#12914,#12915,#12916,#12917,#12918,#12919,#12920,#12921,
#12922),.UNSPECIFIED.,.F.,.F.,(4,3,3,3,3,3,3,3,3,4),(114.222798034742,114.976980503482,
115.731162972221,116.485345440961,117.239527909701,117.993710378441,118.74789284718,
119.50207531592,120.25625778466,120.505983341922),.UNSPECIFIED.);
#257=B_SPLINE_CURVE_WITH_KNOTS('',3,(#12927,#12928,#12929,#12930,#12931,
#12932,#12933,#12934,#12935,#12936,#12937,#12938,#12939,#12940,#12941,#12942,
#12943,#12944,#12945,#12946,#12947,#12948,#12949,#12950,#12951,#12952,#12953,
#12954),.UNSPECIFIED.,.F.,.F.,(4,3,3,3,3,3,3,3,3,4),(-129.756636563722,
-129.002454094983,-128.248271626243,-127.494089157503,-126.739906688764,
-125.985724220024,-125.231541751284,-124.477359282544,-123.723176813805,
-123.473451256543),.UNSPECIFIED.);
#258=B_SPLINE_CURVE_WITH_KNOTS('',3,(#12955,#12956,#12957,#12958,#12959,
#12960,#12961,#12962,#12963,#12964,#12965,#12966,#12967,#12968,#12969,#12970,
#12971,#12972,#12973,#12974,#12975,#12976,#12977,#12978,#12979,#12980,#12981,
#12982),.UNSPECIFIED.,.F.,.F.,(4,3,3,3,3,3,3,3,3,4),(120.505983341922,121.260165810661,
122.014348279401,122.768530748141,123.52271321688,124.27689568562,125.03107815436,
125.7852606231,126.539443091839,126.789168649101),.UNSPECIFIED.);
#259=B_SPLINE_CURVE_WITH_KNOTS('',3,(#12987,#12988,#12989,#12990,#12991,
#12992,#12993,#12994,#12995,#12996,#12997,#12998,#12999,#13000,#13001,#13002,
#13003,#13004,#13005,#13006,#13007,#13008,#13009,#13010,#13011,#13012,#13013,
#13014),.UNSPECIFIED.,.F.,.F.,(4,3,3,3,3,3,3,3,3,4),(-136.039821870902,
-135.285639402162,-134.531456933423,-133.777274464683,-133.023091995943,
-132.268909527203,-131.514727058464,-130.760544589724,-130.006362120984,
-129.756636563722),.UNSPECIFIED.);
#260=B_SPLINE_CURVE_WITH_KNOTS('',3,(#13015,#13016,#13017,#13018,#13019,
#13020,#13021,#13022,#13023,#13024,#13025,#13026,#13027,#13028,#13029,#13030,
#13031,#13032,#13033,#13034,#13035,#13036,#13037,#13038,#13039,#13040,#13041,
#13042),.UNSPECIFIED.,.F.,.F.,(4,3,3,3,3,3,3,3,3,4),(126.789168649101,127.543351117841,
128.297533586581,129.05171605532,129.80589852406,130.5600809928,131.31426346154,
132.068445930279,132.822628399019,133.072353956281),.UNSPECIFIED.);
#261=B_SPLINE_CURVE_WITH_KNOTS('',3,(#13047,#13048,#13049,#13050,#13051,
#13052,#13053,#13054,#13055,#13056,#13057,#13058,#13059,#13060,#13061,#13062,
#13063,#13064,#13065,#13066,#13067,#13068,#13069,#13070,#13071),
 .UNSPECIFIED.,.F.,.F.,(4,3,3,3,3,3,3,3,4),(-142.323007178082,-141.927256524223,
-140.927768802221,-139.928281080219,-138.928793358218,-137.929305636216,
-136.929817914215,-136.430074053214,-136.039821870902),.UNSPECIFIED.);
#262=B_SPLINE_CURVE_WITH_KNOTS('',3,(#13072,#13073,#13074,#13075,#13076,
#13077,#13078,#13079,#13080,#13081,#13082,#13083,#13084,#13085,#13086,#13087,
#13088,#13089,#13090,#13091,#13092,#13093,#13094,#13095,#13096),
 .UNSPECIFIED.,.F.,.F.,(4,3,3,3,3,3,3,3,4),(133.072353956281,133.93135474821,
134.930842470212,135.930330192213,136.430074053214,136.929817914215,137.929305636216,
138.928793358218,139.35553926346),.UNSPECIFIED.);
#263=B_SPLINE_CURVE_WITH_KNOTS('',3,(#13101,#13102,#13103,#13104,#13105,
#13106,#13107,#13108,#13109,#13110,#13111,#13112,#13113,#13114,#13115,#13116,
#13117,#13118,#13119,#13120,#13121,#13122,#13123,#13124,#13125,#13126,#13127,
#13128),.UNSPECIFIED.,.F.,.F.,(4,3,3,3,3,3,3,3,3,4),(-148.606192485261,
-147.852010016521,-147.097827547782,-146.343645079042,-145.589462610302,
-144.835280141562,-144.081097672823,-143.326915204083,-142.572732735343,
-142.323007178082),.UNSPECIFIED.);
#264=B_SPLINE_CURVE_WITH_KNOTS('',3,(#13129,#13130,#13131,#13132,#13133,
#13134,#13135,#13136,#13137,#13138,#13139,#13140,#13141,#13142,#13143,#13144,
#13145,#13146,#13147,#13148,#13149,#13150,#13151,#13152,#13153,#13154,#13155,
#13156),.UNSPECIFIED.,.F.,.F.,(4,3,3,3,3,3,3,3,3,4),(139.35553926346,140.1097217322,
140.86390420094,141.61808666968,142.372269138419,143.126451607159,143.880634075899,
144.634816544639,145.388999013378,145.63872457064),.UNSPECIFIED.);
#265=B_SPLINE_CURVE_WITH_KNOTS('',3,(#13161,#13162,#13163,#13164,#13165,
#13166,#13167,#13168,#13169,#13170,#13171,#13172,#13173,#13174,#13175,#13176,
#13177,#13178,#13179,#13180,#13181,#13182,#13183,#13184,#13185,#13186,#13187,
#13188),.UNSPECIFIED.,.F.,.F.,(4,3,3,3,3,3,3,3,3,4),(-154.889377792441,
-154.135195323701,-153.381012854961,-152.626830386222,-151.872647917482,
-151.118465448742,-150.364282980002,-149.610100511263,-148.855918042523,
-148.606192485261),.UNSPECIFIED.);
#266=B_SPLINE_CURVE_WITH_KNOTS('',3,(#13189,#13190,#13191,#13192,#13193,
#13194,#13195,#13196,#13197,#13198,#13199,#13200,#13201,#13202,#13203,#13204,
#13205,#13206,#13207,#13208,#13209,#13210,#13211,#13212,#13213,#13214,#13215,
#13216),.UNSPECIFIED.,.F.,.F.,(4,3,3,3,3,3,3,3,3,4),(145.63872457064,146.39290703938,
147.147089508119,147.901271976859,148.655454445599,149.409636914339,150.163819383078,
150.918001851818,151.672184320558,151.921909877819),.UNSPECIFIED.);
#267=B_SPLINE_CURVE_WITH_KNOTS('',3,(#13221,#13222,#13223,#13224,#13225,
#13226,#13227,#13228,#13229,#13230,#13231,#13232,#13233,#13234,#13235,#13236,
#13237,#13238,#13239,#13240,#13241,#13242,#13243,#13244,#13245,#13246,#13247,
#13248),.UNSPECIFIED.,.F.,.F.,(4,3,3,3,3,3,3,3,3,4),(-161.17256309962,-160.418380630881,
-159.664198162141,-158.910015693401,-158.155833224661,-157.401650755922,
-156.647468287182,-155.893285818442,-155.139103349702,-154.889377792441),
 .UNSPECIFIED.);
#268=B_SPLINE_CURVE_WITH_KNOTS('',3,(#13249,#13250,#13251,#13252,#13253,
#13254,#13255,#13256,#13257,#13258,#13259,#13260,#13261,#13262,#13263,#13264,
#13265,#13266,#13267,#13268,#13269,#13270,#13271,#13272,#13273,#13274,#13275,
#13276),.UNSPECIFIED.,.F.,.F.,(4,3,3,3,3,3,3,3,3,4),(151.921909877819,152.676092346559,
153.430274815299,154.184457284039,154.938639752778,155.692822221518,156.447004690258,
157.201187158998,157.955369627737,158.205095184999),.UNSPECIFIED.);
#269=B_SPLINE_CURVE_WITH_KNOTS('',3,(#13281,#13282,#13283,#13284,#13285,
#13286,#13287,#13288,#13289,#13290,#13291,#13292,#13293,#13294,#13295,#13296,
#13297,#13298,#13299,#13300,#13301,#13302,#13303,#13304,#13305),
 .UNSPECIFIED.,.F.,.F.,(4,3,3,3,3,3,3,3,4),(-167.4557484068,-166.914449574262,
-165.91496185226,-164.915474130259,-164.415730269258,-163.915986408257,
-162.916498686255,-161.917010964254,-161.17256309962),.UNSPECIFIED.);
#270=B_SPLINE_CURVE_WITH_KNOTS('',3,(#13306,#13307,#13308,#13309,#13310,
#13311,#13312,#13313,#13314,#13315,#13316,#13317,#13318,#13319,#13320,#13321,
#13322,#13323,#13324,#13325,#13326,#13327,#13328,#13329,#13330,#13331,#13332,
#13333),.UNSPECIFIED.,.F.,.F.,(4,3,3,3,3,3,3,3,3,4),(158.205095184999,158.959277653739,
159.713460122478,160.467642591218,161.221825059958,161.976007528697,162.730189997437,
163.484372466177,164.238554934916,164.488280492179),.UNSPECIFIED.);
#271=B_SPLINE_CURVE_WITH_KNOTS('',3,(#13338,#13339,#13340,#13341,#13342,
#13343,#13344,#13345,#13346,#13347,#13348,#13349,#13350,#13351,#13352,#13353,
#13354,#13355,#13356,#13357,#13358,#13359,#13360,#13361,#13362,#13363,#13364,
#13365),.UNSPECIFIED.,.F.,.F.,(4,3,3,3,3,3,3,3,3,4),(-173.738933713979,
-172.98475124524,-172.2305687765,-171.47638630776,-170.72220383902,-169.968021370281,
-169.213838901541,-168.459656432801,-167.705473964061,-167.4557484068),
 .UNSPECIFIED.);
#272=B_SPLINE_CURVE_WITH_KNOTS('',3,(#13366,#13367,#13368,#13369,#13370,
#13371,#13372,#13373,#13374,#13375,#13376,#13377,#13378,#13379,#13380,#13381,
#13382,#13383,#13384,#13385,#13386,#13387,#13388,#13389,#13390,#13391,#13392,
#13393),.UNSPECIFIED.,.F.,.F.,(4,3,3,3,3,3,3,3,3,4),(164.488280492179,165.242462960918,
165.996645429658,166.750827898398,167.505010367137,168.259192835877,169.013375304617,
169.767557773357,170.521740242096,170.771465799358),.UNSPECIFIED.);
#273=B_SPLINE_CURVE_WITH_KNOTS('',3,(#13398,#13399,#13400,#13401,#13402,
#13403,#13404,#13405,#13406,#13407,#13408,#13409,#13410,#13411,#13412,#13413,
#13414,#13415,#13416,#13417,#13418,#13419,#13420,#13421,#13422,#13423,#13424,
#13425),.UNSPECIFIED.,.F.,.F.,(4,3,3,3,3,3,3,3,3,4),(-180.022119021159,
-179.267936552419,-178.513754083679,-177.75957161494,-177.0053891462,-176.25120667746,
-175.497024208721,-174.742841739981,-173.988659271241,-173.738933713979),
 .UNSPECIFIED.);
#274=B_SPLINE_CURVE_WITH_KNOTS('',3,(#13426,#13427,#13428,#13429,#13430,
#13431,#13432,#13433,#13434,#13435,#13436,#13437,#13438,#13439,#13440,#13441,
#13442,#13443,#13444,#13445,#13446,#13447,#13448,#13449,#13450,#13451,#13452,
#13453),.UNSPECIFIED.,.F.,.F.,(4,3,3,3,3,3,3,3,3,4),(170.771465799358,171.525648268098,
172.279830736838,173.034013205577,173.788195674317,174.542378143057,175.296560611797,
176.050743080536,176.804925549276,177.054651106538),.UNSPECIFIED.);
#275=B_SPLINE_CURVE_WITH_KNOTS('',3,(#13458,#13459,#13460,#13461,#13462,
#13463,#13464,#13465,#13466,#13467,#13468,#13469,#13470,#13471,#13472,#13473,
#13474,#13475,#13476,#13477,#13478,#13479,#13480,#13481,#13482,#13483,#13484,
#13485),.UNSPECIFIED.,.F.,.F.,(4,3,3,3,3,3,3,3,3,4),(-186.305304328339,
-185.551121859599,-184.796939390859,-184.042756922119,-183.28857445338,
-182.53439198464,-181.7802095159,-181.026027047161,-180.271844578421,-180.022119021159),
 .UNSPECIFIED.);
#276=B_SPLINE_CURVE_WITH_KNOTS('',3,(#13486,#13487,#13488,#13489,#13490,
#13491,#13492,#13493,#13494,#13495,#13496,#13497,#13498,#13499,#13500,#13501,
#13502,#13503,#13504,#13505,#13506,#13507,#13508,#13509,#13510,#13511,#13512,
#13513),.UNSPECIFIED.,.F.,.F.,(4,3,3,3,3,3,3,3,3,4),(177.054651106538,177.808833575277,
178.563016044017,179.317198512757,180.071380981497,180.825563450236,181.579745918976,
182.333928387716,183.088110856456,183.337836413717),.UNSPECIFIED.);
#277=B_SPLINE_CURVE_WITH_KNOTS('',3,(#13518,#13519,#13520,#13521,#13522,
#13523,#13524,#13525,#13526,#13527,#13528,#13529,#13530,#13531,#13532,#13533,
#13534,#13535,#13536,#13537,#13538,#13539,#13540,#13541,#13542,#13543,#13544,
#13545),.UNSPECIFIED.,.F.,.F.,(4,3,3,3,3,3,3,3,3,4),(-192.588489635518,
-191.834307166778,-191.080124698039,-190.325942229299,-189.571759760559,
-188.817577291819,-188.06339482308,-187.30921235434,-186.5550298856,-186.305304328339),
 .UNSPECIFIED.);
#278=B_SPLINE_CURVE_WITH_KNOTS('',3,(#13546,#13547,#13548,#13549,#13550,
#13551,#13552,#13553,#13554,#13555,#13556,#13557,#13558,#13559,#13560,#13561,
#13562,#13563,#13564,#13565,#13566,#13567,#13568,#13569,#13570,#13571,#13572,
#13573),.UNSPECIFIED.,.F.,.F.,(4,3,3,3,3,3,3,3,3,4),(183.337836413717,184.092018882457,
184.846201351197,185.600383819936,186.354566288676,187.108748757416,187.862931226156,
188.617113694895,189.371296163635,189.621021720897),.UNSPECIFIED.);
#279=B_SPLINE_CURVE_WITH_KNOTS('',3,(#13578,#13579,#13580,#13581,#13582,
#13583,#13584,#13585,#13586,#13587,#13588,#13589,#13590,#13591,#13592,#13593,
#13594,#13595,#13596,#13597,#13598,#13599,#13600,#13601,#13602,#13603,#13604,
#13605),.UNSPECIFIED.,.F.,.F.,(4,3,3,3,3,3,3,3,3,4),(-198.871674942698,
-198.117492473958,-197.363310005218,-196.609127536478,-195.854945067739,
-195.100762598999,-194.346580130259,-193.592397661519,-192.83821519278,
-192.588489635518),.UNSPECIFIED.);
#280=B_SPLINE_CURVE_WITH_KNOTS('',3,(#13606,#13607,#13608,#13609,#13610,
#13611,#13612,#13613,#13614,#13615,#13616,#13617,#13618,#13619,#13620,#13621,
#13622,#13623,#13624,#13625,#13626,#13627,#13628,#13629,#13630,#13631,#13632,
#13633),.UNSPECIFIED.,.F.,.F.,(4,3,3,3,3,3,3,3,3,4),(189.621021720897,190.375204189637,
191.129386658376,191.883569127116,192.637751595856,193.391934064595,194.146116533335,
194.900299002075,195.654481470815,195.904207028076),.UNSPECIFIED.);
#281=B_SPLINE_CURVE_WITH_KNOTS('',3,(#13638,#13639,#13640,#13641,#13642,
#13643,#13644,#13645,#13646,#13647,#13648,#13649,#13650,#13651,#13652,#13653,
#13654,#13655,#13656,#13657,#13658,#13659,#13660,#13661,#13662,#13663,#13664,
#13665),.UNSPECIFIED.,.F.,.F.,(4,3,3,3,3,3,3,3,3,4),(-205.154860249877,
-204.400677781137,-203.646495312398,-202.892312843658,-202.138130374918,
-201.383947906178,-200.629765437439,-199.875582968699,-199.121400499959,
-198.871674942698),.UNSPECIFIED.);
#282=B_SPLINE_CURVE_WITH_KNOTS('',3,(#13666,#13667,#13668,#13669,#13670,
#13671,#13672,#13673,#13674,#13675,#13676,#13677,#13678,#13679,#13680,#13681,
#13682,#13683,#13684,#13685,#13686,#13687,#13688,#13689,#13690,#13691,#13692,
#13693),.UNSPECIFIED.,.F.,.F.,(4,3,3,3,3,3,3,3,3,4),(195.904207028076,196.658389496816,
197.412571965556,198.166754434296,198.920936903035,199.675119371775,200.429301840515,
201.183484309255,201.937666777995,202.187392335256),.UNSPECIFIED.);
#283=B_SPLINE_CURVE_WITH_KNOTS('',3,(#13698,#13699,#13700,#13701,#13702,
#13703,#13704,#13705,#13706,#13707,#13708,#13709,#13710,#13711,#13712,#13713,
#13714,#13715,#13716,#13717,#13718,#13719,#13720,#13721,#13722,#13723,#13724,
#13725),.UNSPECIFIED.,.F.,.F.,(4,3,3,3,3,3,3,3,3,4),(-211.438045557057,
-210.683863088317,-209.929680619577,-209.175498150838,-208.421315682098,
-207.667133213358,-206.912950744618,-206.158768275878,-205.404585807139,
-205.154860249877),.UNSPECIFIED.);
#284=B_SPLINE_CURVE_WITH_KNOTS('',3,(#13726,#13727,#13728,#13729,#13730,
#13731,#13732,#13733,#13734,#13735,#13736,#13737,#13738,#13739,#13740,#13741,
#13742,#13743,#13744,#13745,#13746,#13747,#13748,#13749,#13750,#13751,#13752,
#13753),.UNSPECIFIED.,.F.,.F.,(4,3,3,3,3,3,3,3,3,4),(202.187392335256,202.941574803996,
203.695757272735,204.449939741475,205.204122210215,205.958304678955,206.712487147694,
207.466669616434,208.220852085174,208.470577642436),.UNSPECIFIED.);
#285=B_SPLINE_CURVE_WITH_KNOTS('',3,(#13758,#13759,#13760,#13761,#13762,
#13763,#13764,#13765,#13766,#13767,#13768,#13769,#13770,#13771,#13772,#13773,
#13774,#13775,#13776,#13777,#13778,#13779,#13780,#13781,#13782,#13783,#13784,
#13785),.UNSPECIFIED.,.F.,.F.,(4,3,3,3,3,3,3,3,3,4),(-217.721230864236,
-216.967048395497,-216.212865926757,-215.458683458017,-214.704500989278,
-213.950318520538,-213.196136051798,-212.441953583058,-211.687771114319,
-211.438045557057),.UNSPECIFIED.);
#286=B_SPLINE_CURVE_WITH_KNOTS('',3,(#13786,#13787,#13788,#13789,#13790,
#13791,#13792,#13793,#13794,#13795,#13796,#13797,#13798,#13799,#13800,#13801,
#13802,#13803,#13804,#13805,#13806,#13807,#13808,#13809,#13810,#13811,#13812,
#13813),.UNSPECIFIED.,.F.,.F.,(4,3,3,3,3,3,3,3,3,4),(208.470577642436,209.224760111175,
209.978942579915,210.733125048655,211.487307517394,212.241489986134,212.995672454874,
213.749854923614,214.504037392353,214.753762949615),.UNSPECIFIED.);
#287=B_SPLINE_CURVE_WITH_KNOTS('',3,(#13818,#13819,#13820,#13821,#13822,
#13823,#13824,#13825,#13826,#13827,#13828,#13829,#13830,#13831,#13832,#13833,
#13834,#13835,#13836,#13837,#13838,#13839,#13840,#13841,#13842,#13843,#13844,
#13845),.UNSPECIFIED.,.F.,.F.,(4,3,3,3,3,3,3,3,3,4),(-224.004416171416,
-223.250233702676,-222.496051233936,-221.741868765197,-220.987686296457,
-220.233503827717,-219.479321358978,-218.725138890238,-217.970956421498,
-217.721230864236),.UNSPECIFIED.);
#288=B_SPLINE_CURVE_WITH_KNOTS('',3,(#13846,#13847,#13848,#13849,#13850,
#13851,#13852,#13853,#13854,#13855,#13856,#13857,#13858,#13859,#13860,#13861,
#13862,#13863,#13864,#13865,#13866,#13867,#13868,#13869,#13870,#13871,#13872,
#13873),.UNSPECIFIED.,.F.,.F.,(4,3,3,3,3,3,3,3,3,4),(214.753762949615,215.507945418355,
216.262127887095,217.016310355834,217.770492824574,218.524675293314,219.278857762054,
220.033040230793,220.787222699533,221.036948256795),.UNSPECIFIED.);
#289=B_SPLINE_CURVE_WITH_KNOTS('',3,(#13878,#13879,#13880,#13881,#13882,
#13883,#13884,#13885,#13886,#13887,#13888,#13889,#13890,#13891,#13892,#13893,
#13894,#13895,#13896,#13897,#13898,#13899,#13900,#13901,#13902),
 .UNSPECIFIED.,.F.,.F.,(4,3,3,3,3,3,3,3,4),(-230.287601478596,-229.88217606036,
-228.882688338359,-227.883200616357,-227.383456755357,-226.883712894356,
-225.884225172354,-224.884737450353,-224.004416171416),.UNSPECIFIED.);
#290=B_SPLINE_CURVE_WITH_KNOTS('',3,(#13903,#13904,#13905,#13906,#13907,
#13908,#13909,#13910,#13911,#13912,#13913,#13914,#13915,#13916,#13917,#13918,
#13919,#13920,#13921,#13922,#13923,#13924,#13925,#13926,#13927,#13928,#13929,
#13930),.UNSPECIFIED.,.F.,.F.,(4,3,3,3,3,3,3,3,3,4),(221.036948256795,221.791130725534,
222.545313194274,223.299495663014,224.053678131754,224.807860600493,225.562043069233,
226.316225537973,227.070408006713,227.320133563974),.UNSPECIFIED.);
#291=B_SPLINE_CURVE_WITH_KNOTS('',3,(#13935,#13936,#13937,#13938,#13939,
#13940,#13941,#13942,#13943,#13944,#13945,#13946,#13947,#13948,#13949,#13950,
#13951,#13952,#13953,#13954,#13955,#13956,#13957,#13958,#13959,#13960,#13961,
#13962),.UNSPECIFIED.,.F.,.F.,(4,3,3,3,3,3,3,3,3,4),(-236.570786785775,
-235.816604317035,-235.062421848296,-234.308239379556,-233.554056910816,
-232.799874442076,-232.045691973336,-231.291509504597,-230.537327035857,
-230.287601478596),.UNSPECIFIED.);
#292=B_SPLINE_CURVE_WITH_KNOTS('',3,(#13963,#13964,#13965,#13966,#13967,
#13968,#13969,#13970,#13971,#13972,#13973,#13974,#13975,#13976,#13977,#13978,
#13979,#13980,#13981,#13982,#13983,#13984,#13985,#13986,#13987,#13988,#13989,
#13990),.UNSPECIFIED.,.F.,.F.,(4,3,3,3,3,3,3,3,3,4),(227.320133563974,228.074316032714,
228.828498501454,229.582680970193,230.336863438933,231.091045907673,231.845228376413,
232.599410845153,233.353593313892,233.603318871154),.UNSPECIFIED.);
#293=B_SPLINE_CURVE_WITH_KNOTS('',3,(#13995,#13996,#13997,#13998,#13999,
#14000,#14001,#14002,#14003,#14004,#14005,#14006,#14007,#14008,#14009,#14010,
#14011,#14012,#14013,#14014,#14015,#14016,#14017,#14018,#14019,#14020,#14021,
#14022),.UNSPECIFIED.,.F.,.F.,(4,3,3,3,3,3,3,3,3,4),(-242.853972092955,
-242.099789624215,-241.345607155475,-240.591424686735,-239.837242217996,
-239.083059749256,-238.328877280516,-237.574694811776,-236.820512343037,
-236.570786785775),.UNSPECIFIED.);
#294=B_SPLINE_CURVE_WITH_KNOTS('',3,(#14023,#14024,#14025,#14026,#14027,
#14028,#14029,#14030,#14031,#14032,#14033,#14034,#14035,#14036,#14037,#14038,
#14039,#14040,#14041,#14042,#14043,#14044,#14045,#14046,#14047,#14048,#14049,
#14050),.UNSPECIFIED.,.F.,.F.,(4,3,3,3,3,3,3,3,3,4),(233.603318871154,234.357501339894,
235.111683808633,235.865866277373,236.620048746113,237.374231214852,238.128413683592,
238.882596152332,239.636778621072,239.886504178333),.UNSPECIFIED.);
#295=B_SPLINE_CURVE_WITH_KNOTS('',3,(#14055,#14056,#14057,#14058,#14059,
#14060,#14061,#14062,#14063,#14064,#14065,#14066,#14067,#14068,#14069,#14070,
#14071,#14072,#14073,#14074,#14075,#14076,#14077,#14078,#14079,#14080,#14081,
#14082),.UNSPECIFIED.,.F.,.F.,(4,3,3,3,3,3,3,3,3,4),(-249.137157400134,
-248.382974931394,-247.628792462655,-246.874609993915,-246.120427525175,
-245.366245056435,-244.612062587695,-243.857880118956,-243.103697650216,
-242.853972092955),.UNSPECIFIED.);
#296=B_SPLINE_CURVE_WITH_KNOTS('',3,(#14083,#14084,#14085,#14086,#14087,
#14088,#14089,#14090,#14091,#14092,#14093,#14094,#14095,#14096,#14097,#14098,
#14099,#14100,#14101,#14102,#14103,#14104,#14105,#14106,#14107,#14108,#14109,
#14110),.UNSPECIFIED.,.F.,.F.,(4,3,3,3,3,3,3,3,3,4),(239.886504178333,240.640686647073,
241.394869115813,242.149051584552,242.903234053292,243.657416522032,244.411598990772,
245.165781459511,245.919963928251,246.169689485513),.UNSPECIFIED.);
#297=B_SPLINE_CURVE_WITH_KNOTS('',3,(#14115,#14116,#14117,#14118,#14119,
#14120,#14121,#14122,#14123,#14124,#14125,#14126,#14127,#14128,#14129,#14130,
#14131,#14132,#14133,#14134,#14135,#14136,#14137,#14138,#14139,#14140,#14141,
#14142),.UNSPECIFIED.,.F.,.F.,(4,3,3,3,3,3,3,3,3,4),(-255.420342707314,
-254.666160238574,-253.911977769834,-253.157795301094,-252.403612832355,
-251.649430363615,-250.895247894875,-250.141065426135,-249.386882957396,
-249.137157400134),.UNSPECIFIED.);
#298=B_SPLINE_CURVE_WITH_KNOTS('',3,(#14143,#14144,#14145,#14146,#14147,
#14148,#14149,#14150,#14151,#14152,#14153,#14154,#14155,#14156,#14157,#14158,
#14159,#14160,#14161,#14162,#14163,#14164,#14165,#14166,#14167,#14168,#14169,
#14170),.UNSPECIFIED.,.F.,.F.,(4,3,3,3,3,3,3,3,3,4),(246.169689485513,246.923871954253,
247.678054422992,248.432236891732,249.186419360471,249.940601829211,250.694784297951,
251.44896676669,252.20314923543,252.452874792692),.UNSPECIFIED.);
#299=B_SPLINE_CURVE_WITH_KNOTS('',3,(#14175,#14176,#14177,#14178,#14179,
#14180,#14181,#14182,#14183,#14184,#14185,#14186,#14187,#14188,#14189,#14190,
#14191,#14192,#14193,#14194,#14195,#14196,#14197,#14198,#14199,#14200,#14201,
#14202),.UNSPECIFIED.,.F.,.F.,(4,3,3,3,3,3,3,3,3,4),(-261.703528014493,
-260.949345545754,-260.195163077014,-259.440980608274,-258.686798139535,
-257.932615670795,-257.178433202055,-256.424250733315,-255.670068264576,
-255.420342707314),.UNSPECIFIED.);
#300=B_SPLINE_CURVE_WITH_KNOTS('',3,(#14203,#14204,#14205,#14206,#14207,
#14208,#14209,#14210,#14211,#14212,#14213,#14214,#14215,#14216,#14217,#14218,
#14219,#14220,#14221,#14222,#14223,#14224,#14225,#14226,#14227),
 .UNSPECIFIED.,.F.,.F.,(4,3,3,3,3,3,3,3,4),(252.452874792692,252.870393666397,
253.869881388398,254.8693691104,255.369112971401,255.868856832401,256.868344554403,
257.867832276404,258.736060099872),.UNSPECIFIED.);
#301=B_SPLINE_CURVE_WITH_KNOTS('',3,(#14232,#14233,#14234,#14235,#14236,
#14237,#14238,#14239,#14240,#14241,#14242,#14243,#14244,#14245,#14246,#14247,
#14248,#14249,#14250,#14251,#14252,#14253,#14254,#14255,#14256,#14257,#14258,
#14259),.UNSPECIFIED.,.F.,.F.,(4,3,3,3,3,3,3,3,3,4),(-267.986713321673,
-267.232530852933,-266.478348384194,-265.724165915454,-264.969983446714,
-264.215800977974,-263.461618509235,-262.707436040495,-261.953253571755,
-261.703528014493),.UNSPECIFIED.);
#302=B_SPLINE_CURVE_WITH_KNOTS('',3,(#14260,#14261,#14262,#14263,#14264,
#14265,#14266,#14267,#14268,#14269,#14270,#14271,#14272,#14273,#14274,#14275,
#14276,#14277,#14278,#14279,#14280,#14281,#14282,#14283,#14284,#14285,#14286,
#14287),.UNSPECIFIED.,.F.,.F.,(4,3,3,3,3,3,3,3,3,4),(258.736060099872,259.490242568612,
260.244425037352,260.998607506091,261.752789974831,262.506972443571,263.261154912311,
264.01533738105,264.76951984979,265.019245407052),.UNSPECIFIED.);
#303=B_SPLINE_CURVE_WITH_KNOTS('',3,(#14292,#14293,#14294,#14295,#14296,
#14297,#14298,#14299,#14300,#14301,#14302,#14303,#14304,#14305,#14306,#14307,
#14308,#14309,#14310,#14311,#14312,#14313,#14314,#14315,#14316,#14317,#14318,
#14319),.UNSPECIFIED.,.F.,.F.,(4,3,3,3,3,3,3,3,3,4),(-274.269898628852,
-273.515716160113,-272.761533691373,-272.007351222633,-271.253168753893,
-270.498986285153,-269.744803816413,-268.990621347674,-268.236438878934,
-267.986713321673),.UNSPECIFIED.);
#304=B_SPLINE_CURVE_WITH_KNOTS('',3,(#14320,#14321,#14322,#14323,#14324,
#14325,#14326,#14327,#14328,#14329,#14330,#14331,#14332,#14333,#14334,#14335,
#14336,#14337,#14338,#14339,#14340,#14341,#14342,#14343,#14344,#14345,#14346,
#14347),.UNSPECIFIED.,.F.,.F.,(4,3,3,3,3,3,3,3,3,4),(265.019245407052,265.773427875791,
266.527610344531,267.281792813271,268.03597528201,268.79015775075,269.54434021949,
270.29852268823,271.052705156969,271.302430714231),.UNSPECIFIED.);
#305=B_SPLINE_CURVE_WITH_KNOTS('',3,(#14352,#14353,#14354,#14355,#14356,
#14357,#14358,#14359,#14360,#14361,#14362,#14363,#14364,#14365,#14366,#14367,
#14368,#14369,#14370,#14371,#14372,#14373,#14374,#14375,#14376,#14377,#14378,
#14379),.UNSPECIFIED.,.F.,.F.,(4,3,3,3,3,3,3,3,3,4),(-280.553083936032,
-279.798901467292,-279.044718998553,-278.290536529813,-277.536354061073,
-276.782171592333,-276.027989123593,-275.273806654854,-274.519624186114,
-274.269898628852),.UNSPECIFIED.);
#306=B_SPLINE_CURVE_WITH_KNOTS('',3,(#14380,#14381,#14382,#14383,#14384,
#14385,#14386,#14387,#14388,#14389,#14390,#14391,#14392,#14393,#14394,#14395,
#14396,#14397,#14398,#14399,#14400,#14401,#14402,#14403,#14404,#14405,#14406,
#14407),.UNSPECIFIED.,.F.,.F.,(4,3,3,3,3,3,3,3,3,4),(271.302430714231,272.056613182971,
272.810795651711,273.56497812045,274.31916058919,275.07334305793,275.82752552667,
276.58170799541,277.335890464149,277.585616021411),.UNSPECIFIED.);
#307=B_SPLINE_CURVE_WITH_KNOTS('',3,(#14412,#14413,#14414,#14415,#14416,
#14417,#14418,#14419,#14420,#14421,#14422,#14423,#14424,#14425,#14426,#14427,
#14428,#14429,#14430,#14431,#14432,#14433,#14434,#14435,#14436,#14437,#14438,
#14439),.UNSPECIFIED.,.F.,.F.,(4,3,3,3,3,3,3,3,3,4),(-286.836269243212,
-286.082086774472,-285.327904305732,-284.573721836992,-283.819539368252,
-283.065356899512,-282.311174430773,-281.556991962033,-280.802809493293,
-280.553083936032),.UNSPECIFIED.);
#308=B_SPLINE_CURVE_WITH_KNOTS('',3,(#14440,#14441,#14442,#14443,#14444,
#14445,#14446,#14447,#14448,#14449,#14450,#14451,#14452,#14453,#14454,#14455,
#14456,#14457,#14458,#14459,#14460,#14461,#14462,#14463,#14464,#14465,#14466,
#14467),.UNSPECIFIED.,.F.,.F.,(4,3,3,3,3,3,3,3,3,4),(277.585616021411,278.33979849015,
279.09398095889,279.84816342763,280.60234589637,281.356528365109,282.110710833849,
282.864893302589,283.619075771328,283.86880132859),.UNSPECIFIED.);
#309=B_SPLINE_CURVE_WITH_KNOTS('',3,(#14472,#14473,#14474,#14475,#14476,
#14477,#14478,#14479,#14480,#14481,#14482,#14483,#14484,#14485,#14486,#14487,
#14488,#14489,#14490,#14491,#14492,#14493,#14494,#14495,#14496,#14497,#14498,
#14499),.UNSPECIFIED.,.F.,.F.,(4,3,3,3,3,3,3,3,3,4),(-293.119454550391,
-292.365272081651,-291.611089612912,-290.856907144172,-290.102724675432,
-289.348542206692,-288.594359737953,-287.840177269213,-287.085994800473,
-286.836269243212),.UNSPECIFIED.);
#310=B_SPLINE_CURVE_WITH_KNOTS('',3,(#14500,#14501,#14502,#14503,#14504,
#14505,#14506,#14507,#14508,#14509,#14510,#14511,#14512,#14513,#14514,#14515,
#14516,#14517,#14518,#14519,#14520,#14521,#14522,#14523,#14524,#14525,#14526,
#14527),.UNSPECIFIED.,.F.,.F.,(4,3,3,3,3,3,3,3,3,4),(283.86880132859,284.62298379733,
285.37716626607,286.131348734809,286.885531203549,287.639713672289,288.393896141029,
289.148078609768,289.902261078508,290.15198663577),.UNSPECIFIED.);
#311=B_SPLINE_CURVE_WITH_KNOTS('',3,(#14532,#14533,#14534,#14535,#14536,
#14537,#14538,#14539,#14540,#14541,#14542,#14543,#14544,#14545,#14546,#14547,
#14548,#14549,#14550,#14551,#14552,#14553,#14554,#14555,#14556,#14557,#14558,
#14559),.UNSPECIFIED.,.F.,.F.,(4,3,3,3,3,3,3,3,3,4),(-299.402639857571,
-298.648457388831,-297.894274920091,-297.140092451352,-296.385909982612,
-295.631727513872,-294.877545045133,-294.123362576393,-293.369180107653,
-293.119454550391),.UNSPECIFIED.);
#312=B_SPLINE_CURVE_WITH_KNOTS('',3,(#14560,#14561,#14562,#14563,#14564,
#14565,#14566,#14567,#14568,#14569,#14570,#14571,#14572,#14573,#14574,#14575,
#14576,#14577,#14578,#14579,#14580,#14581,#14582,#14583,#14584,#14585,#14586,
#14587),.UNSPECIFIED.,.F.,.F.,(4,3,3,3,3,3,3,3,3,4),(290.15198663577,290.90616910451,
291.660351573249,292.414534041989,293.168716510729,293.922898979468,294.677081448208,
295.431263916948,296.185446385687,296.435171942949),.UNSPECIFIED.);
#313=B_SPLINE_CURVE_WITH_KNOTS('',3,(#14592,#14593,#14594,#14595,#14596,
#14597,#14598,#14599,#14600,#14601,#14602,#14603,#14604,#14605,#14606,#14607,
#14608,#14609,#14610,#14611,#14612,#14613,#14614,#14615,#14616),
 .UNSPECIFIED.,.F.,.F.,(4,3,3,3,3,3,3,3,4),(-305.68582516475,-304.843755210478,
-303.844267488476,-302.844779766475,-302.345035905474,-301.845292044473,
-300.845804322472,-299.84631660047,-299.402639857571),.UNSPECIFIED.);
#314=B_SPLINE_CURVE_WITH_KNOTS('',3,(#14617,#14618,#14619,#14620,#14621,
#14622,#14623,#14624,#14625,#14626,#14627,#14628,#14629,#14630,#14631,#14632,
#14633,#14634,#14635,#14636,#14637,#14638,#14639,#14640,#14641,#14642,#14643,
#14644),.UNSPECIFIED.,.F.,.F.,(4,3,3,3,3,3,3,3,3,4),(296.435171942949,297.189354411689,
297.943536880429,298.697719349169,299.451901817908,300.206084286648,300.960266755388,
301.714449224128,302.468631692868,302.718357250129),.UNSPECIFIED.);
#315=B_SPLINE_CURVE_WITH_KNOTS('',3,(#14649,#14650,#14651,#14652,#14653,
#14654,#14655,#14656,#14657,#14658,#14659,#14660,#14661,#14662,#14663,#14664,
#14665,#14666,#14667,#14668,#14669,#14670,#14671,#14672,#14673,#14674,#14675,
#14676),.UNSPECIFIED.,.F.,.F.,(4,3,3,3,3,3,3,3,3,4),(-311.96901047193,-311.21482800319,
-310.46064553445,-309.706463065711,-308.952280596971,-308.198098128231,
-307.443915659491,-306.689733190751,-305.935550722012,-305.68582516475),
 .UNSPECIFIED.);
#316=B_SPLINE_CURVE_WITH_KNOTS('',3,(#14677,#14678,#14679,#14680,#14681,
#14682,#14683,#14684,#14685,#14686,#14687,#14688,#14689,#14690,#14691,#14692,
#14693,#14694,#14695,#14696,#14697,#14698,#14699,#14700,#14701,#14702,#14703,
#14704),.UNSPECIFIED.,.F.,.F.,(4,3,3,3,3,3,3,3,3,4),(302.718357250129,303.472539718869,
304.226722187608,304.980904656348,305.735087125088,306.489269593828,307.243452062567,
307.997634531307,308.751817000047,309.001542557308),.UNSPECIFIED.);
#317=B_SPLINE_CURVE_WITH_KNOTS('',3,(#14709,#14710,#14711,#14712,#14713,
#14714,#14715,#14716,#14717,#14718,#14719,#14720,#14721,#14722,#14723,#14724,
#14725,#14726,#14727,#14728,#14729,#14730,#14731,#14732,#14733,#14734,#14735,
#14736),.UNSPECIFIED.,.F.,.F.,(4,3,3,3,3,3,3,3,3,4),(-318.25219577911,-317.49801331037,
-316.74383084163,-315.98964837289,-315.23546590415,-314.481283435411,-313.727100966671,
-312.972918497931,-312.218736029191,-311.96901047193),.UNSPECIFIED.);
#318=B_SPLINE_CURVE_WITH_KNOTS('',3,(#14737,#14738,#14739,#14740,#14741,
#14742,#14743,#14744,#14745,#14746,#14747,#14748,#14749,#14750,#14751,#14752,
#14753,#14754,#14755,#14756,#14757,#14758,#14759,#14760,#14761,#14762,#14763,
#14764),.UNSPECIFIED.,.F.,.F.,(4,3,3,3,3,3,3,3,3,4),(309.001542557308,309.755725026048,
310.509907494788,311.264089963528,312.018272432267,312.772454901007,313.526637369747,
314.280819838486,315.035002307226,315.284727864488),.UNSPECIFIED.);
#319=B_SPLINE_CURVE_WITH_KNOTS('',3,(#14769,#14770,#14771,#14772,#14773,
#14774,#14775,#14776,#14777,#14778,#14779,#14780,#14781,#14782,#14783,#14784,
#14785,#14786,#14787,#14788,#14789,#14790,#14791,#14792,#14793,#14794,#14795,
#14796),.UNSPECIFIED.,.F.,.F.,(4,3,3,3,3,3,3,3,3,4),(-324.535381086289,
-323.781198617549,-323.027016148809,-322.27283368007,-321.51865121133,-320.76446874259,
-320.01028627385,-319.256103805111,-318.501921336371,-318.25219577911),
 .UNSPECIFIED.);
#320=B_SPLINE_CURVE_WITH_KNOTS('',3,(#14797,#14798,#14799,#14800,#14801,
#14802,#14803,#14804,#14805,#14806,#14807,#14808,#14809,#14810,#14811,#14812,
#14813,#14814,#14815,#14816,#14817,#14818,#14819,#14820,#14821,#14822,#14823,
#14824),.UNSPECIFIED.,.F.,.F.,(4,3,3,3,3,3,3,3,3,4),(315.284727864488,316.038910333228,
316.793092801967,317.547275270707,318.301457739447,319.055640208187,319.809822676926,
320.564005145666,321.318187614406,321.567913171668),.UNSPECIFIED.);
#321=B_SPLINE_CURVE_WITH_KNOTS('',3,(#14829,#14830,#14831,#14832,#14833,
#14834,#14835,#14836,#14837,#14838,#14839,#14840,#14841,#14842,#14843,#14844,
#14845,#14846,#14847,#14848,#14849,#14850,#14851,#14852,#14853,#14854,#14855,
#14856),.UNSPECIFIED.,.F.,.F.,(4,3,3,3,3,3,3,3,3,4),(-330.818566393469,
-330.064383924729,-329.310201455989,-328.556018987249,-327.80183651851,
-327.04765404977,-326.29347158103,-325.539289112291,-324.785106643551,-324.535381086289),
 .UNSPECIFIED.);
#322=B_SPLINE_CURVE_WITH_KNOTS('',3,(#14857,#14858,#14859,#14860,#14861,
#14862,#14863,#14864,#14865,#14866,#14867,#14868,#14869,#14870,#14871,#14872,
#14873,#14874,#14875,#14876,#14877,#14878,#14879,#14880,#14881,#14882,#14883,
#14884),.UNSPECIFIED.,.F.,.F.,(4,3,3,3,3,3,3,3,3,4),(321.567913171668,322.322095640407,
323.076278109147,323.830460577887,324.584643046626,325.338825515366,326.093007984106,
326.847190452846,327.601372921585,327.851098478847),.UNSPECIFIED.);
#323=B_SPLINE_CURVE_WITH_KNOTS('',3,(#14889,#14890,#14891,#14892,#14893,
#14894,#14895,#14896,#14897,#14898,#14899,#14900,#14901,#14902,#14903,#14904,
#14905,#14906,#14907,#14908,#14909,#14910,#14911,#14912,#14913,#14914,#14915,
#14916),.UNSPECIFIED.,.F.,.F.,(4,3,3,3,3,3,3,3,3,4),(-337.101751700648,
-336.347569231908,-335.593386763168,-334.839204294429,-334.085021825689,
-333.330839356949,-332.576656888209,-331.822474419469,-331.06829195073,
-330.818566393469),.UNSPECIFIED.);
#324=B_SPLINE_CURVE_WITH_KNOTS('',3,(#14917,#14918,#14919,#14920,#14921,
#14922,#14923,#14924,#14925,#14926,#14927,#14928,#14929,#14930,#14931,#14932,
#14933,#14934,#14935,#14936,#14937,#14938,#14939,#14940,#14941),
 .UNSPECIFIED.,.F.,.F.,(4,3,3,3,3,3,3,3,4),(327.851098478847,328.831460538516,
329.830948260517,330.330692121518,330.830435982519,331.829923704521,332.829411426522,
333.828899148524,334.134283786027),.UNSPECIFIED.);
#325=B_SPLINE_CURVE_WITH_KNOTS('',3,(#14946,#14947,#14948,#14949,#14950,
#14951,#14952,#14953,#14954,#14955,#14956,#14957,#14958,#14959,#14960,#14961,
#14962,#14963,#14964,#14965,#14966,#14967,#14968,#14969,#14970,#14971,#14972,
#14973),.UNSPECIFIED.,.F.,.F.,(4,3,3,3,3,3,3,3,3,4),(-343.384937007828,
-342.630754539088,-341.876572070348,-341.122389601608,-340.368207132869,
-339.614024664129,-338.859842195389,-338.105659726649,-337.351477257909,
-337.101751700648),.UNSPECIFIED.);
#326=B_SPLINE_CURVE_WITH_KNOTS('',3,(#14974,#14975,#14976,#14977,#14978,
#14979,#14980,#14981,#14982,#14983,#14984,#14985,#14986,#14987,#14988,#14989,
#14990,#14991,#14992,#14993,#14994,#14995,#14996,#14997,#14998,#14999,#15000,
#15001),.UNSPECIFIED.,.F.,.F.,(4,3,3,3,3,3,3,3,3,4),(334.134283786027,334.888466254766,
335.642648723506,336.396831192246,337.151013660986,337.905196129725,338.659378598465,
339.413561067205,340.167743535944,340.417469093206),.UNSPECIFIED.);
#327=B_SPLINE_CURVE_WITH_KNOTS('',3,(#15006,#15007,#15008,#15009,#15010,
#15011,#15012,#15013,#15014,#15015,#15016,#15017,#15018,#15019,#15020,#15021,
#15022,#15023,#15024,#15025,#15026,#15027,#15028,#15029,#15030,#15031,#15032,
#15033),.UNSPECIFIED.,.F.,.F.,(4,3,3,3,3,3,3,3,3,4),(-349.668122315007,
-348.913939846268,-348.159757377528,-347.405574908788,-346.651392440048,
-345.897209971308,-345.143027502569,-344.388845033829,-343.634662565089,
-343.384937007828),.UNSPECIFIED.);
#328=B_SPLINE_CURVE_WITH_KNOTS('',3,(#15034,#15035,#15036,#15037,#15038,
#15039,#15040,#15041,#15042,#15043,#15044,#15045,#15046,#15047,#15048,#15049,
#15050,#15051,#15052,#15053,#15054,#15055,#15056,#15057,#15058,#15059,#15060,
#15061),.UNSPECIFIED.,.F.,.F.,(4,3,3,3,3,3,3,3,3,4),(340.417469093206,341.171651561946,
341.925834030686,342.680016499426,343.434198968165,344.188381436905,344.942563905645,
345.696746374385,346.450928843124,346.700654400386),.UNSPECIFIED.);
#329=B_SPLINE_CURVE_WITH_KNOTS('',3,(#15066,#15067,#15068,#15069,#15070,
#15071,#15072,#15073,#15074,#15075,#15076,#15077,#15078,#15079,#15080,#15081,
#15082,#15083,#15084,#15085,#15086,#15087,#15088,#15089,#15090,#15091,#15092,
#15093),.UNSPECIFIED.,.F.,.F.,(4,3,3,3,3,3,3,3,3,4),(-355.951307622187,
-355.197125153447,-354.442942684707,-353.688760215967,-352.934577747228,
-352.180395278488,-351.426212809748,-350.672030341008,-349.917847872269,
-349.668122315007),.UNSPECIFIED.);
#330=B_SPLINE_CURVE_WITH_KNOTS('',3,(#15094,#15095,#15096,#15097,#15098,
#15099,#15100,#15101,#15102,#15103,#15104,#15105,#15106,#15107,#15108,#15109,
#15110,#15111,#15112,#15113,#15114,#15115,#15116,#15117,#15118,#15119,#15120,
#15121),.UNSPECIFIED.,.F.,.F.,(4,3,3,3,3,3,3,3,3,4),(346.700654400386,347.454836869126,
348.209019337865,348.963201806605,349.717384275345,350.471566744084,351.225749212824,
351.979931681564,352.734114150304,352.983839707566),.UNSPECIFIED.);
#331=B_SPLINE_CURVE_WITH_KNOTS('',3,(#15126,#15127,#15128,#15129,#15130,
#15131,#15132,#15133,#15134,#15135,#15136,#15137,#15138,#15139,#15140,#15141,
#15142,#15143,#15144,#15145,#15146,#15147,#15148,#15149,#15150,#15151,#15152,
#15153),.UNSPECIFIED.,.F.,.F.,(4,3,3,3,3,3,3,3,3,4),(-362.234492929366,
-361.480310460627,-360.726127991887,-359.971945523147,-359.217763054408,
-358.463580585668,-357.709398116928,-356.955215648188,-356.201033179449,
-355.951307622187),.UNSPECIFIED.);
#332=B_SPLINE_CURVE_WITH_KNOTS('',3,(#15154,#15155,#15156,#15157,#15158,
#15159,#15160,#15161,#15162,#15163,#15164,#15165,#15166,#15167,#15168,#15169,
#15170,#15171,#15172,#15173,#15174,#15175,#15176,#15177,#15178,#15179,#15180,
#15181),.UNSPECIFIED.,.F.,.F.,(4,3,3,3,3,3,3,3,3,4),(352.983839707566,353.738022176305,
354.492204645045,355.246387113785,356.000569582525,356.754752051264,357.508934520004,
358.263116988744,359.017299457484,359.267025014745),.UNSPECIFIED.);
#333=B_SPLINE_CURVE_WITH_KNOTS('',3,(#15186,#15187,#15188,#15189,#15190,
#15191,#15192,#15193,#15194,#15195,#15196,#15197,#15198,#15199,#15200,#15201,
#15202,#15203,#15204,#15205,#15206,#15207,#15208,#15209,#15210,#15211,#15212,
#15213),.UNSPECIFIED.,.F.,.F.,(4,3,3,3,3,3,3,3,3,4),(-368.517678236546,
-367.763495767806,-367.009313299066,-366.255130830327,-365.500948361587,
-364.746765892847,-363.992583424108,-363.238400955368,-362.484218486628,
-362.234492929366),.UNSPECIFIED.);
#334=B_SPLINE_CURVE_WITH_KNOTS('',3,(#15214,#15215,#15216,#15217,#15218,
#15219,#15220,#15221,#15222,#15223,#15224,#15225,#15226,#15227,#15228,#15229,
#15230,#15231,#15232,#15233,#15234,#15235,#15236,#15237,#15238,#15239,#15240,
#15241),.UNSPECIFIED.,.F.,.F.,(4,3,3,3,3,3,3,3,3,4),(359.267025014745,360.021207483485,
360.775389952225,361.529572420964,362.283754889704,363.037937358444,363.792119827184,
364.546302295924,365.300484764664,365.550210321925),.UNSPECIFIED.);
#335=B_SPLINE_CURVE_WITH_KNOTS('',3,(#15246,#15247,#15248,#15249,#15250,
#15251,#15252,#15253,#15254,#15255,#15256,#15257,#15258,#15259,#15260,#15261,
#15262,#15263,#15264,#15265,#15266,#15267,#15268,#15269,#15270),
 .UNSPECIFIED.,.F.,.F.,(4,3,3,3,3,3,3,3,4),(-374.800863543725,-373.808408028586,
-372.808920306584,-372.309176445584,-371.809432584583,-370.809944862581,
-369.81045714058,-368.810969418578,-368.517678236546),.UNSPECIFIED.);
#336=B_SPLINE_CURVE_WITH_KNOTS('',3,(#15271,#15272,#15273,#15274,#15275,
#15276,#15277,#15278,#15279,#15280,#15281,#15282,#15283,#15284,#15285,#15286,
#15287,#15288,#15289,#15290,#15291,#15292,#15293,#15294,#15295,#15296,#15297,
#15298),.UNSPECIFIED.,.F.,.F.,(4,3,3,3,3,3,3,3,3,4),(365.550210321925,366.304392790664,
367.058575259404,367.812757728144,368.566940196884,369.321122665623,370.075305134363,
370.829487603103,371.583670071843,371.833395629104),.UNSPECIFIED.);
#337=B_SPLINE_CURVE_WITH_KNOTS('',3,(#15303,#15304,#15305,#15306,#15307,
#15308,#15309,#15310,#15311,#15312,#15313,#15314,#15315,#15316,#15317,#15318,
#15319,#15320,#15321,#15322,#15323,#15324,#15325,#15326,#15327,#15328,#15329,
#15330),.UNSPECIFIED.,.F.,.F.,(4,3,3,3,3,3,3,3,3,4),(-381.084048850905,
-380.329866382165,-379.575683913426,-378.821501444686,-378.067318975946,
-377.313136507206,-376.558954038467,-375.804771569727,-375.050589100987,
-374.800863543725),.UNSPECIFIED.);
#338=B_SPLINE_CURVE_WITH_KNOTS('',3,(#15331,#15332,#15333,#15334,#15335,
#15336,#15337,#15338,#15339,#15340,#15341,#15342,#15343,#15344,#15345,#15346,
#15347,#15348,#15349,#15350,#15351,#15352,#15353,#15354,#15355,#15356,#15357,
#15358),.UNSPECIFIED.,.F.,.F.,(4,3,3,3,3,3,3,3,3,4),(371.833395629104,372.587578097844,
373.341760566584,374.095943035323,374.850125504063,375.604307972803,376.358490441542,
377.112672910282,377.866855379022,378.116580936284),.UNSPECIFIED.);
#339=B_SPLINE_CURVE_WITH_KNOTS('',3,(#15363,#15364,#15365,#15366,#15367,
#15368,#15369,#15370,#15371,#15372,#15373,#15374,#15375,#15376,#15377,#15378,
#15379,#15380,#15381,#15382,#15383,#15384,#15385,#15386,#15387,#15388,#15389,
#15390),.UNSPECIFIED.,.F.,.F.,(4,3,3,3,3,3,3,3,3,4),(-387.367234158085,
-386.613051689345,-385.858869220605,-385.104686751865,-384.350504283126,
-383.596321814386,-382.842139345646,-382.087956876907,-381.333774408167,
-381.084048850905),.UNSPECIFIED.);
#340=B_SPLINE_CURVE_WITH_KNOTS('',3,(#15391,#15392,#15393,#15394,#15395,
#15396,#15397,#15398,#15399,#15400,#15401,#15402,#15403,#15404,#15405,#15406,
#15407,#15408,#15409,#15410,#15411,#15412,#15413,#15414,#15415,#15416,#15417,
#15418),.UNSPECIFIED.,.F.,.F.,(4,3,3,3,3,3,3,3,3,4),(378.116580936284,378.870763405023,
379.624945873763,380.379128342503,381.133310811243,381.887493279982,382.641675748722,
383.395858217462,384.150040686201,384.399766243463),.UNSPECIFIED.);
#341=B_SPLINE_CURVE_WITH_KNOTS('',3,(#15423,#15424,#15425,#15426,#15427,
#15428,#15429,#15430,#15431,#15432,#15433,#15434,#15435,#15436,#15437,#15438,
#15439,#15440,#15441,#15442,#15443,#15444,#15445,#15446,#15447,#15448,#15449,
#15450),.UNSPECIFIED.,.F.,.F.,(4,3,3,3,3,3,3,3,3,4),(-393.650419465264,
-392.896236996525,-392.142054527785,-391.387872059045,-390.633689590305,
-389.879507121566,-389.125324652826,-388.371142184086,-387.616959715347,
-387.367234158085),.UNSPECIFIED.);
#342=B_SPLINE_CURVE_WITH_KNOTS('',3,(#15451,#15452,#15453,#15454,#15455,
#15456,#15457,#15458,#15459,#15460,#15461,#15462,#15463,#15464,#15465,#15466,
#15467,#15468,#15469,#15470,#15471,#15472,#15473,#15474,#15475,#15476,#15477,
#15478),.UNSPECIFIED.,.F.,.F.,(4,3,3,3,3,3,3,3,3,4),(384.399766243463,385.153948712203,
385.908131180943,386.662313649683,387.416496118422,388.170678587162,388.924861055902,
389.679043524642,390.433225993381,390.682951550643),.UNSPECIFIED.);
#343=B_SPLINE_CURVE_WITH_KNOTS('',3,(#15483,#15484,#15485,#15486,#15487,
#15488,#15489,#15490,#15491,#15492,#15493,#15494,#15495,#15496,#15497,#15498,
#15499,#15500,#15501,#15502,#15503,#15504,#15505,#15506,#15507,#15508,#15509,
#15510),.UNSPECIFIED.,.F.,.F.,(4,3,3,3,3,3,3,3,3,4),(-399.933604772444,
-399.179422303704,-398.425239834964,-397.671057366224,-396.916874897485,
-396.162692428745,-395.408509960005,-394.654327491265,-393.900145022526,
-393.650419465264),.UNSPECIFIED.);
#344=B_SPLINE_CURVE_WITH_KNOTS('',3,(#15511,#15512,#15513,#15514,#15515,
#15516,#15517,#15518,#15519,#15520,#15521,#15522,#15523,#15524,#15525,#15526,
#15527,#15528,#15529,#15530,#15531,#15532,#15533,#15534,#15535,#15536,#15537,
#15538),.UNSPECIFIED.,.F.,.F.,(4,3,3,3,3,3,3,3,3,4),(390.682951550643,391.437134019383,
392.191316488122,392.945498956862,393.699681425602,394.453863894341,395.208046363081,
395.962228831821,396.716411300561,396.966136857822),.UNSPECIFIED.);
#345=B_SPLINE_CURVE_WITH_KNOTS('',3,(#15543,#15544,#15545,#15546,#15547,
#15548,#15549,#15550,#15551,#15552,#15553,#15554,#15555,#15556,#15557,#15558,
#15559,#15560,#15561,#15562,#15563,#15564,#15565,#15566,#15567,#15568,#15569,
#15570),.UNSPECIFIED.,.F.,.F.,(4,3,3,3,3,3,3,3,3,4),(-406.216790079623,
-405.462607610884,-404.708425142144,-403.954242673404,-403.200060204664,
-402.445877735925,-401.691695267185,-400.937512798445,-400.183330329705,
-399.933604772444),.UNSPECIFIED.);
#346=B_SPLINE_CURVE_WITH_KNOTS('',3,(#15571,#15572,#15573,#15574,#15575,
#15576,#15577,#15578,#15579,#15580,#15581,#15582,#15583,#15584,#15585,#15586,
#15587,#15588,#15589,#15590,#15591,#15592,#15593,#15594,#15595),
 .UNSPECIFIED.,.F.,.F.,(4,3,3,3,3,3,3,3,4),(396.966136857822,397.796113356624,
398.795601078626,399.795088800627,400.294832661628,400.794576522629,401.79406424463,
402.793551966632,403.249322165002),.UNSPECIFIED.);
#347=B_SPLINE_CURVE_WITH_KNOTS('',3,(#15600,#15601,#15602,#15603,#15604,
#15605,#15606,#15607,#15608,#15609,#15610,#15611,#15612,#15613,#15614,#15615,
#15616,#15617,#15618,#15619,#15620,#15621,#15622,#15623,#15624,#15625,#15626,
#15627),.UNSPECIFIED.,.F.,.F.,(4,3,3,3,3,3,3,3,3,4),(-412.499975386803,
-411.745792918063,-410.991610449323,-410.237427980584,-409.483245511844,
-408.729063043104,-407.974880574364,-407.220698105624,-406.466515636885,
-406.216790079623),.UNSPECIFIED.);
#348=B_SPLINE_CURVE_WITH_KNOTS('',3,(#15628,#15629,#15630,#15631,#15632,
#15633,#15634,#15635,#15636,#15637,#15638,#15639,#15640,#15641,#15642,#15643,
#15644,#15645,#15646,#15647,#15648,#15649,#15650,#15651,#15652,#15653,#15654,
#15655),.UNSPECIFIED.,.F.,.F.,(4,3,3,3,3,3,3,3,3,4),(403.249322165002,404.003504633742,
404.757687102482,405.511869571221,406.266052039961,407.020234508701,407.774416977441,
408.52859944618,409.28278191492,409.532507472182),.UNSPECIFIED.);
#349=B_SPLINE_CURVE_WITH_KNOTS('',3,(#15660,#15661,#15662,#15663,#15664,
#15665,#15666,#15667,#15668,#15669,#15670,#15671,#15672,#15673,#15674,#15675,
#15676,#15677,#15678,#15679,#15680,#15681,#15682,#15683,#15684,#15685,#15686,
#15687),.UNSPECIFIED.,.F.,.F.,(4,3,3,3,3,3,3,3,3,4),(-418.783160693982,
-418.028978225243,-417.274795756503,-416.520613287763,-415.766430819024,
-415.012248350284,-414.258065881544,-413.503883412804,-412.749700944065,
-412.499975386803),.UNSPECIFIED.);
#350=B_SPLINE_CURVE_WITH_KNOTS('',3,(#15688,#15689,#15690,#15691,#15692,
#15693,#15694,#15695,#15696,#15697,#15698,#15699,#15700,#15701,#15702,#15703,
#15704,#15705,#15706,#15707,#15708,#15709,#15710,#15711,#15712,#15713,#15714,
#15715),.UNSPECIFIED.,.F.,.F.,(4,3,3,3,3,3,3,3,3,4),(409.532507472182,410.286689940921,
411.040872409661,411.795054878401,412.54923734714,413.30341981588,414.05760228462,
414.81178475336,415.565967222099,415.815692779361),.UNSPECIFIED.);
#351=B_SPLINE_CURVE_WITH_KNOTS('',3,(#15720,#15721,#15722,#15723,#15724,
#15725,#15726,#15727,#15728,#15729,#15730,#15731,#15732,#15733,#15734,#15735,
#15736,#15737,#15738,#15739,#15740,#15741,#15742,#15743,#15744,#15745,#15746,
#15747),.UNSPECIFIED.,.F.,.F.,(4,3,3,3,3,3,3,3,3,4),(-425.066346001162,
-424.782281850666,-423.782794128664,-422.783306406663,-421.783818684661,
-421.28407482366,-420.78433096266,-419.784843240658,-418.785355518657,-418.783160693982),
 .UNSPECIFIED.);
#352=B_SPLINE_CURVE_WITH_KNOTS('',3,(#15748,#15749,#15750,#15751,#15752,
#15753,#15754,#15755,#15756,#15757,#15758,#15759,#15760,#15761,#15762,#15763,
#15764,#15765,#15766,#15767,#15768,#15769,#15770,#15771,#15772,#15773,#15774,
#15775),.UNSPECIFIED.,.F.,.F.,(4,3,3,3,3,3,3,3,3,4),(415.815692779361,416.569875248101,
417.324057716841,418.07824018558,418.83242265432,419.58660512306,420.340787591799,
421.094970060539,421.849152529279,422.098878086541),.UNSPECIFIED.);
#353=B_SPLINE_CURVE_WITH_KNOTS('',3,(#15780,#15781,#15782,#15783,#15784,
#15785,#15786,#15787,#15788,#15789,#15790,#15791,#15792,#15793,#15794,#15795,
#15796,#15797,#15798,#15799,#15800,#15801,#15802,#15803,#15804),
 .UNSPECIFIED.,.F.,.F.,(4,3,3,3,3,3,3,3,4),(-431.349531308342,-430.779208182675,
-429.779720460674,-428.780232738672,-428.280488877671,-427.780745016671,
-426.781257294669,-425.781769572668,-425.066346001162),.UNSPECIFIED.);
#354=B_SPLINE_CURVE_WITH_KNOTS('',3,(#15805,#15806,#15807,#15808,#15809,
#15810,#15811,#15812,#15813,#15814,#15815,#15816,#15817,#15818,#15819,#15820,
#15821,#15822,#15823,#15824,#15825,#15826,#15827,#15828,#15829,#15830,#15831,
#15832),.UNSPECIFIED.,.F.,.F.,(4,3,3,3,3,3,3,3,3,4),(422.098878086541,422.85306055528,
423.60724302402,424.36142549276,425.1156079615,425.86979043024,426.623972898979,
427.378155367719,428.132337836459,428.38206339372),.UNSPECIFIED.);
#355=B_SPLINE_CURVE_WITH_KNOTS('',3,(#15837,#15838,#15839,#15840,#15841,
#15842,#15843,#15844,#15845,#15846,#15847,#15848,#15849,#15850,#15851,#15852,
#15853,#15854,#15855,#15856,#15857,#15858,#15859,#15860,#15861,#15862,#15863,
#15864),.UNSPECIFIED.,.F.,.F.,(4,3,3,3,3,3,3,3,3,4),(-437.632716615521,
-436.878534146781,-436.124351678042,-435.370169209302,-434.615986740562,
-433.861804271822,-433.107621803083,-432.353439334343,-431.599256865603,
-431.349531308342),.UNSPECIFIED.);
#356=B_SPLINE_CURVE_WITH_KNOTS('',3,(#15865,#15866,#15867,#15868,#15869,
#15870,#15871,#15872,#15873,#15874,#15875,#15876,#15877,#15878,#15879,#15880,
#15881,#15882,#15883,#15884,#15885,#15886,#15887,#15888,#15889,#15890,#15891,
#15892),.UNSPECIFIED.,.F.,.F.,(4,3,3,3,3,3,3,3,3,4),(428.38206339372,429.13624586246,
429.8904283312,430.644610799939,431.398793268679,432.152975737419,432.907158206158,
433.661340674898,434.415523143638,434.6652487009),.UNSPECIFIED.);
#357=B_SPLINE_CURVE_WITH_KNOTS('',3,(#15897,#15898,#15899,#15900,#15901,
#15902,#15903,#15904,#15905,#15906,#15907,#15908,#15909,#15910,#15911,#15912,
#15913,#15914,#15915,#15916,#15917,#15918,#15919,#15920,#15921,#15922,#15923,
#15924),.UNSPECIFIED.,.F.,.F.,(4,3,3,3,3,3,3,3,3,4),(-443.915901922701,
-443.161719453961,-442.407536985222,-441.653354516482,-440.899172047743,
-440.144989579003,-439.390807110263,-438.636624641524,-437.882442172784,
-437.632716615521),.UNSPECIFIED.);
#358=B_SPLINE_CURVE_WITH_KNOTS('',3,(#15925,#15926,#15927,#15928,#15929,
#15930,#15931,#15932,#15933,#15934,#15935,#15936,#15937,#15938,#15939,#15940,
#15941,#15942,#15943,#15944,#15945,#15946,#15947,#15948,#15949,#15950,#15951,
#15952),.UNSPECIFIED.,.F.,.F.,(4,3,3,3,3,3,3,3,3,4),(434.6652487009,435.41943116964,
436.173613638379,436.927796107119,437.681978575859,438.436161044599,439.190343513339,
439.944525982079,440.698708450818,440.948434008079),.UNSPECIFIED.);
#359=B_SPLINE_CURVE_WITH_KNOTS('',3,(#15957,#15958,#15959,#15960,#15961,
#15962,#15963,#15964,#15965,#15966,#15967,#15968,#15969,#15970,#15971,#15972,
#15973,#15974,#15975,#15976,#15977,#15978,#15979,#15980,#15981,#15982,#15983,
#15984),.UNSPECIFIED.,.F.,.F.,(4,3,3,3,3,3,3,3,3,4),(-450.19908722988,-449.44490476114,
-448.690722292401,-447.936539823661,-447.182357354921,-446.428174886181,
-445.673992417442,-444.919809948702,-444.165627479962,-443.915901922701),
 .UNSPECIFIED.);
#360=B_SPLINE_CURVE_WITH_KNOTS('',3,(#15985,#15986,#15987,#15988,#15989,
#15990,#15991,#15992,#15993,#15994,#15995,#15996,#15997,#15998,#15999,#16000,
#16001,#16002,#16003,#16004,#16005,#16006,#16007,#16008,#16009,#16010,#16011,
#16012),.UNSPECIFIED.,.F.,.F.,(4,3,3,3,3,3,3,3,3,4),(440.948434008079,441.702616476819,
442.456798945559,443.210981414299,443.965163883038,444.719346351778,445.473528820518,
446.227711289257,446.981893757997,447.231619315259),.UNSPECIFIED.);
#361=B_SPLINE_CURVE_WITH_KNOTS('',3,(#16017,#16018,#16019,#16020,#16021,
#16022,#16023,#16024,#16025,#16026,#16027,#16028,#16029,#16030,#16031,#16032,
#16033,#16034,#16035,#16036,#16037,#16038,#16039,#16040,#16041,#16042,#16043,
#16044),.UNSPECIFIED.,.F.,.F.,(4,3,3,3,3,3,3,3,3,4),(-456.48227253706,-455.72809006832,
-454.97390759958,-454.219725130841,-453.465542662101,-452.711360193361,
-451.957177724622,-451.202995255882,-450.448812787142,-450.19908722988),
 .UNSPECIFIED.);
#362=B_SPLINE_CURVE_WITH_KNOTS('',3,(#16045,#16046,#16047,#16048,#16049,
#16050,#16051,#16052,#16053,#16054,#16055,#16056,#16057,#16058,#16059,#16060,
#16061,#16062,#16063,#16064,#16065,#16066,#16067,#16068,#16069,#16070,#16071,
#16072),.UNSPECIFIED.,.F.,.F.,(4,3,3,3,3,3,3,3,3,4),(447.231619315259,447.985801783999,
448.739984252738,449.494166721478,450.248349190217,451.002531658957,451.756714127697,
452.510896596436,453.265079065176,453.514804622438),.UNSPECIFIED.);
#363=B_SPLINE_CURVE_WITH_KNOTS('',3,(#16077,#16078,#16079,#16080,#16081,
#16082,#16083,#16084,#16085,#16086,#16087,#16088,#16089,#16090,#16091,#16092,
#16093,#16094,#16095,#16096,#16097,#16098,#16099,#16100,#16101,#16102,#16103,
#16104),.UNSPECIFIED.,.F.,.F.,(4,3,3,3,3,3,3,3,3,4),(-462.765457844239,
-462.0112753755,-461.25709290676,-460.50291043802,-459.74872796928,-458.99454550054,
-458.240363031801,-457.486180563061,-456.731998094321,-456.48227253706),
 .UNSPECIFIED.);
#364=B_SPLINE_CURVE_WITH_KNOTS('',3,(#16105,#16106,#16107,#16108,#16109,
#16110,#16111,#16112,#16113,#16114,#16115,#16116,#16117,#16118,#16119,#16120,
#16121,#16122,#16123,#16124,#16125,#16126,#16127,#16128,#16129,#16130,#16131,
#16132),.UNSPECIFIED.,.F.,.F.,(4,3,3,3,3,3,3,3,3,4),(453.514804622438,454.268987091178,
455.023169559918,455.777352028658,456.531534497398,457.285716966138,458.039899434877,
458.794081903617,459.548264372357,459.797989929618),.UNSPECIFIED.);
#365=B_SPLINE_CURVE_WITH_KNOTS('',3,(#16137,#16138,#16139,#16140,#16141,
#16142,#16143,#16144,#16145,#16146,#16147,#16148,#16149,#16150,#16151,#16152,
#16153,#16154,#16155,#16156,#16157,#16158,#16159,#16160,#16161,#16162,#16163,
#16164),.UNSPECIFIED.,.F.,.F.,(4,3,3,3,3,3,3,3,3,4),(-469.048643151419,
-468.294460682679,-467.54027821394,-466.7860957452,-466.03191327646,-465.277730807721,
-464.523548338981,-463.769365870241,-463.015183401502,-462.765457844239),
 .UNSPECIFIED.);
#366=B_SPLINE_CURVE_WITH_KNOTS('',3,(#16165,#16166,#16167,#16168,#16169,
#16170,#16171,#16172,#16173,#16174,#16175,#16176,#16177,#16178,#16179,#16180,
#16181,#16182,#16183,#16184,#16185,#16186,#16187,#16188,#16189,#16190,#16191,
#16192),.UNSPECIFIED.,.F.,.F.,(4,3,3,3,3,3,3,3,3,4),(459.797989929618,460.552172398358,
461.306354867097,462.060537335837,462.814719804577,463.568902273316,464.323084742056,
465.077267210796,465.831449679535,466.081175236798),.UNSPECIFIED.);
#367=B_SPLINE_CURVE_WITH_KNOTS('',3,(#16197,#16198,#16199,#16200,#16201,
#16202,#16203,#16204,#16205,#16206,#16207,#16208,#16209,#16210,#16211,#16212,
#16213,#16214,#16215,#16216,#16217,#16218,#16219,#16220,#16221,#16222,#16223,
#16224),.UNSPECIFIED.,.F.,.F.,(4,3,3,3,3,3,3,3,3,4),(-475.331828458599,
-474.577645989859,-473.823463521119,-473.069281052379,-472.31509858364,
-471.5609161149,-470.80673364616,-470.052551177421,-469.298368708681,-469.048643151419),
 .UNSPECIFIED.);
#368=B_SPLINE_CURVE_WITH_KNOTS('',3,(#16225,#16226,#16227,#16228,#16229,
#16230,#16231,#16232,#16233,#16234,#16235,#16236,#16237,#16238,#16239,#16240,
#16241,#16242,#16243,#16244,#16245,#16246,#16247,#16248,#16249,#16250,#16251,
#16252),.UNSPECIFIED.,.F.,.F.,(4,3,3,3,3,3,3,3,3,4),(466.081175236798,466.835357705537,
467.589540174277,468.343722643017,469.097905111756,469.852087580496,470.606270049236,
471.360452517975,472.114634986715,472.364360543977),.UNSPECIFIED.);
#369=B_SPLINE_CURVE_WITH_KNOTS('',3,(#16257,#16258,#16259,#16260,#16261,
#16262,#16263,#16264,#16265,#16266,#16267,#16268,#16269,#16270,#16271,#16272,
#16273,#16274,#16275,#16276,#16277,#16278,#16279,#16280,#16281,#16282,#16283,
#16284),.UNSPECIFIED.,.F.,.F.,(4,3,3,3,3,3,3,3,3,4),(-481.615013765778,
-480.860831297038,-480.106648828299,-479.352466359559,-478.598283890819,
-477.844101422079,-477.08991895334,-476.3357364846,-475.58155401586,-475.331828458599),
 .UNSPECIFIED.);
#370=B_SPLINE_CURVE_WITH_KNOTS('',3,(#16285,#16286,#16287,#16288,#16289,
#16290,#16291,#16292,#16293,#16294,#16295,#16296,#16297,#16298,#16299,#16300,
#16301,#16302,#16303,#16304,#16305,#16306,#16307,#16308,#16309,#16310,#16311,
#16312),.UNSPECIFIED.,.F.,.F.,(4,3,3,3,3,3,3,3,3,4),(472.364360543977,473.118543012717,
473.872725481457,474.626907950196,475.381090418936,476.135272887676,476.889455356416,
477.643637825155,478.397820293895,478.647545851157),.UNSPECIFIED.);
#371=B_SPLINE_CURVE_WITH_KNOTS('',3,(#16317,#16318,#16319,#16320,#16321,
#16322,#16323,#16324,#16325,#16326,#16327,#16328,#16329,#16330,#16331,#16332,
#16333,#16334,#16335,#16336,#16337,#16338,#16339,#16340,#16341,#16342,#16343,
#16344),.UNSPECIFIED.,.F.,.F.,(4,3,3,3,3,3,3,3,3,4),(-487.898199072958,
-487.144016604218,-486.389834135478,-485.635651666738,-484.881469197999,
-484.127286729259,-483.373104260519,-482.618921791779,-481.86473932304,
-481.615013765778),.UNSPECIFIED.);
#372=B_SPLINE_CURVE_WITH_KNOTS('',3,(#16345,#16346,#16347,#16348,#16349,
#16350,#16351,#16352,#16353,#16354,#16355,#16356,#16357,#16358,#16359,#16360,
#16361,#16362,#16363,#16364,#16365,#16366,#16367,#16368,#16369,#16370,#16371,
#16372),.UNSPECIFIED.,.F.,.F.,(4,3,3,3,3,3,3,3,3,4),(478.647545851157,479.401728319896,
480.155910788636,480.910093257376,481.664275726116,482.418458194855,483.172640663595,
483.926823132335,484.681005601074,484.930731158336),.UNSPECIFIED.);
#373=B_SPLINE_CURVE_WITH_KNOTS('',3,(#16377,#16378,#16379,#16380,#16381,
#16382,#16383,#16384,#16385,#16386,#16387,#16388,#16389,#16390,#16391,#16392,
#16393,#16394,#16395,#16396,#16397,#16398,#16399,#16400,#16401),
 .UNSPECIFIED.,.F.,.F.,(4,3,3,3,3,3,3,3,4),(-494.181384380137,-493.746934668774,
-492.747446946773,-491.747959224771,-491.24821536377,-490.748471502769,
-489.748983780768,-488.749496058766,-487.898199072958),.UNSPECIFIED.);
#374=B_SPLINE_CURVE_WITH_KNOTS('',3,(#16402,#16403,#16404,#16405,#16406,
#16407,#16408,#16409,#16410,#16411,#16412,#16413,#16414,#16415,#16416,#16417,
#16418,#16419,#16420,#16421,#16422,#16423,#16424,#16425,#16426,#16427,#16428,
#16429),.UNSPECIFIED.,.F.,.F.,(4,3,3,3,3,3,3,3,3,4),(484.930731158336,485.684913627076,
486.439096095816,487.193278564555,487.947461033295,488.701643502035,489.455825970775,
490.210008439514,490.964190908254,491.213916465516),.UNSPECIFIED.);
#375=B_SPLINE_CURVE_WITH_KNOTS('',3,(#16434,#16435,#16436,#16437,#16438,
#16439,#16440,#16441,#16442,#16443,#16444,#16445,#16446,#16447,#16448,#16449,
#16450,#16451,#16452,#16453,#16454,#16455,#16456,#16457,#16458,#16459,#16460,
#16461),.UNSPECIFIED.,.F.,.F.,(4,3,3,3,3,3,3,3,3,4),(-500.464569687317,
-499.710387218577,-498.956204749837,-498.202022281097,-497.447839812357,
-496.693657343618,-495.939474874878,-495.185292406138,-494.431109937398,
-494.181384380137),.UNSPECIFIED.);
#376=B_SPLINE_CURVE_WITH_KNOTS('',3,(#16462,#16463,#16464,#16465,#16466,
#16467,#16468,#16469,#16470,#16471,#16472,#16473,#16474,#16475,#16476,#16477,
#16478,#16479,#16480,#16481,#16482,#16483,#16484,#16485,#16486,#16487,#16488,
#16489),.UNSPECIFIED.,.F.,.F.,(4,3,3,3,3,3,3,3,3,4),(491.213916465516,491.968098934256,
492.722281402995,493.476463871735,494.230646340475,494.984828809214,495.739011277954,
496.493193746694,497.247376215433,497.497101772695),.UNSPECIFIED.);
#377=B_SPLINE_CURVE_WITH_KNOTS('',3,(#16494,#16495,#16496,#16497,#16498,
#16499,#16500,#16501,#16502,#16503,#16504,#16505,#16506,#16507,#16508,#16509,
#16510,#16511,#16512,#16513,#16514,#16515,#16516,#16517,#16518,#16519,#16520,
#16521),.UNSPECIFIED.,.F.,.F.,(4,3,3,3,3,3,3,3,3,4),(-506.747754994496,
-505.993572525757,-505.239390057017,-504.485207588277,-503.731025119538,
-502.976842650798,-502.222660182058,-501.468477713319,-500.714295244579,
-500.464569687317),.UNSPECIFIED.);
#378=B_SPLINE_CURVE_WITH_KNOTS('',3,(#16522,#16523,#16524,#16525,#16526,
#16527,#16528,#16529,#16530,#16531,#16532,#16533,#16534,#16535,#16536,#16537,
#16538,#16539,#16540,#16541,#16542,#16543,#16544,#16545,#16546,#16547,#16548,
#16549),.UNSPECIFIED.,.F.,.F.,(4,3,3,3,3,3,3,3,3,4),(497.497101772695,498.251284241435,
499.005466710175,499.759649178915,500.513831647655,501.268014116394,502.022196585134,
502.776379053874,503.530561522614,503.780287079875),.UNSPECIFIED.);
#379=B_SPLINE_CURVE_WITH_KNOTS('',3,(#16554,#16555,#16556,#16557,#16558,
#16559,#16560,#16561,#16562,#16563,#16564,#16565,#16566,#16567,#16568,#16569,
#16570,#16571,#16572,#16573,#16574,#16575,#16576,#16577,#16578,#16579,#16580,
#16581),.UNSPECIFIED.,.F.,.F.,(4,3,3,3,3,3,3,3,3,4),(-513.030940301676,
-512.276757832936,-511.522575364197,-510.768392895457,-510.014210426717,
-509.260027957977,-508.505845489238,-507.751663020498,-506.997480551758,
-506.747754994496),.UNSPECIFIED.);
#380=B_SPLINE_CURVE_WITH_KNOTS('',3,(#16582,#16583,#16584,#16585,#16586,
#16587,#16588,#16589,#16590,#16591,#16592,#16593,#16594,#16595,#16596,#16597,
#16598,#16599,#16600,#16601,#16602,#16603,#16604,#16605,#16606,#16607,#16608,
#16609),.UNSPECIFIED.,.F.,.F.,(4,3,3,3,3,3,3,3,3,4),(503.780287079875,504.534469548615,
505.288652017355,506.042834486094,506.797016954834,507.551199423574,508.305381892314,
509.059564361054,509.813746829794,510.063472387055),.UNSPECIFIED.);
#381=B_SPLINE_CURVE_WITH_KNOTS('',3,(#16614,#16615,#16616,#16617,#16618,
#16619,#16620,#16621,#16622,#16623,#16624,#16625,#16626,#16627,#16628,#16629,
#16630,#16631,#16632,#16633,#16634,#16635,#16636,#16637,#16638,#16639,#16640,
#16641),.UNSPECIFIED.,.F.,.F.,(4,3,3,3,3,3,3,3,3,4),(-519.314125608855,
-518.559943140116,-517.805760671376,-517.051578202637,-516.297395733897,
-515.543213265157,-514.789030796418,-514.034848327678,-513.280665858939,
-513.030940301676),.UNSPECIFIED.);
#382=B_SPLINE_CURVE_WITH_KNOTS('',3,(#16642,#16643,#16644,#16645,#16646,
#16647,#16648,#16649,#16650,#16651,#16652,#16653,#16654,#16655,#16656,#16657,
#16658,#16659,#16660,#16661,#16662,#16663,#16664,#16665,#16666,#16667,#16668,
#16669),.UNSPECIFIED.,.F.,.F.,(4,3,3,3,3,3,3,3,3,4),(510.063472387055,510.817654855794,
511.571837324534,512.326019793273,513.080202262013,513.834384730752,514.588567199492,
515.342749668232,516.096932136971,516.346657694234),.UNSPECIFIED.);
#383=B_SPLINE_CURVE_WITH_KNOTS('',3,(#16674,#16675,#16676,#16677,#16678,
#16679,#16680,#16681,#16682,#16683,#16684,#16685,#16686,#16687,#16688,#16689,
#16690,#16691,#16692,#16693,#16694,#16695,#16696,#16697,#16698,#16699,#16700,
#16701),.UNSPECIFIED.,.F.,.F.,(4,3,3,3,3,3,3,3,3,4),(-525.597310916035,
-524.843128447295,-524.088945978556,-523.334763509816,-522.580581041076,
-521.826398572337,-521.072216103597,-520.318033634857,-519.563851166117,
-519.314125608855),.UNSPECIFIED.);
#384=B_SPLINE_CURVE_WITH_KNOTS('',3,(#16702,#16703,#16704,#16705,#16706,
#16707,#16708,#16709,#16710,#16711,#16712,#16713,#16714,#16715,#16716,#16717,
#16718,#16719,#16720,#16721,#16722,#16723,#16724,#16725,#16726),
 .UNSPECIFIED.,.F.,.F.,(4,3,3,3,3,3,3,3,4),(516.346657694234,516.735152274811,
517.734639996812,518.734127718814,519.233871579814,519.733615440815,520.733103162817,
521.732590884818,522.629843001414),.UNSPECIFIED.);
#385=B_SPLINE_CURVE_WITH_KNOTS('',3,(#16731,#16732,#16733,#16734,#16735,
#16736,#16737,#16738,#16739,#16740,#16741,#16742,#16743,#16744,#16745,#16746,
#16747,#16748,#16749,#16750,#16751,#16752,#16753,#16754,#16755,#16756,#16757,
#16758),.UNSPECIFIED.,.F.,.F.,(4,3,3,3,3,3,3,3,3,4),(-531.880496223215,
-531.126313754475,-530.372131285735,-529.617948816995,-528.863766348255,
-528.109583879515,-527.355401410776,-526.601218942036,-525.847036473296,
-525.597310916035),.UNSPECIFIED.);
#386=B_SPLINE_CURVE_WITH_KNOTS('',3,(#16759,#16760,#16761,#16762,#16763,
#16764,#16765,#16766,#16767,#16768,#16769,#16770,#16771,#16772,#16773,#16774,
#16775,#16776,#16777,#16778,#16779,#16780,#16781,#16782,#16783,#16784,#16785,
#16786),.UNSPECIFIED.,.F.,.F.,(4,3,3,3,3,3,3,3,3,4),(522.629843001414,523.384025470153,
524.138207938893,524.892390407633,525.646572876373,526.400755345113,527.154937813853,
527.909120282592,528.663302751332,528.913028308593),.UNSPECIFIED.);
#387=B_SPLINE_CURVE_WITH_KNOTS('',3,(#16791,#16792,#16793,#16794,#16795,
#16796,#16797,#16798,#16799,#16800,#16801,#16802,#16803,#16804,#16805,#16806,
#16807,#16808,#16809,#16810,#16811,#16812,#16813,#16814,#16815,#16816,#16817,
#16818),.UNSPECIFIED.,.F.,.F.,(4,3,3,3,3,3,3,3,3,4),(-538.163681530394,
-537.409499061655,-536.655316592915,-535.901134124175,-535.146951655435,
-534.392769186696,-533.638586717956,-532.884404249216,-532.130221780477,
-531.880496223215),.UNSPECIFIED.);
#388=B_SPLINE_CURVE_WITH_KNOTS('',3,(#16819,#16820,#16821,#16822,#16823,
#16824,#16825,#16826,#16827,#16828,#16829,#16830,#16831,#16832,#16833,#16834,
#16835,#16836,#16837,#16838,#16839,#16840,#16841,#16842,#16843,#16844,#16845,
#16846),.UNSPECIFIED.,.F.,.F.,(4,3,3,3,3,3,3,3,3,4),(528.913028308593,529.667210777333,
530.421393246073,531.175575714812,531.929758183552,532.683940652292,533.438123121032,
534.192305589771,534.946488058511,535.196213615773),.UNSPECIFIED.);
#389=B_SPLINE_CURVE_WITH_KNOTS('',3,(#16851,#16852,#16853,#16854,#16855,
#16856,#16857,#16858,#16859,#16860,#16861,#16862,#16863,#16864,#16865,#16866,
#16867,#16868,#16869,#16870,#16871,#16872,#16873,#16874,#16875,#16876,#16877,
#16878),.UNSPECIFIED.,.F.,.F.,(4,3,3,3,3,3,3,3,3,4),(-544.446866837574,
-543.692684368834,-542.938501900094,-542.184319431355,-541.430136962615,
-540.675954493875,-539.921772025136,-539.167589556396,-538.413407087656,
-538.163681530394),.UNSPECIFIED.);
#390=B_SPLINE_CURVE_WITH_KNOTS('',3,(#16879,#16880,#16881,#16882,#16883,
#16884,#16885,#16886,#16887,#16888,#16889,#16890,#16891,#16892,#16893,#16894,
#16895,#16896,#16897,#16898,#16899,#16900,#16901,#16902,#16903,#16904,#16905,
#16906),.UNSPECIFIED.,.F.,.F.,(4,3,3,3,3,3,3,3,3,4),(535.196213615773,535.950396084513,
536.704578553252,537.458761021992,538.212943490732,538.967125959471,539.721308428211,
540.475490896951,541.229673365691,541.479398922952),.UNSPECIFIED.);
#391=B_SPLINE_CURVE_WITH_KNOTS('',3,(#16911,#16912,#16913,#16914,#16915,
#16916,#16917,#16918,#16919,#16920,#16921,#16922,#16923,#16924,#16925,#16926,
#16927,#16928,#16929,#16930,#16931,#16932,#16933,#16934,#16935,#16936,#16937,
#16938),.UNSPECIFIED.,.F.,.F.,(4,3,3,3,3,3,3,3,3,4),(-550.730052144753,
-549.975869676014,-549.221687207274,-548.467504738534,-547.713322269795,
-546.959139801055,-546.204957332315,-545.450774863575,-544.696592394836,
-544.446866837574),.UNSPECIFIED.);
#392=B_SPLINE_CURVE_WITH_KNOTS('',3,(#16939,#16940,#16941,#16942,#16943,
#16944,#16945,#16946,#16947,#16948,#16949,#16950,#16951,#16952,#16953,#16954,
#16955,#16956,#16957,#16958,#16959,#16960,#16961,#16962,#16963,#16964,#16965,
#16966),.UNSPECIFIED.,.F.,.F.,(4,3,3,3,3,3,3,3,3,4),(541.479398922952,542.233581391692,
542.987763860432,543.741946329171,544.496128797911,545.250311266651,546.004493735391,
546.75867620413,547.51285867287,547.762584230132),.UNSPECIFIED.);
#393=B_SPLINE_CURVE_WITH_KNOTS('',3,(#16971,#16972,#16973,#16974,#16975,
#16976,#16977,#16978,#16979,#16980,#16981,#16982,#16983,#16984,#16985,#16986,
#16987,#16988,#16989,#16990,#16991,#16992,#16993,#16994,#16995,#16996,#16997,
#16998),.UNSPECIFIED.,.F.,.F.,(4,3,3,3,3,3,3,3,3,4),(-557.013237451933,
-556.259054983193,-555.504872514453,-554.750690045713,-553.996507576973,
-553.242325108234,-552.488142639494,-551.733960170754,-550.979777702014,
-550.730052144753),.UNSPECIFIED.);
#394=B_SPLINE_CURVE_WITH_KNOTS('',3,(#16999,#17000,#17001,#17002,#17003,
#17004,#17005,#17006,#17007,#17008,#17009,#17010,#17011,#17012,#17013,#17014,
#17015,#17016,#17017,#17018,#17019,#17020,#17021,#17022,#17023,#17024,#17025,
#17026),.UNSPECIFIED.,.F.,.F.,(4,3,3,3,3,3,3,3,3,4),(547.762584230132,548.516766698872,
549.270949167611,550.025131636351,550.779314105091,551.533496573831,552.28767904257,
553.04186151131,553.79604398005,554.045769537312),.UNSPECIFIED.);
#395=B_SPLINE_CURVE_WITH_KNOTS('',3,(#17031,#17032,#17033,#17034,#17035,
#17036,#17037,#17038,#17039,#17040,#17041,#17042,#17043,#17044,#17045,#17046,
#17047,#17048,#17049,#17050,#17051,#17052,#17053,#17054,#17055,#17056,#17057,
#17058),.UNSPECIFIED.,.F.,.F.,(4,3,3,3,3,3,3,3,3,4),(-563.296422759112,
-562.542240290373,-561.788057821633,-561.033875352894,-560.279692884154,
-559.525510415414,-558.771327946675,-558.017145477935,-557.262963009196,
-557.013237451933),.UNSPECIFIED.);
#396=B_SPLINE_CURVE_WITH_KNOTS('',3,(#17059,#17060,#17061,#17062,#17063,
#17064,#17065,#17066,#17067,#17068,#17069,#17070,#17071,#17072,#17073,#17074,
#17075,#17076,#17077,#17078,#17079,#17080,#17081,#17082,#17083,#17084,#17085,
#17086),.UNSPECIFIED.,.F.,.F.,(4,3,3,3,3,3,3,3,3,4),(554.045769537312,554.799952006051,
555.554134474791,556.308316943531,557.062499412271,557.816681881011,558.570864349751,
559.32504681849,560.07922928723,560.328954844491),.UNSPECIFIED.);
#397=B_SPLINE_CURVE_WITH_KNOTS('',3,(#17091,#17092,#17093,#17094,#17095,
#17096,#17097,#17098,#17099,#17100,#17101,#17102,#17103,#17104,#17105,#17106,
#17107,#17108,#17109,#17110,#17111,#17112,#17113,#17114,#17115,#17116,#17117,
#17118),.UNSPECIFIED.,.F.,.F.,(4,3,3,3,3,3,3,3,3,4),(-569.579608066292,
-568.825425597552,-568.071243128813,-567.317060660073,-566.562878191334,
-565.808695722594,-565.054513253854,-564.300330785115,-563.546148316375,
-563.296422759112),.UNSPECIFIED.);
#398=B_SPLINE_CURVE_WITH_KNOTS('',3,(#17119,#17120,#17121,#17122,#17123,
#17124,#17125,#17126,#17127,#17128,#17129,#17130,#17131,#17132,#17133,#17134,
#17135,#17136,#17137,#17138,#17139,#17140,#17141,#17142,#17143,#17144,#17145,
#17146),.UNSPECIFIED.,.F.,.F.,(4,3,3,3,3,3,3,3,3,4),(560.328954844491,561.083137313231,
561.837319781971,562.59150225071,563.34568471945,564.09986718819,564.854049656929,
565.608232125669,566.362414594409,566.612140151671),.UNSPECIFIED.);
#399=B_SPLINE_CURVE_WITH_KNOTS('',3,(#17151,#17152,#17153,#17154,#17155,
#17156,#17157,#17158,#17159,#17160,#17161,#17162,#17163,#17164,#17165,#17166,
#17167,#17168,#17169,#17170,#17171,#17172,#17173,#17174,#17175,#17176,#17177,
#17178),.UNSPECIFIED.,.F.,.F.,(4,3,3,3,3,3,3,3,3,4),(-575.862793373472,
-575.108610904732,-574.354428435992,-573.600245967253,-572.846063498513,
-572.091881029774,-571.337698561034,-570.583516092294,-569.829333623555,
-569.579608066292),.UNSPECIFIED.);
#400=B_SPLINE_CURVE_WITH_KNOTS('',3,(#17179,#17180,#17181,#17182,#17183,
#17184,#17185,#17186,#17187,#17188,#17189,#17190,#17191,#17192,#17193,#17194,
#17195,#17196,#17197,#17198,#17199,#17200,#17201,#17202,#17203,#17204,#17205,
#17206),.UNSPECIFIED.,.F.,.F.,(4,3,3,3,3,3,3,3,3,4),(566.612140151671,567.36632262041,
568.12050508915,568.87468755789,569.62887002663,570.383052495369,571.137234964109,
571.891417432849,572.645599901588,572.89532545885),.UNSPECIFIED.);
#401=B_SPLINE_CURVE_WITH_KNOTS('',3,(#17211,#17212,#17213,#17214,#17215,
#17216,#17217,#17218,#17219,#17220,#17221,#17222,#17223,#17224,#17225,#17226,
#17227,#17228,#17229,#17230,#17231,#17232,#17233,#17234,#17235,#17236,#17237,
#17238),.UNSPECIFIED.,.F.,.F.,(4,3,3,3,3,3,3,3,3,4),(-582.145978680651,
-581.391796211912,-580.637613743172,-579.883431274432,-579.129248805693,
-578.375066336953,-577.620883868214,-576.866701399474,-576.112518930734,
-575.862793373472),.UNSPECIFIED.);
#402=B_SPLINE_CURVE_WITH_KNOTS('',3,(#17239,#17240,#17241,#17242,#17243,
#17244,#17245,#17246,#17247,#17248,#17249,#17250,#17251,#17252,#17253,#17254,
#17255,#17256,#17257,#17258,#17259,#17260,#17261,#17262,#17263,#17264,#17265,
#17266),.UNSPECIFIED.,.F.,.F.,(4,3,3,3,3,3,3,3,3,4),(572.89532545885,573.64950792759,
574.40369039633,575.157872865069,575.912055333809,576.666237802549,577.420420271289,
578.174602740028,578.928785208768,579.17851076603),.UNSPECIFIED.);
#403=B_SPLINE_CURVE_WITH_KNOTS('',3,(#17271,#17272,#17273,#17274,#17275,
#17276,#17277,#17278,#17279,#17280,#17281,#17282,#17283,#17284,#17285,#17286,
#17287,#17288,#17289,#17290,#17291,#17292,#17293,#17294,#17295,#17296,#17297,
#17298),.UNSPECIFIED.,.F.,.F.,(4,3,3,3,3,3,3,3,3,4),(-588.429163987831,
-587.674981519091,-586.920799050352,-586.166616581612,-585.412434112872,
-584.658251644133,-583.904069175393,-583.149886706654,-582.395704237914,
-582.145978680651),.UNSPECIFIED.);
#404=B_SPLINE_CURVE_WITH_KNOTS('',3,(#17299,#17300,#17301,#17302,#17303,
#17304,#17305,#17306,#17307,#17308,#17309,#17310,#17311,#17312,#17313,#17314,
#17315,#17316,#17317,#17318,#17319,#17320,#17321,#17322,#17323),
 .UNSPECIFIED.,.F.,.F.,(4,3,3,3,3,3,3,3,4),(579.17851076603,579.702878760909,
580.702366482911,581.701854204912,582.201598065913,582.701341926914,583.700829648916,
584.700317370917,585.461696073209),.UNSPECIFIED.);
#405=B_SPLINE_CURVE_WITH_KNOTS('',3,(#17329,#17330,#17331,#17332,#17333,
#17334,#17335,#17336,#17337,#17338),.UNSPECIFIED.,.F.,.F.,(4,3,3,4),(600.04419683565,
600.828396999699,601.612597163748,602.234451722701),.UNSPECIFIED.);
#406=B_SPLINE_CURVE_WITH_KNOTS('',3,(#17341,#17342,#17343,#17344,#17345),
 .UNSPECIFIED.,.F.,.F.,(4,1,4),(600.04419683565,600.495790741192,600.995534602193),
 .UNSPECIFIED.);
#407=B_SPLINE_CURVE_WITH_KNOTS('',3,(#17350,#17351,#17352,#17353,#17354,
#17355,#17356,#17357,#17358,#17359,#17360,#17361,#17362,#17363,#17364,#17365,
#17366,#17367,#17368,#17369,#17370,#17371,#17372,#17373,#17374,#17375,#17376,
#17377),.UNSPECIFIED.,.F.,.F.,(4,3,3,3,3,3,3,3,3,4),(593.761011528471,594.54521169252,
595.329411856569,596.113612020618,596.897812184667,597.682012348716,598.466212512766,
599.250412676815,600.034612840864,600.04419683565),.UNSPECIFIED.);
#408=B_SPLINE_CURVE_WITH_KNOTS('',3,(#17378,#17379,#17380,#17381,#17382,
#17383,#17384,#17385,#17386,#17387,#17388,#17389,#17390,#17391,#17392,#17393,
#17394,#17395,#17396,#17397,#17398,#17399,#17400,#17401,#17402,#17403,#17404,
#17405),.UNSPECIFIED.,.F.,.F.,(4,3,3,3,3,3,3,3,3,4),(593.761011528471,594.54521169252,
595.329411856569,596.113612020618,596.897812184667,597.682012348717,598.466212512766,
599.250412676815,600.034612840864,600.04419683565),.UNSPECIFIED.);
#409=B_SPLINE_CURVE_WITH_KNOTS('',3,(#17410,#17411,#17412,#17413,#17414,
#17415,#17416,#17417,#17418,#17419,#17420,#17421,#17422,#17423,#17424,#17425,
#17426,#17427,#17428,#17429,#17430,#17431,#17432,#17433,#17434,#17435,#17436,
#17437),.UNSPECIFIED.,.F.,.F.,(4,3,3,3,3,3,3,3,3,4),(587.477826221291,588.26202638534,
589.046226549389,589.830426713438,590.614626877487,591.398827041536,592.183027205585,
592.967227369634,593.751427533683,593.761011528471),.UNSPECIFIED.);
#410=B_SPLINE_CURVE_WITH_KNOTS('',3,(#17438,#17439,#17440,#17441,#17442,
#17443,#17444,#17445,#17446,#17447,#17448,#17449,#17450,#17451,#17452,#17453,
#17454,#17455,#17456,#17457,#17458,#17459,#17460,#17461,#17462),
 .UNSPECIFIED.,.F.,.F.,(4,3,3,3,3,3,3,3,4),(587.477826221291,588.002194216173,
589.001681938174,590.001169660176,590.500913521176,591.000657382177,592.000145104179,
592.99963282618,593.761011528471),.UNSPECIFIED.);
#411=B_SPLINE_CURVE_WITH_KNOTS('',3,(#17467,#17468,#17469,#17470,#17471,
#17472,#17473,#17474,#17475,#17476,#17477,#17478,#17479,#17480,#17481,#17482,
#17483,#17484,#17485,#17486,#17487,#17488,#17489,#17490,#17491,#17492,#17493,
#17494),.UNSPECIFIED.,.F.,.F.,(4,3,3,3,3,3,3,3,3,4),(581.194640914112,581.978841078161,
582.76304124221,583.54724140626,584.331441570309,585.115641734358,585.899841898408,
586.684042062457,587.468242226507,587.477826221291),.UNSPECIFIED.);
#412=B_SPLINE_CURVE_WITH_KNOTS('',3,(#17495,#17496,#17497,#17498,#17499,
#17500,#17501,#17502,#17503,#17504,#17505,#17506,#17507,#17508,#17509,#17510,
#17511,#17512,#17513,#17514,#17515,#17516,#17517,#17518,#17519,#17520,#17521,
#17522),.UNSPECIFIED.,.F.,.F.,(4,3,3,3,3,3,3,3,3,4),(581.194640914112,581.978841078161,
582.763041242211,583.54724140626,584.331441570309,585.115641734359,585.899841898408,
586.684042062457,587.468242226507,587.477826221291),.UNSPECIFIED.);
#413=B_SPLINE_CURVE_WITH_KNOTS('',3,(#17527,#17528,#17529,#17530,#17531,
#17532,#17533,#17534,#17535,#17536,#17537,#17538,#17539,#17540,#17541,#17542,
#17543,#17544,#17545,#17546,#17547,#17548,#17549,#17550,#17551,#17552,#17553,
#17554),.UNSPECIFIED.,.F.,.F.,(4,3,3,3,3,3,3,3,3,4),(574.911455606932,575.695655770981,
576.47985593503,577.264056099079,578.048256263128,578.832456427178,579.616656591227,
580.400856755276,581.185056919325,581.194640914112),.UNSPECIFIED.);
#414=B_SPLINE_CURVE_WITH_KNOTS('',3,(#17555,#17556,#17557,#17558,#17559,
#17560,#17561,#17562,#17563,#17564,#17565,#17566,#17567,#17568,#17569,#17570,
#17571,#17572,#17573,#17574,#17575,#17576,#17577,#17578,#17579,#17580,#17581,
#17582),.UNSPECIFIED.,.F.,.F.,(4,3,3,3,3,3,3,3,3,4),(574.911455606932,575.695655770981,
576.479855935031,577.26405609908,578.048256263129,578.832456427178,579.616656591227,
580.400856755276,581.185056919325,581.194640914112),.UNSPECIFIED.);
#415=B_SPLINE_CURVE_WITH_KNOTS('',3,(#17587,#17588,#17589,#17590,#17591,
#17592,#17593,#17594,#17595,#17596,#17597,#17598,#17599,#17600,#17601,#17602,
#17603,#17604,#17605,#17606,#17607,#17608,#17609,#17610,#17611,#17612,#17613,
#17614),.UNSPECIFIED.,.F.,.F.,(4,3,3,3,3,3,3,3,3,4),(568.628270299752,569.412470463802,
570.196670627851,570.9808707919,571.765070955949,572.549271119999,573.333471284048,
574.117671448097,574.901871612146,574.911455606932),.UNSPECIFIED.);
#416=B_SPLINE_CURVE_WITH_KNOTS('',3,(#17615,#17616,#17617,#17618,#17619,
#17620,#17621,#17622,#17623,#17624,#17625),.UNSPECIFIED.,.F.,.F.,(4,1,1,
1,1,1,1,1,4),(568.628270299753,569.011927498143,569.511671359144,570.011415220144,
571.010902942146,572.010390664148,573.009878386149,574.009366108151,574.911455606932),
 .UNSPECIFIED.);
#417=B_SPLINE_CURVE_WITH_KNOTS('',3,(#17630,#17631,#17632,#17633,#17634,
#17635,#17636,#17637,#17638,#17639,#17640),.UNSPECIFIED.,.F.,.F.,(4,1,1,
1,1,1,1,1,4),(562.345084992573,563.332255392685,564.331743114686,565.331230836688,
565.830974697689,566.33071855869,567.330206280691,568.329694002693,568.628270299752),
 .UNSPECIFIED.);
#418=B_SPLINE_CURVE_WITH_KNOTS('',3,(#17641,#17642,#17643,#17644,#17645,
#17646,#17647,#17648,#17649,#17650,#17651,#17652,#17653,#17654,#17655,#17656,
#17657,#17658,#17659,#17660,#17661,#17662,#17663,#17664,#17665,#17666,#17667,
#17668),.UNSPECIFIED.,.F.,.F.,(4,3,3,3,3,3,3,3,3,4),(562.345084992573,563.129285156622,
563.913485320671,564.69768548472,565.48188564877,566.266085812819,567.050285976868,
567.834486140917,568.618686304966,568.628270299753),.UNSPECIFIED.);
#419=B_SPLINE_CURVE_WITH_KNOTS('',3,(#17673,#17674,#17675,#17676,#17677,
#17678,#17679,#17680,#17681,#17682,#17683,#17684,#17685,#17686,#17687,#17688,
#17689,#17690,#17691,#17692,#17693,#17694,#17695,#17696,#17697,#17698,#17699,
#17700),.UNSPECIFIED.,.F.,.F.,(4,3,3,3,3,3,3,3,3,4),(556.061899685393,556.846099849442,
557.630300013492,558.414500177541,559.19870034159,559.982900505639,560.767100669689,
561.551300833738,562.335500997787,562.345084992573),.UNSPECIFIED.);
#420=B_SPLINE_CURVE_WITH_KNOTS('',3,(#17701,#17702,#17703,#17704,#17705,
#17706,#17707,#17708,#17709,#17710),.UNSPECIFIED.,.F.,.F.,(4,1,1,1,1,1,
1,4),(556.061899685393,557.018074834124,558.017562556126,559.017050278127,
560.016538000129,561.01602572213,562.015513444132,562.345084992573),
 .UNSPECIFIED.);
#421=B_SPLINE_CURVE_WITH_KNOTS('',3,(#17715,#17716,#17717,#17718,#17719,
#17720,#17721,#17722,#17723,#17724,#17725,#17726,#17727,#17728,#17729,#17730,
#17731,#17732,#17733,#17734,#17735,#17736,#17737,#17738,#17739,#17740,#17741,
#17742),.UNSPECIFIED.,.F.,.F.,(4,3,3,3,3,3,3,3,3,4),(549.778714378214,550.562914542263,
551.347114706312,552.131314870362,552.915515034411,553.699715198461,554.48391536251,
555.268115526559,556.052315690609,556.061899685393),.UNSPECIFIED.);
#422=B_SPLINE_CURVE_WITH_KNOTS('',3,(#17743,#17744,#17745,#17746,#17747,
#17748,#17749,#17750,#17751,#17752,#17753,#17754,#17755,#17756,#17757,#17758,
#17759,#17760,#17761,#17762,#17763,#17764,#17765,#17766,#17767,#17768,#17769,
#17770),.UNSPECIFIED.,.F.,.F.,(4,3,3,3,3,3,3,3,3,4),(549.778714378214,550.562914542263,
551.347114706312,552.131314870362,552.915515034411,553.69971519846,554.483915362509,
555.268115526559,556.052315690608,556.061899685393),.UNSPECIFIED.);
#423=B_SPLINE_CURVE_WITH_KNOTS('',3,(#17775,#17776,#17777,#17778,#17779,
#17780,#17781,#17782,#17783,#17784,#17785,#17786,#17787,#17788,#17789,#17790,
#17791,#17792,#17793,#17794,#17795,#17796,#17797,#17798,#17799,#17800,#17801,
#17802),.UNSPECIFIED.,.F.,.F.,(4,3,3,3,3,3,3,3,3,4),(543.495529071034,544.279729235084,
545.063929399133,545.848129563182,546.632329727232,547.416529891281,548.20073005533,
548.98493021938,549.769130383429,549.778714378214),.UNSPECIFIED.);
#424=B_SPLINE_CURVE_WITH_KNOTS('',3,(#17803,#17804,#17805,#17806,#17807,
#17808,#17809,#17810,#17811,#17812,#17813,#17814,#17815,#17816,#17817,#17818,
#17819,#17820,#17821,#17822,#17823,#17824,#17825,#17826,#17827,#17828,#17829,
#17830),.UNSPECIFIED.,.F.,.F.,(4,3,3,3,3,3,3,3,3,4),(543.495529071034,544.279729235084,
545.063929399133,545.848129563183,546.632329727232,547.416529891281,548.200730055331,
548.98493021938,549.769130383429,549.778714378214),.UNSPECIFIED.);
#425=B_SPLINE_CURVE_WITH_KNOTS('',3,(#17835,#17836,#17837,#17838,#17839,
#17840,#17841,#17842,#17843,#17844,#17845,#17846,#17847,#17848,#17849,#17850,
#17851,#17852,#17853,#17854,#17855,#17856,#17857,#17858,#17859,#17860,#17861,
#17862),.UNSPECIFIED.,.F.,.F.,(4,3,3,3,3,3,3,3,3,4),(537.212343763855,537.996543927904,
538.780744091952,539.564944256001,540.34914442005,541.133344584099,541.917544748148,
542.701744912197,543.485945076246,543.495529071034),.UNSPECIFIED.);
#426=B_SPLINE_CURVE_WITH_KNOTS('',3,(#17863,#17864,#17865,#17866,#17867,
#17868,#17869,#17870,#17871,#17872,#17873,#17874,#17875,#17876,#17877,#17878,
#17879,#17880,#17881,#17882,#17883,#17884,#17885,#17886,#17887,#17888,#17889,
#17890),.UNSPECIFIED.,.F.,.F.,(4,3,3,3,3,3,3,3,3,4),(537.212343763855,537.996543927904,
538.780744091953,539.564944256002,540.349144420051,541.1333445841,541.917544748149,
542.701744912198,543.485945076247,543.495529071034),.UNSPECIFIED.);
#427=B_SPLINE_CURVE_WITH_KNOTS('',3,(#17895,#17896,#17897,#17898,#17899,
#17900,#17901,#17902,#17903,#17904,#17905,#17906,#17907,#17908,#17909,#17910,
#17911,#17912,#17913,#17914,#17915,#17916,#17917,#17918,#17919,#17920,#17921,
#17922),.UNSPECIFIED.,.F.,.F.,(4,3,3,3,3,3,3,3,3,4),(530.929158456675,531.713358620724,
532.497558784773,533.281758948822,534.065959112871,534.85015927692,535.634359440969,
536.418559605018,537.202759769067,537.212343763855),.UNSPECIFIED.);
#428=B_SPLINE_CURVE_WITH_KNOTS('',3,(#17923,#17924,#17925,#17926,#17927,
#17928,#17929,#17930,#17931,#17932,#17933,#17934,#17935,#17936,#17937,#17938,
#17939,#17940,#17941,#17942,#17943,#17944,#17945,#17946,#17947,#17948,#17949,
#17950),.UNSPECIFIED.,.F.,.F.,(4,3,3,3,3,3,3,3,3,4),(530.929158456675,531.713358620725,
532.497558784774,533.281758948823,534.065959112872,534.850159276922,535.634359440971,
536.41855960502,537.202759769069,537.212343763855),.UNSPECIFIED.);
#429=B_SPLINE_CURVE_WITH_KNOTS('',3,(#17955,#17956,#17957,#17958,#17959,
#17960,#17961,#17962,#17963,#17964,#17965,#17966,#17967,#17968,#17969,#17970,
#17971,#17972,#17973,#17974,#17975,#17976,#17977,#17978,#17979,#17980,#17981,
#17982),.UNSPECIFIED.,.F.,.F.,(4,3,3,3,3,3,3,3,3,4),(524.645973149495,525.430173313545,
526.214373477594,526.998573641643,527.782773805692,528.566973969742,529.351174133791,
530.13537429784,530.91957446189,530.929158456675),.UNSPECIFIED.);
#430=B_SPLINE_CURVE_WITH_KNOTS('',3,(#17983,#17984,#17985,#17986,#17987,
#17988,#17989,#17990,#17991,#17992,#17993),.UNSPECIFIED.,.F.,.F.,(4,1,1,
1,1,1,1,1,4),(524.645973149496,525.034467730074,526.033955452075,527.033443174077,
527.533187035078,528.032930896078,529.03241861808,530.031906340082,530.929158456675),
 .UNSPECIFIED.);
#431=B_SPLINE_CURVE_WITH_KNOTS('',3,(#17998,#17999,#18000,#18001,#18002,
#18003,#18004,#18005,#18006,#18007,#18008,#18009,#18010,#18011,#18012,#18013,
#18014,#18015,#18016,#18017,#18018,#18019,#18020,#18021,#18022,#18023,#18024,
#18025),.UNSPECIFIED.,.F.,.F.,(4,3,3,3,3,3,3,3,3,4),(518.362787842316,519.146988006365,
519.931188170414,520.715388334463,521.499588498512,522.283788662561,523.06798882661,
523.852188990659,524.636389154708,524.645973149495),.UNSPECIFIED.);
#432=B_SPLINE_CURVE_WITH_KNOTS('',3,(#18026,#18027,#18028,#18029,#18030,
#18031,#18032,#18033,#18034,#18035,#18036,#18037,#18038,#18039,#18040,#18041,
#18042,#18043,#18044,#18045,#18046,#18047,#18048,#18049,#18050,#18051,#18052,
#18053),.UNSPECIFIED.,.F.,.F.,(4,3,3,3,3,3,3,3,3,4),(518.362787842316,519.146988006365,
519.931188170415,520.715388334464,521.499588498513,522.283788662562,523.067988826612,
523.852188990661,524.63638915471,524.645973149496),.UNSPECIFIED.);
#433=B_SPLINE_CURVE_WITH_KNOTS('',3,(#18058,#18059,#18060,#18061,#18062,
#18063,#18064,#18065,#18066,#18067,#18068,#18069,#18070,#18071,#18072,#18073,
#18074,#18075,#18076,#18077,#18078,#18079,#18080,#18081,#18082,#18083,#18084,
#18085),.UNSPECIFIED.,.F.,.F.,(4,3,3,3,3,3,3,3,3,4),(512.079602535136,512.863802699186,
513.648002863235,514.432203027284,515.216403191333,516.000603355383,516.784803519432,
517.569003683481,518.35320384753,518.362787842316),.UNSPECIFIED.);
#434=B_SPLINE_CURVE_WITH_KNOTS('',3,(#18086,#18087,#18088,#18089,#18090,
#18091,#18092,#18093,#18094,#18095,#18096,#18097,#18098,#18099,#18100,#18101,
#18102,#18103,#18104,#18105,#18106,#18107,#18108,#18109,#18110,#18111,#18112,
#18113),.UNSPECIFIED.,.F.,.F.,(4,3,3,3,3,3,3,3,3,4),(512.079602535137,512.863802699186,
513.648002863235,514.432203027285,515.216403191334,516.000603355383,516.784803519433,
517.569003683482,518.353203847532,518.362787842316),.UNSPECIFIED.);
#435=B_SPLINE_CURVE_WITH_KNOTS('',3,(#18118,#18119,#18120,#18121,#18122,
#18123,#18124,#18125,#18126,#18127,#18128,#18129,#18130,#18131,#18132,#18133,
#18134,#18135,#18136,#18137,#18138,#18139,#18140,#18141,#18142,#18143,#18144,
#18145),.UNSPECIFIED.,.F.,.F.,(4,3,3,3,3,3,3,3,3,4),(505.796417227957,506.580617392006,
507.364817556055,508.149017720104,508.933217884153,509.717418048202,510.501618212252,
511.285818376301,512.07001854035,512.079602535136),.UNSPECIFIED.);
#436=B_SPLINE_CURVE_WITH_KNOTS('',3,(#18146,#18147,#18148,#18149,#18150,
#18151,#18152,#18153,#18154,#18155,#18156,#18157,#18158,#18159,#18160,#18161,
#18162,#18163,#18164,#18165,#18166,#18167,#18168,#18169,#18170,#18171,#18172,
#18173),.UNSPECIFIED.,.F.,.F.,(4,3,3,3,3,3,3,3,3,4),(505.796417227957,506.580617392006,
507.364817556056,508.149017720105,508.933217884154,509.717418048203,510.501618212253,
511.285818376302,512.070018540351,512.079602535137),.UNSPECIFIED.);
#437=B_SPLINE_CURVE_WITH_KNOTS('',3,(#18178,#18179,#18180,#18181,#18182,
#18183,#18184,#18185,#18186,#18187,#18188),.UNSPECIFIED.,.F.,.F.,(4,1,1,
1,1,1,1,1,4),(499.513231920777,500.364528906586,501.364016628588,502.363504350589,
502.86324821159,503.362992072591,504.362479794592,505.361967516594,505.796417227957),
 .UNSPECIFIED.);
#438=B_SPLINE_CURVE_WITH_KNOTS('',3,(#18189,#18190,#18191,#18192,#18193,
#18194,#18195,#18196,#18197,#18198,#18199,#18200,#18201,#18202,#18203,#18204,
#18205,#18206,#18207,#18208,#18209,#18210,#18211,#18212,#18213,#18214,#18215,
#18216),.UNSPECIFIED.,.F.,.F.,(4,3,3,3,3,3,3,3,3,4),(499.513231920777,500.297432084827,
501.081632248876,501.865832412925,502.650032576974,503.434232741023,504.218432905073,
505.002633069122,505.786833233171,505.796417227957),.UNSPECIFIED.);
#439=B_SPLINE_CURVE_WITH_KNOTS('',3,(#18221,#18222,#18223,#18224,#18225,
#18226,#18227,#18228,#18229,#18230,#18231,#18232,#18233,#18234,#18235,#18236,
#18237,#18238,#18239,#18240,#18241,#18242,#18243,#18244,#18245,#18246,#18247,
#18248),.UNSPECIFIED.,.F.,.F.,(4,3,3,3,3,3,3,3,3,4),(493.230046613598,494.014246777647,
494.798446941696,495.582647105745,496.366847269795,497.151047433844,497.935247597893,
498.719447761942,499.503647925992,499.513231920777),.UNSPECIFIED.);
#440=B_SPLINE_CURVE_WITH_KNOTS('',3,(#18249,#18250,#18251,#18252,#18253,
#18254,#18255,#18256,#18257,#18258,#18259,#18260,#18261,#18262,#18263,#18264,
#18265,#18266,#18267,#18268,#18269,#18270,#18271,#18272,#18273,#18274,#18275,
#18276),.UNSPECIFIED.,.F.,.F.,(4,3,3,3,3,3,3,3,3,4),(493.230046613598,494.014246777647,
494.798446941696,495.582647105745,496.366847269794,497.151047433844,497.935247597893,
498.719447761942,499.503647925991,499.513231920777),.UNSPECIFIED.);
#441=B_SPLINE_CURVE_WITH_KNOTS('',3,(#18281,#18282,#18283,#18284,#18285,
#18286,#18287,#18288,#18289,#18290,#18291,#18292,#18293,#18294,#18295,#18296,
#18297,#18298,#18299,#18300,#18301,#18302,#18303,#18304,#18305,#18306,#18307,
#18308),.UNSPECIFIED.,.F.,.F.,(4,3,3,3,3,3,3,3,3,4),(486.946861306418,487.731061470467,
488.515261634516,489.299461798566,490.083661962615,490.867862126664,491.652062290713,
492.436262454762,493.220462618811,493.230046613598),.UNSPECIFIED.);
#442=B_SPLINE_CURVE_WITH_KNOTS('',3,(#18309,#18310,#18311,#18312,#18313,
#18314,#18315,#18316,#18317,#18318,#18319,#18320,#18321,#18322,#18323,#18324,
#18325,#18326,#18327,#18328,#18329,#18330,#18331,#18332,#18333,#18334,#18335,
#18336),.UNSPECIFIED.,.F.,.F.,(4,3,3,3,3,3,3,3,3,4),(486.946861306418,487.731061470467,
488.515261634517,489.299461798566,490.083661962615,490.867862126664,491.652062290713,
492.436262454762,493.220462618811,493.230046613598),.UNSPECIFIED.);
#443=B_SPLINE_CURVE_WITH_KNOTS('',3,(#18341,#18342,#18343,#18344,#18345,
#18346,#18347,#18348,#18349,#18350,#18351,#18352,#18353,#18354,#18355,#18356,
#18357,#18358,#18359,#18360,#18361,#18362,#18363,#18364,#18365,#18366,#18367,
#18368),.UNSPECIFIED.,.F.,.F.,(4,3,3,3,3,3,3,3,3,4),(480.663675999239,481.447876163288,
482.232076327337,483.016276491386,483.800476655435,484.584676819484,485.368876983533,
486.153077147583,486.937277311632,486.946861306418),.UNSPECIFIED.);
#444=B_SPLINE_CURVE_WITH_KNOTS('',3,(#18369,#18370,#18371,#18372,#18373,
#18374,#18375,#18376,#18377,#18378,#18379,#18380,#18381,#18382,#18383,#18384,
#18385,#18386,#18387,#18388,#18389,#18390,#18391,#18392,#18393,#18394,#18395,
#18396),.UNSPECIFIED.,.F.,.F.,(4,3,3,3,3,3,3,3,3,4),(480.663675999239,481.447876163288,
482.232076327337,483.016276491386,483.800476655435,484.584676819485,485.368876983534,
486.153077147583,486.937277311632,486.946861306418),.UNSPECIFIED.);
#445=B_SPLINE_CURVE_WITH_KNOTS('',3,(#18401,#18402,#18403,#18404,#18405,
#18406,#18407,#18408,#18409,#18410,#18411,#18412,#18413,#18414,#18415,#18416,
#18417,#18418,#18419,#18420,#18421,#18422,#18423,#18424,#18425,#18426,#18427,
#18428),.UNSPECIFIED.,.F.,.F.,(4,3,3,3,3,3,3,3,3,4),(474.380490692059,475.164690856108,
475.948891020157,476.733091184207,477.517291348256,478.301491512305,479.085691676354,
479.869891840403,480.654092004453,480.663675999239),.UNSPECIFIED.);
#446=B_SPLINE_CURVE_WITH_KNOTS('',3,(#18429,#18430,#18431,#18432,#18433,
#18434,#18435,#18436,#18437,#18438,#18439,#18440,#18441,#18442,#18443,#18444,
#18445,#18446,#18447,#18448,#18449,#18450,#18451,#18452,#18453,#18454,#18455,
#18456),.UNSPECIFIED.,.F.,.F.,(4,3,3,3,3,3,3,3,3,4),(474.380490692059,475.164690856108,
475.948891020158,476.733091184207,477.517291348256,478.301491512305,479.085691676354,
479.869891840404,480.654092004453,480.663675999239),.UNSPECIFIED.);
#447=B_SPLINE_CURVE_WITH_KNOTS('',3,(#18461,#18462,#18463,#18464,#18465,
#18466,#18467,#18468,#18469,#18470,#18471,#18472,#18473,#18474,#18475,#18476,
#18477,#18478,#18479,#18480,#18481,#18482,#18483,#18484,#18485,#18486,#18487,
#18488),.UNSPECIFIED.,.F.,.F.,(4,3,3,3,3,3,3,3,3,4),(468.097305384879,468.881505548929,
469.665705712978,470.449905877027,471.234106041076,472.018306205126,472.802506369175,
473.586706533224,474.370906697273,474.380490692059),.UNSPECIFIED.);
#448=B_SPLINE_CURVE_WITH_KNOTS('',3,(#18489,#18490,#18491,#18492,#18493,
#18494,#18495,#18496,#18497,#18498,#18499),.UNSPECIFIED.,.F.,.F.,(4,1,1,
1,1,1,1,1,4),(468.09730538488,469.063155297986,470.062643019988,471.062130741989,
471.56187460299,472.061618463991,473.061106185992,474.060593907994,474.380490692059),
 .UNSPECIFIED.);
#449=B_SPLINE_CURVE_WITH_KNOTS('',3,(#18504,#18505,#18506,#18507,#18508,
#18509,#18510,#18511,#18512,#18513,#18514,#18515,#18516,#18517,#18518,#18519,
#18520,#18521,#18522,#18523,#18524,#18525,#18526,#18527,#18528,#18529,#18530,
#18531),.UNSPECIFIED.,.F.,.F.,(4,3,3,3,3,3,3,3,3,4),(461.8141200777,462.598320241749,
463.382520405798,464.166720569848,464.950920733897,465.735120897946,466.519321061995,
467.303521226045,468.087721390094,468.097305384879),.UNSPECIFIED.);
#450=B_SPLINE_CURVE_WITH_KNOTS('',3,(#18532,#18533,#18534,#18535,#18536,
#18537,#18538,#18539,#18540,#18541,#18542,#18543,#18544,#18545,#18546,#18547,
#18548,#18549,#18550,#18551,#18552,#18553,#18554,#18555,#18556,#18557,#18558,
#18559),.UNSPECIFIED.,.F.,.F.,(4,3,3,3,3,3,3,3,3,4),(461.8141200777,462.598320241749,
463.382520405798,464.166720569848,464.950920733897,465.735120897946,466.519321061995,
467.303521226044,468.087721390094,468.09730538488),.UNSPECIFIED.);
#451=B_SPLINE_CURVE_WITH_KNOTS('',3,(#18564,#18565,#18566,#18567,#18568,
#18569,#18570,#18571,#18572,#18573,#18574,#18575,#18576,#18577,#18578,#18579,
#18580,#18581,#18582,#18583,#18584,#18585,#18586,#18587,#18588,#18589,#18590,
#18591),.UNSPECIFIED.,.F.,.F.,(4,3,3,3,3,3,3,3,3,4),(455.53093477052,456.31513493457,
457.099335098619,457.883535262668,458.667735426717,459.451935590767,460.236135754816,
461.020335918865,461.804536082914,461.8141200777),.UNSPECIFIED.);
#452=B_SPLINE_CURVE_WITH_KNOTS('',3,(#18592,#18593,#18594,#18595,#18596,
#18597,#18598,#18599,#18600,#18601,#18602,#18603,#18604,#18605,#18606,#18607,
#18608,#18609,#18610,#18611,#18612,#18613,#18614,#18615,#18616,#18617,#18618,
#18619),.UNSPECIFIED.,.F.,.F.,(4,3,3,3,3,3,3,3,3,4),(455.53093477052,456.31513493457,
457.099335098619,457.883535262668,458.667735426717,459.451935590766,460.236135754816,
461.020335918865,461.804536082914,461.8141200777),.UNSPECIFIED.);
#453=B_SPLINE_CURVE_WITH_KNOTS('',3,(#18624,#18625,#18626,#18627,#18628,
#18629,#18630,#18631,#18632,#18633,#18634,#18635,#18636,#18637,#18638,#18639,
#18640,#18641,#18642,#18643,#18644,#18645,#18646,#18647,#18648,#18649,#18650,
#18651),.UNSPECIFIED.,.F.,.F.,(4,3,3,3,3,3,3,3,3,4),(449.247749463341,450.03194962739,
450.816149791439,451.600349955488,452.384550119537,453.168750283587,453.952950447636,
454.737150611685,455.521350775734,455.53093477052),.UNSPECIFIED.);
#454=B_SPLINE_CURVE_WITH_KNOTS('',3,(#18652,#18653,#18654,#18655,#18656,
#18657,#18658,#18659,#18660,#18661,#18662,#18663,#18664,#18665,#18666,#18667,
#18668,#18669,#18670,#18671,#18672,#18673,#18674,#18675,#18676,#18677,#18678,
#18679),.UNSPECIFIED.,.F.,.F.,(4,3,3,3,3,3,3,3,3,4),(449.247749463341,450.03194962739,
450.816149791439,451.600349955488,452.384550119538,453.168750283587,453.952950447636,
454.737150611685,455.521350775734,455.53093477052),.UNSPECIFIED.);
#455=B_SPLINE_CURVE_WITH_KNOTS('',3,(#18684,#18685,#18686,#18687,#18688,
#18689,#18690,#18691,#18692,#18693,#18694,#18695,#18696,#18697,#18698,#18699,
#18700,#18701,#18702,#18703,#18704,#18705,#18706,#18707,#18708,#18709,#18710,
#18711),.UNSPECIFIED.,.F.,.F.,(4,3,3,3,3,3,3,3,3,4),(442.964564156161,443.74876432021,
444.532964484259,445.317164648309,446.101364812358,446.885564976407,447.669765140456,
448.453965304505,449.238165468555,449.247749463341),.UNSPECIFIED.);
#456=B_SPLINE_CURVE_WITH_KNOTS('',3,(#18712,#18713,#18714,#18715,#18716,
#18717,#18718,#18719,#18720,#18721,#18722,#18723,#18724,#18725,#18726,#18727,
#18728,#18729,#18730,#18731,#18732,#18733,#18734,#18735,#18736,#18737,#18738,
#18739),.UNSPECIFIED.,.F.,.F.,(4,3,3,3,3,3,3,3,3,4),(442.964564156161,443.748764320211,
444.53296448426,445.317164648309,446.101364812358,446.885564976407,447.669765140457,
448.453965304506,449.238165468555,449.247749463341),.UNSPECIFIED.);
#457=B_SPLINE_CURVE_WITH_KNOTS('',3,(#18744,#18745,#18746,#18747,#18748,
#18749,#18750,#18751,#18752,#18753,#18754),.UNSPECIFIED.,.F.,.F.,(4,1,1,
1,1,1,1,1,4),(436.681378848981,437.396802420487,438.396290142489,439.39577786449,
439.895521725491,440.395265586492,441.394753308494,442.394241030495,442.964564156161),
 .UNSPECIFIED.);
#458=B_SPLINE_CURVE_WITH_KNOTS('',3,(#18755,#18756,#18757,#18758,#18759,
#18760,#18761,#18762,#18763,#18764),.UNSPECIFIED.,.F.,.F.,(4,1,1,1,1,1,
1,4),(436.681378848982,437.079548193936,438.079035915937,439.078523637939,
440.078011359941,441.077499081942,442.076986803944,442.964564156161),
 .UNSPECIFIED.);
#459=B_SPLINE_CURVE_WITH_KNOTS('',3,(#18769,#18770,#18771,#18772,#18773,
#18774,#18775,#18776,#18777,#18778,#18779,#18780),.UNSPECIFIED.,.F.,.F.,
(4,1,1,1,1,1,1,1,1,4),(430.398193541802,430.400388366476,431.399876088478,
432.399363810479,432.89910767148,433.398851532481,434.398339254483,435.397826976484,
436.397314698486,436.681378848981),.UNSPECIFIED.);
#460=B_SPLINE_CURVE_WITH_KNOTS('',3,(#18781,#18782,#18783,#18784,#18785,
#18786,#18787,#18788,#18789,#18790,#18791,#18792,#18793,#18794,#18795,#18796,
#18797,#18798,#18799,#18800,#18801,#18802,#18803,#18804,#18805,#18806,#18807,
#18808),.UNSPECIFIED.,.F.,.F.,(4,3,3,3,3,3,3,3,3,4),(430.398193541802,431.182393705851,
431.966593869901,432.75079403395,433.534994197999,434.319194362049,435.103394526098,
435.887594690147,436.671794854196,436.681378848982),.UNSPECIFIED.);
#461=B_SPLINE_CURVE_WITH_KNOTS('',3,(#18813,#18814,#18815,#18816,#18817,
#18818,#18819,#18820,#18821,#18822,#18823,#18824,#18825,#18826,#18827,#18828,
#18829,#18830,#18831,#18832,#18833,#18834,#18835,#18836,#18837,#18838,#18839,
#18840),.UNSPECIFIED.,.F.,.F.,(4,3,3,3,3,3,3,3,3,4),(424.115008234622,424.899208398672,
425.683408562721,426.46760872677,427.251808890819,428.036009054868,428.820209218918,
429.604409382967,430.388609547016,430.398193541802),.UNSPECIFIED.);
#462=B_SPLINE_CURVE_WITH_KNOTS('',3,(#18841,#18842,#18843,#18844,#18845,
#18846,#18847,#18848,#18849,#18850,#18851,#18852,#18853,#18854,#18855,#18856,
#18857,#18858,#18859,#18860,#18861,#18862,#18863,#18864,#18865,#18866,#18867,
#18868),.UNSPECIFIED.,.F.,.F.,(4,3,3,3,3,3,3,3,3,4),(424.115008234623,424.899208398672,
425.683408562721,426.46760872677,427.25180889082,428.036009054869,428.820209218918,
429.604409382967,430.388609547017,430.398193541802),.UNSPECIFIED.);
#463=B_SPLINE_CURVE_WITH_KNOTS('',3,(#18873,#18874,#18875,#18876,#18877,
#18878,#18879,#18880,#18881,#18882,#18883,#18884,#18885,#18886,#18887,#18888,
#18889,#18890,#18891,#18892,#18893,#18894,#18895,#18896,#18897,#18898,#18899,
#18900),.UNSPECIFIED.,.F.,.F.,(4,3,3,3,3,3,3,3,3,4),(417.831822927443,418.616023091492,
419.400223255541,420.18442341959,420.968623583639,421.752823747689,422.537023911738,
423.321224075787,424.105424239836,424.115008234622),.UNSPECIFIED.);
#464=B_SPLINE_CURVE_WITH_KNOTS('',3,(#18901,#18902,#18903,#18904,#18905,
#18906,#18907,#18908,#18909,#18910,#18911,#18912,#18913,#18914,#18915,#18916,
#18917,#18918,#18919,#18920,#18921,#18922,#18923,#18924,#18925,#18926,#18927,
#18928),.UNSPECIFIED.,.F.,.F.,(4,3,3,3,3,3,3,3,3,4),(417.831822927443,418.616023091492,
419.400223255541,420.184423419591,420.96862358364,421.752823747689,422.537023911738,
423.321224075787,424.105424239836,424.115008234623),.UNSPECIFIED.);
#465=B_SPLINE_CURVE_WITH_KNOTS('',3,(#18933,#18934,#18935,#18936,#18937,
#18938,#18939,#18940,#18941,#18942,#18943),.UNSPECIFIED.,.F.,.F.,(4,1,1,
1,1,1,1,1,4),(411.548637620263,411.909865509447,412.409609370448,413.40909709245,
414.408584814451,415.408072536453,416.407560258454,417.407047980456,417.831822927443),
 .UNSPECIFIED.);
#466=B_SPLINE_CURVE_WITH_KNOTS('',3,(#18944,#18945,#18946,#18947,#18948,
#18949,#18950,#18951,#18952,#18953,#18954,#18955,#18956,#18957,#18958,#18959,
#18960,#18961,#18962,#18963,#18964,#18965,#18966,#18967,#18968,#18969,#18970,
#18971),.UNSPECIFIED.,.F.,.F.,(4,3,3,3,3,3,3,3,3,4),(411.548637620263,412.332837784313,
413.117037948362,413.901238112411,414.68543827646,415.469638440509,416.253838604559,
417.038038768608,417.822238932657,417.831822927443),.UNSPECIFIED.);
#467=B_SPLINE_CURVE_WITH_KNOTS('',3,(#18976,#18977,#18978,#18979,#18980,
#18981,#18982,#18983,#18984,#18985,#18986,#18987,#18988,#18989,#18990,#18991,
#18992,#18993,#18994,#18995,#18996,#18997,#18998,#18999,#19000,#19001,#19002,
#19003),.UNSPECIFIED.,.F.,.F.,(4,3,3,3,3,3,3,3,3,4),(405.265452313084,406.049652477133,
406.833852641182,407.618052805231,408.40225296928,409.186453133329,409.970653297379,
410.754853461428,411.539053625477,411.548637620263),.UNSPECIFIED.);
#468=B_SPLINE_CURVE_WITH_KNOTS('',3,(#19004,#19005,#19006,#19007,#19008,
#19009,#19010,#19011,#19012,#19013,#19014),.UNSPECIFIED.,.F.,.F.,(4,1,1,
1,1,1,1,1,4),(405.265452313084,406.095428811887,407.094916533889,408.09440425589,
408.594148116891,409.093891977892,410.093379699894,411.092867421895,411.548637620263),
 .UNSPECIFIED.);
#469=B_SPLINE_CURVE_WITH_KNOTS('',3,(#19019,#19020,#19021,#19022,#19023,
#19024,#19025,#19026,#19027,#19028,#19029),.UNSPECIFIED.,.F.,.F.,(4,1,1,
1,1,1,1,1,4),(398.982267005904,399.416268984428,400.415756706429,401.415244428431,
402.414732150432,403.414219872434,404.413707594436,404.913451455436,405.265452313084),
 .UNSPECIFIED.);
#470=B_SPLINE_CURVE_WITH_KNOTS('',3,(#19030,#19031,#19032,#19033,#19034,
#19035,#19036,#19037,#19038,#19039,#19040,#19041,#19042,#19043,#19044,#19045,
#19046,#19047,#19048,#19049,#19050,#19051,#19052,#19053,#19054,#19055,#19056,
#19057),.UNSPECIFIED.,.F.,.F.,(4,3,3,3,3,3,3,3,3,4),(398.982267005904,399.766467169954,
400.550667334003,401.334867498052,402.119067662101,402.903267826151,403.6874679902,
404.471668154249,405.255868318298,405.265452313084),.UNSPECIFIED.);
#471=B_SPLINE_CURVE_WITH_KNOTS('',3,(#19062,#19063,#19064,#19065,#19066,
#19067,#19068,#19069,#19070,#19071,#19072,#19073,#19074,#19075,#19076,#19077,
#19078,#19079,#19080,#19081,#19082,#19083,#19084,#19085,#19086,#19087,#19088,
#19089),.UNSPECIFIED.,.F.,.F.,(4,3,3,3,3,3,3,3,3,4),(392.699081698725,393.483281862774,
394.267482026823,395.051682190872,395.835882354922,396.620082518971,397.40428268302,
398.188482847069,398.972683011119,398.982267005904),.UNSPECIFIED.);
#472=B_SPLINE_CURVE_WITH_KNOTS('',3,(#19090,#19091,#19092,#19093,#19094,
#19095,#19096,#19097,#19098,#19099,#19100,#19101,#19102,#19103,#19104,#19105,
#19106,#19107,#19108,#19109,#19110,#19111,#19112,#19113,#19114,#19115,#19116,
#19117),.UNSPECIFIED.,.F.,.F.,(4,3,3,3,3,3,3,3,3,4),(392.699081698725,393.483281862774,
394.267482026823,395.051682190872,395.835882354921,396.620082518971,397.40428268302,
398.188482847069,398.972683011118,398.982267005904),.UNSPECIFIED.);
#473=B_SPLINE_CURVE_WITH_KNOTS('',3,(#19122,#19123,#19124,#19125,#19126,
#19127,#19128,#19129,#19130,#19131,#19132,#19133,#19134,#19135,#19136,#19137,
#19138,#19139,#19140,#19141,#19142,#19143,#19144,#19145,#19146,#19147,#19148,
#19149),.UNSPECIFIED.,.F.,.F.,(4,3,3,3,3,3,3,3,3,4),(386.415896391545,387.200096555594,
387.984296719643,388.768496883693,389.552697047742,390.336897211791,391.12109737584,
391.905297539889,392.689497703939,392.699081698725),.UNSPECIFIED.);
#474=B_SPLINE_CURVE_WITH_KNOTS('',3,(#19150,#19151,#19152,#19153,#19154,
#19155,#19156,#19157,#19158,#19159,#19160,#19161,#19162,#19163,#19164,#19165,
#19166,#19167,#19168,#19169,#19170,#19171,#19172,#19173,#19174,#19175,#19176,
#19177),.UNSPECIFIED.,.F.,.F.,(4,3,3,3,3,3,3,3,3,4),(386.415896391545,387.200096555594,
387.984296719644,388.768496883693,389.552697047742,390.336897211791,391.12109737584,
391.90529753989,392.689497703939,392.699081698725),.UNSPECIFIED.);
#475=B_SPLINE_CURVE_WITH_KNOTS('',3,(#19182,#19183,#19184,#19185,#19186,
#19187,#19188,#19189,#19190,#19191,#19192),.UNSPECIFIED.,.F.,.F.,(4,1,1,
1,1,1,1,1,4),(380.132711084365,380.426002266398,381.4254899884,382.424977710401,
383.424465432403,383.924209293403,384.423953154404,385.423440876406,386.415896391545),
 .UNSPECIFIED.);
#476=B_SPLINE_CURVE_WITH_KNOTS('',3,(#19193,#19194,#19195,#19196,#19197,
#19198,#19199,#19200,#19201,#19202,#19203,#19204,#19205,#19206,#19207,#19208,
#19209,#19210,#19211,#19212,#19213,#19214,#19215,#19216,#19217,#19218,#19219,
#19220),.UNSPECIFIED.,.F.,.F.,(4,3,3,3,3,3,3,3,3,4),(380.132711084366,380.916911248415,
381.701111412464,382.485311576513,383.269511740562,384.053711904611,384.837912068661,
385.62211223271,386.406312396759,386.415896391545),.UNSPECIFIED.);
#477=B_SPLINE_CURVE_WITH_KNOTS('',3,(#19225,#19226,#19227,#19228,#19229,
#19230,#19231,#19232,#19233,#19234,#19235),.UNSPECIFIED.,.F.,.F.,(4,1,1,
1,1,1,1,1,4),(373.849525777186,374.429075934389,375.42856365639,376.428051378392,
376.927795239393,377.427539100393,378.427026822395,379.426514544396,380.132711084365),
 .UNSPECIFIED.);
#478=B_SPLINE_CURVE_WITH_KNOTS('',3,(#19236,#19237,#19238,#19239,#19240,
#19241,#19242,#19243,#19244,#19245,#19246,#19247,#19248,#19249,#19250,#19251,
#19252,#19253,#19254,#19255,#19256,#19257,#19258,#19259,#19260,#19261,#19262,
#19263),.UNSPECIFIED.,.F.,.F.,(4,3,3,3,3,3,3,3,3,4),(373.849525777186,374.633725941235,
375.417926105284,376.202126269334,376.986326433383,377.770526597432,378.554726761481,
379.33892692553,380.12312708958,380.132711084366),.UNSPECIFIED.);
#479=B_SPLINE_CURVE_WITH_KNOTS('',3,(#19268,#19269,#19270,#19271,#19272,
#19273,#19274,#19275,#19276,#19277,#19278,#19279,#19280,#19281,#19282,#19283,
#19284,#19285,#19286,#19287,#19288,#19289,#19290,#19291,#19292,#19293,#19294,
#19295),.UNSPECIFIED.,.F.,.F.,(4,3,3,3,3,3,3,3,3,4),(367.566340470006,368.350540634056,
369.134740798105,369.918940962154,370.703141126203,371.487341290252,372.271541454301,
373.055741618351,373.8399417824,373.849525777186),.UNSPECIFIED.);
#480=B_SPLINE_CURVE_WITH_KNOTS('',3,(#19296,#19297,#19298,#19299,#19300,
#19301,#19302,#19303,#19304,#19305,#19306,#19307,#19308,#19309,#19310,#19311,
#19312,#19313,#19314,#19315,#19316,#19317,#19318,#19319,#19320,#19321,#19322,
#19323),.UNSPECIFIED.,.F.,.F.,(4,3,3,3,3,3,3,3,3,4),(367.566340470007,368.350540634056,
369.134740798105,369.918940962155,370.703141126204,371.487341290253,372.271541454302,
373.055741618352,373.839941782401,373.849525777186),.UNSPECIFIED.);
#481=B_SPLINE_CURVE_WITH_KNOTS('',3,(#19328,#19329,#19330,#19331,#19332,
#19333,#19334,#19335,#19336,#19337,#19338,#19339,#19340,#19341,#19342,#19343,
#19344,#19345,#19346,#19347,#19348,#19349,#19350,#19351,#19352,#19353,#19354,
#19355),.UNSPECIFIED.,.F.,.F.,(4,3,3,3,3,3,3,3,3,4),(361.283155162827,362.067355326876,
362.851555490925,363.635755654975,364.419955819024,365.204155983073,365.988356147122,
366.772556311172,367.556756475221,367.566340470006),.UNSPECIFIED.);
#482=B_SPLINE_CURVE_WITH_KNOTS('',3,(#19356,#19357,#19358,#19359,#19360,
#19361,#19362,#19363,#19364,#19365,#19366,#19367,#19368,#19369,#19370,#19371,
#19372,#19373,#19374,#19375,#19376,#19377,#19378,#19379,#19380,#19381,#19382,
#19383),.UNSPECIFIED.,.F.,.F.,(4,3,3,3,3,3,3,3,3,4),(361.283155162827,362.067355326876,
362.851555490926,363.635755654975,364.419955819024,365.204155983073,365.988356147123,
366.772556311172,367.556756475221,367.566340470007),.UNSPECIFIED.);
#483=B_SPLINE_CURVE_WITH_KNOTS('',3,(#19388,#19389,#19390,#19391,#19392,
#19393,#19394,#19395,#19396,#19397,#19398,#19399,#19400,#19401,#19402,#19403,
#19404,#19405,#19406,#19407,#19408,#19409,#19410,#19411,#19412,#19413,#19414,
#19415),.UNSPECIFIED.,.F.,.F.,(4,3,3,3,3,3,3,3,3,4),(354.999969855647,355.784170019696,
356.568370183746,357.352570347795,358.136770511844,358.920970675893,359.705170839943,
360.489371003992,361.273571168041,361.283155162827),.UNSPECIFIED.);
#484=B_SPLINE_CURVE_WITH_KNOTS('',3,(#19416,#19417,#19418,#19419,#19420,
#19421,#19422,#19423,#19424,#19425,#19426,#19427,#19428,#19429,#19430,#19431,
#19432,#19433,#19434,#19435,#19436,#19437,#19438,#19439,#19440,#19441,#19442,
#19443),.UNSPECIFIED.,.F.,.F.,(4,3,3,3,3,3,3,3,3,4),(354.999969855647,355.784170019697,
356.568370183746,357.352570347795,358.136770511844,358.920970675893,359.705170839943,
360.489371003992,361.273571168041,361.283155162827),.UNSPECIFIED.);
#485=B_SPLINE_CURVE_WITH_KNOTS('',3,(#19448,#19449,#19450,#19451,#19452,
#19453,#19454,#19455,#19456,#19457,#19458,#19459,#19460,#19461,#19462,#19463,
#19464,#19465,#19466,#19467,#19468,#19469,#19470,#19471,#19472,#19473,#19474,
#19475),.UNSPECIFIED.,.F.,.F.,(4,3,3,3,3,3,3,3,3,4),(348.716784548468,349.500984712517,
350.285184876566,351.069385040616,351.853585204665,352.637785368714,353.421985532763,
354.206185696813,354.990385860862,354.999969855647),.UNSPECIFIED.);
#486=B_SPLINE_CURVE_WITH_KNOTS('',3,(#19476,#19477,#19478,#19479,#19480,
#19481,#19482,#19483,#19484,#19485,#19486,#19487,#19488,#19489,#19490,#19491,
#19492,#19493,#19494,#19495,#19496,#19497,#19498,#19499,#19500,#19501,#19502,
#19503),.UNSPECIFIED.,.F.,.F.,(4,3,3,3,3,3,3,3,3,4),(348.716784548468,349.500984712517,
350.285184876566,351.069385040615,351.853585204664,352.637785368713,353.421985532762,
354.206185696811,354.990385860861,354.999969855647),.UNSPECIFIED.);
#487=B_SPLINE_CURVE_WITH_KNOTS('',3,(#19508,#19509,#19510,#19511,#19512,
#19513,#19514,#19515,#19516,#19517,#19518,#19519,#19520,#19521,#19522,#19523,
#19524,#19525,#19526,#19527,#19528,#19529,#19530,#19531,#19532,#19533,#19534,
#19535),.UNSPECIFIED.,.F.,.F.,(4,3,3,3,3,3,3,3,3,4),(342.433599241288,343.217799405337,
344.001999569386,344.786199733435,345.570399897485,346.354600061534,347.138800225583,
347.923000389632,348.707200553681,348.716784548468),.UNSPECIFIED.);
#488=B_SPLINE_CURVE_WITH_KNOTS('',3,(#19536,#19537,#19538,#19539,#19540,
#19541,#19542,#19543,#19544,#19545,#19546),.UNSPECIFIED.,.F.,.F.,(4,1,1,
1,1,1,1,1,4),(342.433599241288,343.127702325789,344.12719004779,345.126677769792,
345.626421630792,346.126165491793,347.125653213795,348.125140935796,348.716784548468),
 .UNSPECIFIED.);
#489=B_SPLINE_CURVE_WITH_KNOTS('',3,(#19551,#19552,#19553,#19554,#19555,
#19556,#19557,#19558,#19559,#19560,#19561,#19562,#19563,#19564,#19565,#19566,
#19567,#19568,#19569,#19570,#19571,#19572,#19573,#19574,#19575,#19576,#19577,
#19578),.UNSPECIFIED.,.F.,.F.,(4,3,3,3,3,3,3,3,3,4),(336.150413934109,336.934614098158,
337.718814262207,338.503014426256,339.287214590305,340.071414754354,340.855614918403,
341.639815082453,342.424015246502,342.433599241288),.UNSPECIFIED.);
#490=B_SPLINE_CURVE_WITH_KNOTS('',3,(#19579,#19580,#19581,#19582,#19583,
#19584,#19585,#19586,#19587,#19588,#19589),.UNSPECIFIED.,.F.,.F.,(4,1,1,
1,1,1,1,1,4),(336.150413934109,337.130775993779,338.130263715781,338.630007576781,
339.129751437782,340.129239159784,341.128726881785,342.128214603787,342.433599241288),
 .UNSPECIFIED.);
#491=B_SPLINE_CURVE_WITH_KNOTS('',3,(#19594,#19595,#19596,#19597,#19598,
#19599,#19600,#19601,#19602,#19603,#19604,#19605,#19606,#19607,#19608,#19609,
#19610,#19611,#19612,#19613,#19614,#19615,#19616,#19617,#19618,#19619,#19620,
#19621),.UNSPECIFIED.,.F.,.F.,(4,3,3,3,3,3,3,3,3,4),(329.867228626929,330.651428790978,
331.435628955027,332.219829119077,333.004029283126,333.788229447175,334.572429611224,
335.356629775273,336.140829939323,336.150413934109),.UNSPECIFIED.);
#492=B_SPLINE_CURVE_WITH_KNOTS('',3,(#19622,#19623,#19624,#19625,#19626,
#19627,#19628,#19629,#19630,#19631,#19632,#19633,#19634,#19635,#19636,#19637,
#19638,#19639,#19640,#19641,#19642,#19643,#19644,#19645,#19646,#19647,#19648,
#19649),.UNSPECIFIED.,.F.,.F.,(4,3,3,3,3,3,3,3,3,4),(329.867228626929,330.651428790978,
331.435628955028,332.219829119077,333.004029283126,333.788229447175,334.572429611224,
335.356629775274,336.140829939323,336.150413934109),.UNSPECIFIED.);
#493=B_SPLINE_CURVE_WITH_KNOTS('',3,(#19654,#19655,#19656,#19657,#19658,
#19659,#19660,#19661,#19662,#19663,#19664,#19665,#19666,#19667,#19668,#19669,
#19670,#19671,#19672,#19673,#19674,#19675,#19676,#19677,#19678,#19679,#19680,
#19681),.UNSPECIFIED.,.F.,.F.,(4,3,3,3,3,3,3,3,3,4),(323.584043319749,324.368243483799,
325.152443647848,325.936643811897,326.720843975946,327.505044139995,328.289244304045,
329.073444468094,329.857644632143,329.867228626929),.UNSPECIFIED.);
#494=B_SPLINE_CURVE_WITH_KNOTS('',3,(#19682,#19683,#19684,#19685,#19686,
#19687,#19688,#19689,#19690,#19691,#19692,#19693,#19694,#19695,#19696,#19697,
#19698,#19699,#19700,#19701,#19702,#19703,#19704,#19705,#19706,#19707,#19708,
#19709),.UNSPECIFIED.,.F.,.F.,(4,3,3,3,3,3,3,3,3,4),(323.58404331975,324.368243483799,
325.152443647848,325.936643811897,326.720843975946,327.505044139996,328.289244304045,
329.073444468094,329.857644632143,329.867228626929),.UNSPECIFIED.);
#495=B_SPLINE_CURVE_WITH_KNOTS('',3,(#19714,#19715,#19716,#19717,#19718,
#19719,#19720,#19721,#19722,#19723,#19724,#19725,#19726,#19727,#19728,#19729,
#19730,#19731,#19732,#19733,#19734,#19735,#19736,#19737,#19738,#19739,#19740,
#19741),.UNSPECIFIED.,.F.,.F.,(4,3,3,3,3,3,3,3,3,4),(317.30085801257,318.085058176619,
318.869258340668,319.653458504718,320.437658668767,321.221858832816,322.006058996865,
322.790259160915,323.574459324964,323.584043319749),.UNSPECIFIED.);
#496=B_SPLINE_CURVE_WITH_KNOTS('',3,(#19742,#19743,#19744,#19745,#19746,
#19747,#19748,#19749,#19750,#19751,#19752),.UNSPECIFIED.,.F.,.F.,(4,1,1,
1,1,1,1,1,4),(317.30085801257,317.640765414749,318.140509275749,319.139996997751,
320.139484719752,321.138972441754,322.138460163756,323.137947885757,323.58404331975),
 .UNSPECIFIED.);
#497=B_SPLINE_CURVE_WITH_KNOTS('',3,(#19757,#19758,#19759,#19760,#19761,
#19762,#19763,#19764,#19765,#19766,#19767),.UNSPECIFIED.,.F.,.F.,(4,1,1,
1,1,1,1,1,4),(311.01767270539,311.46134944829,312.460837170291,313.460324892293,
313.960068753294,314.459812614295,315.459300336296,316.458788058298,317.30085801257),
 .UNSPECIFIED.);
#498=B_SPLINE_CURVE_WITH_KNOTS('',3,(#19768,#19769,#19770,#19771,#19772,
#19773,#19774,#19775,#19776,#19777,#19778,#19779,#19780,#19781,#19782,#19783,
#19784,#19785,#19786,#19787,#19788,#19789,#19790,#19791,#19792,#19793,#19794,
#19795),.UNSPECIFIED.,.F.,.F.,(4,3,3,3,3,3,3,3,3,4),(311.01767270539,311.80187286944,
312.586073033489,313.370273197538,314.154473361587,314.938673525636,315.722873689685,
316.507073853734,317.291274017784,317.30085801257),.UNSPECIFIED.);
#499=B_SPLINE_CURVE_WITH_KNOTS('',3,(#19800,#19801,#19802,#19803,#19804,
#19805,#19806,#19807,#19808,#19809,#19810,#19811,#19812,#19813,#19814,#19815,
#19816,#19817,#19818,#19819,#19820,#19821,#19822,#19823,#19824,#19825,#19826,
#19827),.UNSPECIFIED.,.F.,.F.,(4,3,3,3,3,3,3,3,3,4),(304.734487398211,305.51868756226,
306.302887726309,307.087087890358,307.871288054408,308.655488218457,309.439688382506,
310.223888546555,311.008088710604,311.01767270539),.UNSPECIFIED.);
#500=B_SPLINE_CURVE_WITH_KNOTS('',3,(#19828,#19829,#19830,#19831,#19832,
#19833,#19834,#19835,#19836,#19837,#19838),.UNSPECIFIED.,.F.,.F.,(4,1,1,
1,1,1,1,1,4),(304.734487398211,305.147168889729,306.146656611731,307.146144333732,
308.145632055734,309.145119777735,310.144607499737,310.644351360738,311.01767270539),
 .UNSPECIFIED.);
#501=B_SPLINE_CURVE_WITH_KNOTS('',3,(#19843,#19844,#19845,#19846,#19847,
#19848,#19849,#19850,#19851,#19852,#19853,#19854,#19855,#19856,#19857,#19858,
#19859,#19860,#19861,#19862,#19863,#19864,#19865,#19866,#19867,#19868,#19869,
#19870),.UNSPECIFIED.,.F.,.F.,(4,3,3,3,3,3,3,3,3,4),(298.451302091031,299.23550225508,
300.019702419129,300.803902583179,301.588102747228,302.372302911277,303.156503075326,
303.940703239375,304.724903403425,304.734487398211),.UNSPECIFIED.);
#502=B_SPLINE_CURVE_WITH_KNOTS('',3,(#19871,#19872,#19873,#19874,#19875,
#19876,#19877,#19878,#19879,#19880,#19881,#19882,#19883,#19884,#19885,#19886,
#19887,#19888,#19889,#19890,#19891,#19892,#19893,#19894,#19895,#19896,#19897,
#19898),.UNSPECIFIED.,.F.,.F.,(4,3,3,3,3,3,3,3,3,4),(298.451302091031,299.235502255081,
300.01970241913,300.803902583179,301.588102747228,302.372302911278,303.156503075327,
303.940703239376,304.724903403425,304.734487398211),.UNSPECIFIED.);
#503=B_SPLINE_CURVE_WITH_KNOTS('',3,(#19903,#19904,#19905,#19906,#19907,
#19908,#19909,#19910,#19911,#19912,#19913),.UNSPECIFIED.,.F.,.F.,(4,1,1,
1,1,1,1,1,4),(292.168116783852,292.47108273026,293.470570452262,294.470058174263,
294.969802035264,295.469545896265,296.469033618266,297.468521340268,298.451302091031),
 .UNSPECIFIED.);
#504=B_SPLINE_CURVE_WITH_KNOTS('',3,(#19914,#19915,#19916,#19917,#19918,
#19919,#19920,#19921,#19922,#19923,#19924,#19925,#19926,#19927,#19928,#19929,
#19930,#19931,#19932,#19933,#19934,#19935,#19936,#19937,#19938,#19939,#19940,
#19941),.UNSPECIFIED.,.F.,.F.,(4,3,3,3,3,3,3,3,3,4),(292.168116783852,292.952316947901,
293.73651711195,294.520717276,295.304917440049,296.089117604098,296.873317768147,
297.657517932197,298.441718096246,298.451302091031),.UNSPECIFIED.);
#505=B_SPLINE_CURVE_WITH_KNOTS('',3,(#19946,#19947,#19948,#19949,#19950,
#19951,#19952,#19953,#19954,#19955,#19956,#19957,#19958,#19959,#19960,#19961,
#19962,#19963,#19964,#19965,#19966,#19967,#19968,#19969,#19970,#19971,#19972,
#19973),.UNSPECIFIED.,.F.,.F.,(4,3,3,3,3,3,3,3,3,4),(285.884931476672,286.669131640721,
287.45333180477,288.23753196882,289.021732132869,289.805932296918,290.590132460967,
291.374332625016,292.158532789066,292.168116783852),.UNSPECIFIED.);
#506=B_SPLINE_CURVE_WITH_KNOTS('',3,(#19974,#19975,#19976,#19977,#19978,
#19979,#19980,#19981,#19982,#19983,#19984,#19985,#19986,#19987,#19988,#19989,
#19990,#19991,#19992,#19993,#19994,#19995,#19996,#19997,#19998,#19999,#20000,
#20001),.UNSPECIFIED.,.F.,.F.,(4,3,3,3,3,3,3,3,3,4),(285.884931476672,286.669131640721,
287.453331804771,288.23753196882,289.021732132869,289.805932296918,290.590132460967,
291.374332625017,292.158532789066,292.168116783852),.UNSPECIFIED.);
#507=B_SPLINE_CURVE_WITH_KNOTS('',3,(#20006,#20007,#20008,#20009,#20010,
#20011,#20012,#20013,#20014,#20015,#20016,#20017,#20018,#20019,#20020,#20021,
#20022,#20023,#20024,#20025,#20026,#20027,#20028,#20029,#20030,#20031,#20032,
#20033),.UNSPECIFIED.,.F.,.F.,(4,3,3,3,3,3,3,3,3,4),(279.601746169492,280.385946333542,
281.170146497591,281.95434666164,282.738546825689,283.522746989739,284.306947153788,
285.091147317837,285.875347481886,285.884931476672),.UNSPECIFIED.);
#508=B_SPLINE_CURVE_WITH_KNOTS('',3,(#20034,#20035,#20036,#20037,#20038,
#20039,#20040,#20041,#20042,#20043,#20044,#20045,#20046,#20047,#20048,#20049,
#20050,#20051,#20052,#20053,#20054,#20055,#20056,#20057,#20058,#20059,#20060,
#20061),.UNSPECIFIED.,.F.,.F.,(4,3,3,3,3,3,3,3,3,4),(279.601746169493,280.385946333542,
281.170146497591,281.95434666164,282.738546825689,283.522746989739,284.306947153788,
285.091147317837,285.875347481886,285.884931476672),.UNSPECIFIED.);
#509=B_SPLINE_CURVE_WITH_KNOTS('',3,(#20066,#20067,#20068,#20069,#20070,
#20071,#20072,#20073,#20074,#20075,#20076,#20077,#20078,#20079,#20080,#20081,
#20082,#20083,#20084,#20085,#20086,#20087,#20088,#20089,#20090,#20091,#20092,
#20093),.UNSPECIFIED.,.F.,.F.,(4,3,3,3,3,3,3,3,3,4),(273.318560862313,274.102761026362,
274.886961190411,275.67116135446,276.45536151851,277.239561682559,278.023761846608,
278.807962010657,279.592162174706,279.601746169492),.UNSPECIFIED.);
#510=B_SPLINE_CURVE_WITH_KNOTS('',3,(#20094,#20095,#20096,#20097,#20098,
#20099,#20100,#20101,#20102,#20103,#20104,#20105,#20106,#20107,#20108,#20109,
#20110,#20111,#20112,#20113,#20114,#20115,#20116,#20117,#20118,#20119,#20120,
#20121),.UNSPECIFIED.,.F.,.F.,(4,3,3,3,3,3,3,3,3,4),(273.318560862313,274.102761026362,
274.886961190412,275.671161354461,276.45536151851,277.239561682559,278.023761846609,
278.807962010658,279.592162174707,279.601746169493),.UNSPECIFIED.);
#511=B_SPLINE_CURVE_WITH_KNOTS('',3,(#20126,#20127,#20128,#20129,#20130,
#20131,#20132,#20133,#20134,#20135,#20136,#20137,#20138,#20139,#20140,#20141,
#20142,#20143,#20144,#20145,#20146,#20147,#20148,#20149,#20150,#20151,#20152,
#20153),.UNSPECIFIED.,.F.,.F.,(4,3,3,3,3,3,3,3,3,4),(267.035375555133,267.819575719182,
268.603775883232,269.387976047281,270.17217621133,270.956376375379,271.740576539428,
272.524776703478,273.308976867527,273.318560862313),.UNSPECIFIED.);
#512=B_SPLINE_CURVE_WITH_KNOTS('',3,(#20154,#20155,#20156,#20157,#20158,
#20159,#20160,#20161,#20162,#20163,#20164,#20165,#20166,#20167,#20168,#20169,
#20170,#20171,#20172,#20173,#20174,#20175,#20176,#20177,#20178,#20179,#20180,
#20181),.UNSPECIFIED.,.F.,.F.,(4,3,3,3,3,3,3,3,3,4),(267.035375555134,267.819575719183,
268.603775883232,269.387976047281,270.17217621133,270.956376375379,271.740576539428,
272.524776703478,273.308976867527,273.318560862313),.UNSPECIFIED.);
#513=B_SPLINE_CURVE_WITH_KNOTS('',3,(#20186,#20187,#20188,#20189,#20190,
#20191,#20192,#20193,#20194,#20195,#20196,#20197,#20198,#20199,#20200,#20201,
#20202,#20203,#20204,#20205,#20206,#20207,#20208,#20209,#20210,#20211,#20212,
#20213),.UNSPECIFIED.,.F.,.F.,(4,3,3,3,3,3,3,3,3,4),(260.752190247954,261.536390412003,
262.320590576052,263.104790740101,263.888990904151,264.6731910682,265.457391232249,
266.241591396298,267.025791560347,267.035375555133),.UNSPECIFIED.);
#514=B_SPLINE_CURVE_WITH_KNOTS('',3,(#20214,#20215,#20216,#20217,#20218,
#20219,#20220,#20221,#20222,#20223,#20224),.UNSPECIFIED.,.F.,.F.,(4,1,1,
1,1,1,1,1,4),(260.752190247954,261.16970912166,262.169196843661,263.168684565663,
263.668428426664,264.168172287665,265.167660009666,266.167147731668,267.035375555134),
 .UNSPECIFIED.);
#515=B_SPLINE_CURVE_WITH_KNOTS('',3,(#20229,#20230,#20231,#20232,#20233,
#20234,#20235,#20236,#20237,#20238,#20239,#20240,#20241,#20242,#20243,#20244,
#20245,#20246,#20247,#20248,#20249,#20250,#20251,#20252,#20253,#20254,#20255,
#20256),.UNSPECIFIED.,.F.,.F.,(4,3,3,3,3,3,3,3,3,4),(254.469004940774,255.253205104823,
256.037405268872,256.821605432922,257.605805596971,258.39000576102,259.174205925069,
259.958406089118,260.742606253167,260.752190247954),.UNSPECIFIED.);
#516=B_SPLINE_CURVE_WITH_KNOTS('',3,(#20257,#20258,#20259,#20260,#20261,
#20262,#20263,#20264,#20265,#20266,#20267,#20268,#20269,#20270,#20271,#20272,
#20273,#20274,#20275,#20276,#20277,#20278,#20279,#20280,#20281,#20282,#20283,
#20284),.UNSPECIFIED.,.F.,.F.,(4,3,3,3,3,3,3,3,3,4),(254.469004940774,255.253205104824,
256.037405268873,256.821605432922,257.605805596971,258.39000576102,259.174205925069,
259.958406089118,260.742606253168,260.752190247954),.UNSPECIFIED.);
#517=B_SPLINE_CURVE_WITH_KNOTS('',3,(#20289,#20290,#20291,#20292,#20293,
#20294,#20295,#20296,#20297,#20298,#20299,#20300,#20301,#20302,#20303,#20304,
#20305,#20306,#20307,#20308,#20309,#20310,#20311,#20312,#20313,#20314,#20315,
#20316),.UNSPECIFIED.,.F.,.F.,(4,3,3,3,3,3,3,3,3,4),(248.185819633595,248.970019797644,
249.754219961693,250.538420125742,251.322620289791,252.10682045384,252.89102061789,
253.675220781939,254.459420945988,254.469004940774),.UNSPECIFIED.);
#518=B_SPLINE_CURVE_WITH_KNOTS('',3,(#20317,#20318,#20319,#20320,#20321,
#20322,#20323,#20324,#20325,#20326,#20327,#20328,#20329,#20330,#20331,#20332,
#20333,#20334,#20335,#20336,#20337,#20338,#20339,#20340,#20341,#20342,#20343,
#20344),.UNSPECIFIED.,.F.,.F.,(4,3,3,3,3,3,3,3,3,4),(248.185819633595,248.970019797644,
249.754219961693,250.538420125742,251.322620289792,252.106820453841,252.89102061789,
253.675220781939,254.459420945988,254.469004940774),.UNSPECIFIED.);
#519=B_SPLINE_CURVE_WITH_KNOTS('',3,(#20349,#20350,#20351,#20352,#20353,
#20354,#20355,#20356,#20357,#20358,#20359,#20360,#20361,#20362,#20363,#20364,
#20365,#20366,#20367,#20368,#20369,#20370,#20371,#20372,#20373,#20374,#20375,
#20376),.UNSPECIFIED.,.F.,.F.,(4,3,3,3,3,3,3,3,3,4),(241.902634326415,242.686834490464,
243.471034654513,244.255234818563,245.039434982612,245.823635146661,246.60783531071,
247.392035474759,248.176235638809,248.185819633595),.UNSPECIFIED.);
#520=B_SPLINE_CURVE_WITH_KNOTS('',3,(#20377,#20378,#20379,#20380,#20381,
#20382,#20383,#20384,#20385,#20386,#20387,#20388,#20389,#20390,#20391,#20392,
#20393,#20394,#20395,#20396,#20397,#20398,#20399,#20400,#20401,#20402,#20403,
#20404),.UNSPECIFIED.,.F.,.F.,(4,3,3,3,3,3,3,3,3,4),(241.902634326415,242.686834490465,
243.471034654514,244.255234818563,245.039434982612,245.823635146661,246.60783531071,
247.39203547476,248.176235638809,248.185819633595),.UNSPECIFIED.);
#521=B_SPLINE_CURVE_WITH_KNOTS('',3,(#20409,#20410,#20411,#20412,#20413,
#20414,#20415,#20416,#20417,#20418,#20419),.UNSPECIFIED.,.F.,.F.,(4,1,1,
1,1,1,1,1,4),(235.619449019236,236.499770298172,237.499258020174,238.498745742176,
238.998489603176,239.498233464177,240.497721186179,241.49720890818,241.902634326415),
 .UNSPECIFIED.);
#522=B_SPLINE_CURVE_WITH_KNOTS('',3,(#20420,#20421,#20422,#20423,#20424,
#20425,#20426,#20427,#20428,#20429,#20430,#20431,#20432,#20433,#20434,#20435,
#20436,#20437,#20438,#20439,#20440,#20441,#20442,#20443,#20444,#20445,#20446,
#20447),.UNSPECIFIED.,.F.,.F.,(4,3,3,3,3,3,3,3,3,4),(235.619449019236,236.403649183285,
237.187849347334,237.972049511383,238.756249675432,239.540449839482,240.324650003531,
241.10885016758,241.893050331629,241.902634326415),.UNSPECIFIED.);
#523=B_SPLINE_CURVE_WITH_KNOTS('',3,(#20452,#20453,#20454,#20455,#20456,
#20457,#20458,#20459,#20460,#20461,#20462,#20463,#20464,#20465,#20466,#20467,
#20468,#20469,#20470,#20471,#20472,#20473,#20474,#20475,#20476,#20477,#20478,
#20479),.UNSPECIFIED.,.F.,.F.,(4,3,3,3,3,3,3,3,3,4),(229.336263712056,230.120463876105,
230.904664040154,231.688864204203,232.473064368253,233.257264532302,234.041464696351,
234.8256648604,235.609865024449,235.619449019236),.UNSPECIFIED.);
#524=B_SPLINE_CURVE_WITH_KNOTS('',3,(#20480,#20481,#20482,#20483,#20484,
#20485,#20486,#20487,#20488,#20489,#20490,#20491,#20492,#20493,#20494,#20495,
#20496,#20497,#20498,#20499,#20500,#20501,#20502,#20503,#20504,#20505,#20506,
#20507),.UNSPECIFIED.,.F.,.F.,(4,3,3,3,3,3,3,3,3,4),(229.336263712056,230.120463876105,
230.904664040155,231.688864204204,232.473064368253,233.257264532302,234.041464696352,
234.825664860401,235.60986502445,235.619449019236),.UNSPECIFIED.);
#525=B_SPLINE_CURVE_WITH_KNOTS('',3,(#20512,#20513,#20514,#20515,#20516,
#20517,#20518,#20519,#20520,#20521,#20522,#20523,#20524,#20525,#20526,#20527,
#20528,#20529,#20530,#20531,#20532,#20533,#20534,#20535,#20536,#20537,#20538,
#20539),.UNSPECIFIED.,.F.,.F.,(4,3,3,3,3,3,3,3,3,4),(223.053078404876,223.837278568926,
224.621478732975,225.405678897024,226.189879061073,226.974079225123,227.758279389172,
228.542479553221,229.32667971727,229.336263712056),.UNSPECIFIED.);
#526=B_SPLINE_CURVE_WITH_KNOTS('',3,(#20540,#20541,#20542,#20543,#20544,
#20545,#20546,#20547,#20548,#20549,#20550,#20551,#20552,#20553,#20554,#20555,
#20556,#20557,#20558,#20559,#20560,#20561,#20562,#20563,#20564,#20565,#20566,
#20567),.UNSPECIFIED.,.F.,.F.,(4,3,3,3,3,3,3,3,3,4),(223.053078404877,223.837278568926,
224.621478732975,225.405678897024,226.189879061073,226.974079225123,227.758279389172,
228.542479553221,229.32667971727,229.336263712056),.UNSPECIFIED.);
#527=B_SPLINE_CURVE_WITH_KNOTS('',3,(#20572,#20573,#20574,#20575,#20576,
#20577,#20578,#20579,#20580,#20581,#20582,#20583,#20584,#20585,#20586,#20587,
#20588,#20589,#20590,#20591,#20592,#20593,#20594,#20595,#20596,#20597,#20598,
#20599),.UNSPECIFIED.,.F.,.F.,(4,3,3,3,3,3,3,3,3,4),(216.769893097697,217.554093261746,
218.338293425795,219.122493589844,219.906693753894,220.690893917943,221.475094081992,
222.259294246041,223.043494410091,223.053078404876),.UNSPECIFIED.);
#528=B_SPLINE_CURVE_WITH_KNOTS('',3,(#20600,#20601,#20602,#20603,#20604,
#20605,#20606,#20607,#20608,#20609,#20610,#20611,#20612,#20613,#20614,#20615,
#20616,#20617,#20618,#20619,#20620,#20621,#20622,#20623,#20624,#20625,#20626,
#20627),.UNSPECIFIED.,.F.,.F.,(4,3,3,3,3,3,3,3,3,4),(216.769893097697,217.554093261746,
218.338293425795,219.122493589845,219.906693753894,220.690893917943,221.475094081992,
222.259294246042,223.043494410091,223.053078404877),.UNSPECIFIED.);
#529=B_SPLINE_CURVE_WITH_KNOTS('',3,(#20632,#20633,#20634,#20635,#20636,
#20637,#20638,#20639,#20640,#20641,#20642,#20643,#20644,#20645,#20646,#20647,
#20648,#20649,#20650,#20651,#20652,#20653,#20654,#20655,#20656,#20657,#20658,
#20659),.UNSPECIFIED.,.F.,.F.,(4,3,3,3,3,3,3,3,3,4),(210.486707790517,211.270907954566,
212.055108118616,212.839308282665,213.623508446714,214.407708610763,215.191908774813,
215.976108938862,216.760309102911,216.769893097697),.UNSPECIFIED.);
#530=B_SPLINE_CURVE_WITH_KNOTS('',3,(#20660,#20661,#20662,#20663,#20664,
#20665,#20666,#20667,#20668,#20669,#20670,#20671,#20672,#20673,#20674,#20675,
#20676,#20677,#20678,#20679,#20680,#20681,#20682,#20683,#20684,#20685,#20686,
#20687),.UNSPECIFIED.,.F.,.F.,(4,3,3,3,3,3,3,3,3,4),(210.486707790517,211.270907954567,
212.055108118616,212.839308282665,213.623508446714,214.407708610764,215.191908774813,
215.976108938862,216.760309102911,216.769893097697),.UNSPECIFIED.);
#531=B_SPLINE_CURVE_WITH_KNOTS('',3,(#20692,#20693,#20694,#20695,#20696,
#20697,#20698,#20699,#20700,#20701),.UNSPECIFIED.,.F.,.F.,(4,1,1,1,1,1,
1,4),(204.203522483338,204.516163194122,205.515650916124,206.515138638125,
207.514626360127,208.514114082129,209.51360180413,210.486707790517),
 .UNSPECIFIED.);
#532=B_SPLINE_CURVE_WITH_KNOTS('',3,(#20702,#20703,#20704,#20705,#20706,
#20707,#20708,#20709,#20710,#20711,#20712,#20713,#20714,#20715,#20716,#20717,
#20718,#20719,#20720,#20721,#20722,#20723,#20724,#20725,#20726,#20727,#20728,
#20729),.UNSPECIFIED.,.F.,.F.,(4,3,3,3,3,3,3,3,3,4),(204.203522483338,204.987722647387,
205.771922811436,206.556122975485,207.340323139535,208.124523303584,208.908723467633,
209.692923631682,210.477123795732,210.486707790517),.UNSPECIFIED.);
#533=B_SPLINE_CURVE_WITH_KNOTS('',3,(#20734,#20735,#20736,#20737,#20738,
#20739,#20740,#20741,#20742,#20743,#20744,#20745,#20746,#20747,#20748,#20749,
#20750,#20751,#20752,#20753,#20754,#20755,#20756,#20757,#20758,#20759,#20760,
#20761),.UNSPECIFIED.,.F.,.F.,(4,3,3,3,3,3,3,3,3,4),(197.920337176158,198.704537340207,
199.488737504256,200.272937668306,201.057137832355,201.841337996404,202.625538160453,
203.409738324502,204.193938488552,204.203522483338),.UNSPECIFIED.);
#534=B_SPLINE_CURVE_WITH_KNOTS('',3,(#20762,#20763,#20764,#20765,#20766,
#20767,#20768,#20769,#20770,#20771,#20772,#20773,#20774,#20775,#20776,#20777,
#20778,#20779,#20780,#20781,#20782,#20783,#20784,#20785,#20786,#20787,#20788,
#20789),.UNSPECIFIED.,.F.,.F.,(4,3,3,3,3,3,3,3,3,4),(197.920337176158,198.704537340207,
199.488737504257,200.272937668306,201.057137832355,201.841337996404,202.625538160453,
203.409738324502,204.193938488552,204.203522483338),.UNSPECIFIED.);
#535=B_SPLINE_CURVE_WITH_KNOTS('',3,(#20794,#20795,#20796,#20797,#20798,
#20799,#20800,#20801,#20802,#20803,#20804),.UNSPECIFIED.,.F.,.F.,(4,1,1,
1,1,1,1,1,4),(191.637151868978,192.522310530103,193.521798252105,194.521285974107,
195.520773696108,196.52026141811,197.020005279111,197.519749140111,197.920337176158),
 .UNSPECIFIED.);
#536=B_SPLINE_CURVE_WITH_KNOTS('',3,(#20805,#20806,#20807,#20808,#20809,
#20810,#20811,#20812,#20813,#20814,#20815,#20816,#20817,#20818,#20819,#20820,
#20821,#20822,#20823,#20824,#20825,#20826,#20827,#20828,#20829,#20830,#20831,
#20832),.UNSPECIFIED.,.F.,.F.,(4,3,3,3,3,3,3,3,3,4),(191.637151868979,192.421352033028,
193.205552197077,193.989752361126,194.773952525176,195.558152689225,196.342352853274,
197.126553017323,197.910753181373,197.920337176158),.UNSPECIFIED.);
#537=B_SPLINE_CURVE_WITH_KNOTS('',3,(#20837,#20838,#20839,#20840,#20841,
#20842,#20843,#20844,#20845,#20846,#20847,#20848,#20849,#20850,#20851,#20852,
#20853,#20854,#20855,#20856,#20857,#20858,#20859,#20860,#20861,#20862,#20863,
#20864),.UNSPECIFIED.,.F.,.F.,(4,3,3,3,3,3,3,3,3,4),(185.353966561799,186.138166725848,
186.922366889897,187.706567053947,188.490767217996,189.274967382045,190.059167546094,
190.843367710144,191.627567874193,191.637151868979),.UNSPECIFIED.);
#538=B_SPLINE_CURVE_WITH_KNOTS('',3,(#20865,#20866,#20867,#20868,#20869,
#20870,#20871,#20872,#20873,#20874,#20875,#20876,#20877,#20878,#20879,#20880,
#20881,#20882,#20883,#20884,#20885,#20886,#20887,#20888,#20889,#20890,#20891,
#20892),.UNSPECIFIED.,.F.,.F.,(4,3,3,3,3,3,3,3,3,4),(185.353966561799,186.138166725848,
186.922366889898,187.706567053947,188.490767217996,189.274967382045,190.059167546095,
190.843367710144,191.627567874193,191.637151868979),.UNSPECIFIED.);
#539=B_SPLINE_CURVE_WITH_KNOTS('',3,(#20897,#20898,#20899,#20900,#20901,
#20902,#20903,#20904,#20905,#20906,#20907,#20908,#20909,#20910,#20911,#20912,
#20913,#20914,#20915,#20916,#20917,#20918,#20919,#20920,#20921,#20922,#20923,
#20924),.UNSPECIFIED.,.F.,.F.,(4,3,3,3,3,3,3,3,3,4),(179.070781254619,179.854981418669,
180.639181582718,181.423381746767,182.207581910816,182.991782074865,183.775982238915,
184.560182402964,185.344382567013,185.353966561799),.UNSPECIFIED.);
#540=B_SPLINE_CURVE_WITH_KNOTS('',3,(#20925,#20926,#20927,#20928,#20929,
#20930,#20931,#20932,#20933,#20934,#20935,#20936,#20937,#20938,#20939,#20940,
#20941,#20942,#20943,#20944,#20945,#20946,#20947,#20948,#20949,#20950,#20951,
#20952),.UNSPECIFIED.,.F.,.F.,(4,3,3,3,3,3,3,3,3,4),(179.07078125462,179.854981418669,
180.639181582718,181.423381746767,182.207581910816,182.991782074865,183.775982238915,
184.560182402964,185.344382567013,185.353966561799),.UNSPECIFIED.);
#541=B_SPLINE_CURVE_WITH_KNOTS('',3,(#20957,#20958,#20959,#20960,#20961,
#20962,#20963,#20964,#20965,#20966,#20967),.UNSPECIFIED.,.F.,.F.,(4,1,1,
1,1,1,1,1,4),(172.78759594744,173.532043812074,174.531531534075,175.531019256077,
176.030763117078,176.530506978078,177.52999470008,178.529482422082,179.070781254619),
 .UNSPECIFIED.);
#542=B_SPLINE_CURVE_WITH_KNOTS('',3,(#20968,#20969,#20970,#20971,#20972,
#20973,#20974,#20975,#20976,#20977,#20978,#20979,#20980,#20981,#20982,#20983,
#20984,#20985,#20986,#20987,#20988,#20989,#20990,#20991,#20992,#20993,#20994,
#20995),.UNSPECIFIED.,.F.,.F.,(4,3,3,3,3,3,3,3,3,4),(172.78759594744,173.571796111489,
174.355996275539,175.140196439588,175.924396603637,176.708596767686,177.492796931735,
178.276997095785,179.061197259834,179.07078125462),.UNSPECIFIED.);
#543=B_SPLINE_CURVE_WITH_KNOTS('',3,(#21000,#21001,#21002,#21003,#21004,
#21005,#21006,#21007,#21008,#21009,#21010,#21011),.UNSPECIFIED.,.F.,.F.,
(4,1,1,1,1,1,1,1,1,4),(166.50441064026,166.535629758063,167.535117480064,
168.534605202066,169.034349063067,169.534092924067,170.533580646069,171.533068368071,
172.532556090072,172.78759594744),.UNSPECIFIED.);
#544=B_SPLINE_CURVE_WITH_KNOTS('',3,(#21012,#21013,#21014,#21015,#21016,
#21017,#21018,#21019,#21020,#21021,#21022,#21023,#21024,#21025,#21026,#21027,
#21028,#21029,#21030,#21031,#21032,#21033,#21034,#21035,#21036,#21037,#21038,
#21039),.UNSPECIFIED.,.F.,.F.,(4,3,3,3,3,3,3,3,3,4),(166.50441064026,167.28861080431,
168.072810968359,168.857011132408,169.641211296457,170.425411460506,171.209611624556,
171.993811788605,172.778011952654,172.78759594744),.UNSPECIFIED.);
#545=B_SPLINE_CURVE_WITH_KNOTS('',3,(#21044,#21045,#21046,#21047,#21048,
#21049,#21050,#21051,#21052,#21053,#21054,#21055,#21056,#21057,#21058,#21059,
#21060,#21061,#21062,#21063,#21064,#21065,#21066,#21067,#21068,#21069,#21070,
#21071),.UNSPECIFIED.,.F.,.F.,(4,3,3,3,3,3,3,3,3,4),(160.221225333081,161.00542549713,
161.789625661179,162.573825825228,163.358025989277,164.142226153327,164.926426317376,
165.710626481425,166.494826645474,166.50441064026),.UNSPECIFIED.);
#546=B_SPLINE_CURVE_WITH_KNOTS('',3,(#21072,#21073,#21074,#21075,#21076,
#21077,#21078,#21079,#21080,#21081,#21082,#21083,#21084,#21085,#21086,#21087,
#21088,#21089,#21090,#21091,#21092,#21093,#21094,#21095,#21096,#21097,#21098,
#21099),.UNSPECIFIED.,.F.,.F.,(4,3,3,3,3,3,3,3,3,4),(160.221225333081,161.00542549713,
161.789625661179,162.573825825229,163.358025989278,164.142226153327,164.926426317376,
165.710626481425,166.494826645475,166.50441064026),.UNSPECIFIED.);
#547=B_SPLINE_CURVE_WITH_KNOTS('',3,(#21104,#21105,#21106,#21107,#21108,
#21109,#21110,#21111,#21112,#21113,#21114,#21115,#21116,#21117,#21118,#21119,
#21120,#21121,#21122,#21123,#21124,#21125,#21126,#21127,#21128,#21129,#21130,
#21131),.UNSPECIFIED.,.F.,.F.,(4,3,3,3,3,3,3,3,3,4),(153.938040025901,154.72224018995,
155.506440354,156.290640518049,157.074840682098,157.859040846147,158.643241010196,
159.427441174246,160.211641338295,160.221225333081),.UNSPECIFIED.);
#548=B_SPLINE_CURVE_WITH_KNOTS('',3,(#21132,#21133,#21134,#21135,#21136,
#21137,#21138,#21139,#21140,#21141,#21142,#21143,#21144,#21145,#21146,#21147,
#21148,#21149,#21150,#21151,#21152,#21153,#21154,#21155,#21156,#21157,#21158,
#21159),.UNSPECIFIED.,.F.,.F.,(4,3,3,3,3,3,3,3,3,4),(153.938040025901,154.722240189951,
155.506440354,156.290640518049,157.074840682098,157.859040846147,158.643241010197,
159.427441174246,160.211641338295,160.221225333081),.UNSPECIFIED.);
#549=B_SPLINE_CURVE_WITH_KNOTS('',3,(#21164,#21165,#21166,#21167,#21168,
#21169,#21170,#21171,#21172,#21173,#21174),.UNSPECIFIED.,.F.,.F.,(4,1,1,
1,1,1,1,1,4),(147.654854718722,148.045106901034,148.544850762035,149.544338484036,
150.543826206038,151.543313928039,152.542801650041,153.542289372042,153.938040025901),
 .UNSPECIFIED.);
#550=B_SPLINE_CURVE_WITH_KNOTS('',3,(#21175,#21176,#21177,#21178,#21179,
#21180,#21181,#21182,#21183,#21184,#21185,#21186,#21187,#21188,#21189,#21190,
#21191,#21192,#21193,#21194,#21195,#21196,#21197,#21198,#21199,#21200,#21201,
#21202),.UNSPECIFIED.,.F.,.F.,(4,3,3,3,3,3,3,3,3,4),(147.654854718722,148.439054882771,
149.22325504682,150.007455210869,150.791655374919,151.575855538968,152.360055703017,
153.144255867066,153.928456031116,153.938040025901),.UNSPECIFIED.);
#551=B_SPLINE_CURVE_WITH_KNOTS('',3,(#21207,#21208,#21209,#21210,#21211,
#21212,#21213,#21214,#21215,#21216,#21217,#21218,#21219,#21220,#21221,#21222,
#21223,#21224,#21225,#21226,#21227,#21228,#21229,#21230,#21231,#21232,#21233,
#21234),.UNSPECIFIED.,.F.,.F.,(4,3,3,3,3,3,3,3,3,4),(141.371669411542,142.155869575591,
142.94006973964,143.72426990369,144.508470067739,145.292670231788,146.076870395837,
146.861070559887,147.645270723936,147.654854718722),.UNSPECIFIED.);
#552=B_SPLINE_CURVE_WITH_KNOTS('',3,(#21235,#21236,#21237,#21238,#21239,
#21240,#21241,#21242,#21243,#21244,#21245),.UNSPECIFIED.,.F.,.F.,(4,1,1,
1,1,1,1,1,4),(141.371669411542,142.230670203473,143.230157925475,144.229645647477,
144.729389508477,145.229133369478,146.22862109148,147.228108813481,147.654854718722),
 .UNSPECIFIED.);
#553=B_SPLINE_CURVE_WITH_KNOTS('',3,(#21250,#21251,#21252,#21253,#21254,
#21255,#21256,#21257,#21258,#21259,#21260,#21261,#21262,#21263,#21264,#21265,
#21266,#21267,#21268,#21269,#21270,#21271,#21272,#21273,#21274,#21275,#21276,
#21277),.UNSPECIFIED.,.F.,.F.,(4,3,3,3,3,3,3,3,3,4),(135.088484104362,135.872684268412,
136.656884432461,137.44108459651,138.225284760559,139.009484924609,139.793685088658,
140.577885252707,141.362085416756,141.371669411542),.UNSPECIFIED.);
#554=B_SPLINE_CURVE_WITH_KNOTS('',3,(#21278,#21279,#21280,#21281,#21282,
#21283,#21284,#21285,#21286,#21287,#21288,#21289,#21290,#21291,#21292,#21293,
#21294,#21295,#21296,#21297,#21298,#21299,#21300,#21301,#21302,#21303,#21304,
#21305),.UNSPECIFIED.,.F.,.F.,(4,3,3,3,3,3,3,3,3,4),(135.088484104363,135.872684268412,
136.656884432461,137.44108459651,138.225284760559,139.009484924609,139.793685088658,
140.577885252707,141.362085416756,141.371669411542),.UNSPECIFIED.);
#555=B_SPLINE_CURVE_WITH_KNOTS('',3,(#21310,#21311,#21312,#21313,#21314,
#21315,#21316,#21317,#21318,#21319,#21320,#21321,#21322,#21323,#21324,#21325,
#21326,#21327,#21328,#21329,#21330,#21331,#21332,#21333,#21334,#21335,#21336,
#21337),.UNSPECIFIED.,.F.,.F.,(4,3,3,3,3,3,3,3,3,4),(128.805298797183,129.589498961232,
130.373699125281,131.15789928933,131.94209945338,132.726299617429,133.510499781478,
134.294699945527,135.078900109576,135.088484104362),.UNSPECIFIED.);
#556=B_SPLINE_CURVE_WITH_KNOTS('',3,(#21338,#21339,#21340,#21341,#21342,
#21343,#21344,#21345,#21346,#21347,#21348,#21349,#21350,#21351,#21352,#21353,
#21354,#21355,#21356,#21357,#21358,#21359,#21360,#21361,#21362,#21363,#21364,
#21365),.UNSPECIFIED.,.F.,.F.,(4,3,3,3,3,3,3,3,3,4),(128.805298797183,129.589498961232,
130.373699125281,131.157899289331,131.94209945338,132.726299617429,133.510499781478,
134.294699945527,135.078900109576,135.088484104363),.UNSPECIFIED.);
#557=B_SPLINE_CURVE_WITH_KNOTS('',3,(#21370,#21371,#21372,#21373,#21374,
#21375,#21376,#21377,#21378,#21379,#21380,#21381,#21382,#21383,#21384,#21385,
#21386,#21387,#21388,#21389,#21390,#21391,#21392,#21393,#21394,#21395,#21396,
#21397),.UNSPECIFIED.,.F.,.F.,(4,3,3,3,3,3,3,3,3,4),(122.522113490003,123.306313654053,
124.090513818102,124.874713982151,125.6589141462,126.443114310249,127.227314474299,
128.011514638348,128.795714802397,128.805298797183),.UNSPECIFIED.);
#558=B_SPLINE_CURVE_WITH_KNOTS('',3,(#21398,#21399,#21400,#21401,#21402,
#21403,#21404,#21405,#21406,#21407,#21408,#21409,#21410,#21411,#21412,#21413,
#21414,#21415,#21416,#21417,#21418,#21419,#21420,#21421,#21422,#21423,#21424,
#21425),.UNSPECIFIED.,.F.,.F.,(4,3,3,3,3,3,3,3,3,4),(122.522113490004,123.306313654053,
124.090513818102,124.874713982151,125.6589141462,126.44311431025,127.227314474299,
128.011514638348,128.795714802397,128.805298797183),.UNSPECIFIED.);
#559=B_SPLINE_CURVE_WITH_KNOTS('',3,(#21430,#21431,#21432,#21433,#21434,
#21435,#21436,#21437,#21438,#21439,#21440),.UNSPECIFIED.,.F.,.F.,(4,1,1,
1,1,1,1,1,4),(116.238928182824,116.561243657984,117.560731379986,118.560219101987,
119.559706823989,120.05945068499,120.559194545991,121.558682267992,122.522113490003),
 .UNSPECIFIED.);
#560=B_SPLINE_CURVE_WITH_KNOTS('',3,(#21441,#21442,#21443,#21444,#21445,
#21446,#21447,#21448,#21449,#21450,#21451,#21452,#21453,#21454,#21455,#21456,
#21457,#21458,#21459,#21460,#21461,#21462,#21463,#21464,#21465,#21466,#21467,
#21468),.UNSPECIFIED.,.F.,.F.,(4,3,3,3,3,3,3,3,3,4),(116.238928182824,117.023128346873,
117.807328510922,118.591528674972,119.375728839021,120.15992900307,120.944129167119,
121.728329331169,122.512529495218,122.522113490004),.UNSPECIFIED.);
#561=B_SPLINE_CURVE_WITH_KNOTS('',3,(#21473,#21474,#21475,#21476,#21477,
#21478,#21479,#21480,#21481,#21482,#21483),.UNSPECIFIED.,.F.,.F.,(4,1,1,
1,1,1,1,1,4),(109.955742875644,110.564317325975,111.563805047977,112.563292769978,
113.063036630979,113.56278049198,114.562268213981,115.561755935983,116.238928182824),
 .UNSPECIFIED.);
#562=B_SPLINE_CURVE_WITH_KNOTS('',3,(#21484,#21485,#21486,#21487,#21488,
#21489,#21490,#21491,#21492,#21493,#21494,#21495,#21496,#21497,#21498,#21499,
#21500,#21501,#21502,#21503,#21504,#21505,#21506,#21507,#21508,#21509,#21510,
#21511),.UNSPECIFIED.,.F.,.F.,(4,3,3,3,3,3,3,3,3,4),(109.955742875644,110.739943039694,
111.524143203743,112.308343367792,113.092543531841,113.87674369589,114.66094385994,
115.445144023989,116.229344188038,116.238928182824),.UNSPECIFIED.);
#563=B_SPLINE_CURVE_WITH_KNOTS('',3,(#21516,#21517,#21518,#21519,#21520,
#21521,#21522,#21523,#21524,#21525,#21526,#21527,#21528,#21529,#21530,#21531,
#21532,#21533,#21534,#21535,#21536,#21537,#21538,#21539,#21540,#21541,#21542,
#21543),.UNSPECIFIED.,.F.,.F.,(4,3,3,3,3,3,3,3,3,4),(103.672557568465,104.456757732514,
105.240957896563,106.025158060612,106.809358224661,107.593558388711,108.37775855276,
109.161958716809,109.946158880858,109.955742875644),.UNSPECIFIED.);
#564=B_SPLINE_CURVE_WITH_KNOTS('',3,(#21544,#21545,#21546,#21547,#21548,
#21549,#21550,#21551,#21552,#21553,#21554,#21555,#21556,#21557,#21558,#21559,
#21560,#21561,#21562,#21563,#21564,#21565,#21566,#21567,#21568,#21569,#21570,
#21571),.UNSPECIFIED.,.F.,.F.,(4,3,3,3,3,3,3,3,3,4),(103.672557568465,104.456757732514,
105.240957896563,106.025158060612,106.809358224662,107.593558388711,108.37775855276,
109.161958716809,109.946158880859,109.955742875644),.UNSPECIFIED.);
#565=B_SPLINE_CURVE_WITH_KNOTS('',3,(#21576,#21577,#21578,#21579,#21580,
#21581,#21582,#21583,#21584,#21585,#21586,#21587,#21588,#21589,#21590,#21591,
#21592,#21593,#21594,#21595,#21596,#21597,#21598,#21599,#21600,#21601,#21602,
#21603),.UNSPECIFIED.,.F.,.F.,(4,3,3,3,3,3,3,3,3,4),(97.3893722612849,98.1735724253341,
98.9577725893833,99.7419727534325,100.526172917482,101.310373081531,102.09457324558,
102.878773409629,103.662973573678,103.672557568465),.UNSPECIFIED.);
#566=B_SPLINE_CURVE_WITH_KNOTS('',3,(#21604,#21605,#21606,#21607,#21608,
#21609,#21610,#21611,#21612,#21613,#21614,#21615,#21616,#21617,#21618,#21619,
#21620,#21621,#21622,#21623,#21624,#21625,#21626,#21627,#21628,#21629,#21630,
#21631),.UNSPECIFIED.,.F.,.F.,(4,3,3,3,3,3,3,3,3,4),(97.3893722612851,98.1735724253344,
98.9577725893836,99.7419727534328,100.526172917482,101.310373081531,102.09457324558,
102.87877340963,103.662973573679,103.672557568465),.UNSPECIFIED.);
#567=B_SPLINE_CURVE_WITH_KNOTS('',3,(#21636,#21637,#21638,#21639,#21640,
#21641,#21642,#21643,#21644,#21645,#21646,#21647,#21648,#21649,#21650,#21651,
#21652,#21653,#21654,#21655,#21656,#21657,#21658,#21659,#21660,#21661,#21662,
#21663),.UNSPECIFIED.,.F.,.F.,(4,3,3,3,3,3,3,3,3,4),(91.1061869541053,91.8903871181545,
92.6745872822037,93.458787446253,94.2429876103022,95.0271877743514,95.8113879384006,
96.5955881024498,97.379788266499,97.3893722612849),.UNSPECIFIED.);
#568=B_SPLINE_CURVE_WITH_KNOTS('',3,(#21664,#21665,#21666,#21667,#21668,
#21669,#21670,#21671,#21672,#21673,#21674,#21675,#21676,#21677,#21678,#21679,
#21680,#21681,#21682,#21683,#21684,#21685,#21686,#21687,#21688,#21689,#21690,
#21691),.UNSPECIFIED.,.F.,.F.,(4,3,3,3,3,3,3,3,3,4),(91.1061869541056,91.8903871181548,
92.674587282204,93.4587874462532,94.2429876103025,95.0271877743517,95.8113879384009,
96.5955881024501,97.3797882664994,97.3893722612851),.UNSPECIFIED.);
#569=B_SPLINE_CURVE_WITH_KNOTS('',3,(#21696,#21697,#21698,#21699,#21700,
#21701,#21702,#21703,#21704,#21705,#21706,#21707,#21708,#21709,#21710,#21711,
#21712,#21713,#21714,#21715,#21716,#21717,#21718,#21719,#21720,#21721,#21722,
#21723),.UNSPECIFIED.,.F.,.F.,(4,3,3,3,3,3,3,3,3,4),(84.8230016469257,85.6072018109749,
86.3914019750241,87.1756021390733,87.9598023031225,88.7440024671717,89.5282026312209,
90.3124027952701,91.0966029593193,91.1061869541053),.UNSPECIFIED.);
#570=B_SPLINE_CURVE_WITH_KNOTS('',3,(#21724,#21725,#21726,#21727,#21728,
#21729,#21730,#21731,#21732,#21733,#21734,#21735,#21736,#21737,#21738,#21739,
#21740,#21741,#21742,#21743,#21744,#21745,#21746,#21747,#21748,#21749,#21750,
#21751),.UNSPECIFIED.,.F.,.F.,(4,3,3,3,3,3,3,3,3,4),(84.823001646926,85.6072018109752,
86.3914019750244,87.1756021390736,87.9598023031228,88.744002467172,89.5282026312212,
90.3124027952704,91.0966029593196,91.1061869541056),.UNSPECIFIED.);
#571=B_SPLINE_CURVE_WITH_KNOTS('',3,(#21756,#21757,#21758,#21759,#21760,
#21761,#21762,#21763,#21764,#21765,#21766,#21767,#21768,#21769,#21770,#21771,
#21772,#21773,#21774,#21775,#21776,#21777,#21778,#21779,#21780,#21781,#21782,
#21783),.UNSPECIFIED.,.F.,.F.,(4,3,3,3,3,3,3,3,3,4),(78.5398163397462,79.3240165037953,
80.1082166678445,80.8924168318937,81.6766169959429,82.4608171599921,83.2450173240413,
84.0292174880905,84.8134176521397,84.8230016469257),.UNSPECIFIED.);
#572=B_SPLINE_CURVE_WITH_KNOTS('',3,(#21784,#21785,#21786,#21787,#21788,
#21789,#21790,#21791,#21792,#21793,#21794),.UNSPECIFIED.,.F.,.F.,(4,1,1,
1,1,1,1,1,4),(78.5398163397464,79.2629437173746,80.2624314393762,81.2619191613777,
81.7616630223785,82.2614068833793,83.2608946053809,84.2603823273824,84.823001646926),
 .UNSPECIFIED.);
#573=B_SPLINE_CURVE_WITH_KNOTS('',3,(#21799,#21800,#21801,#21802,#21803,
#21804,#21805,#21806,#21807,#21808,#21809),.UNSPECIFIED.,.F.,.F.,(4,1,1,
1,1,1,1,1,4),(72.2566310325665,72.5837838899154,73.583271611917,74.5827593339185,
75.5822470559201,76.5817347779217,77.5812224999232,78.080966360924,78.5398163397462),
 .UNSPECIFIED.);
#574=B_SPLINE_CURVE_WITH_KNOTS('',3,(#21810,#21811,#21812,#21813,#21814,
#21815,#21816,#21817,#21818,#21819,#21820,#21821),.UNSPECIFIED.,.F.,.F.,
(4,1,1,1,1,1,1,1,1,4),(72.2566310325668,72.2665296633636,73.2660173853652,
74.2655051073667,74.7652489683675,75.2649928293683,76.2644805513699,77.2639682733715,
78.263455995373,78.5398163397464),.UNSPECIFIED.);
#575=B_SPLINE_CURVE_WITH_KNOTS('',3,(#21826,#21827,#21828,#21829,#21830,
#21831,#21832,#21833,#21834,#21835,#21836,#21837,#21838,#21839,#21840,#21841,
#21842,#21843,#21844,#21845,#21846,#21847,#21848,#21849,#21850,#21851,#21852,
#21853),.UNSPECIFIED.,.F.,.F.,(4,3,3,3,3,3,3,3,3,4),(65.973445725387,66.7576458894362,
67.5418460534854,68.3260462175346,69.1102463815837,69.8944465456329,70.6786467096821,
71.4628468737313,72.2470470377805,72.2566310325665),.UNSPECIFIED.);
#576=B_SPLINE_CURVE_WITH_KNOTS('',3,(#21854,#21855,#21856,#21857,#21858,
#21859,#21860,#21861,#21862,#21863,#21864,#21865,#21866,#21867,#21868,#21869,
#21870,#21871,#21872,#21873,#21874,#21875,#21876,#21877,#21878,#21879,#21880,
#21881),.UNSPECIFIED.,.F.,.F.,(4,3,3,3,3,3,3,3,3,4),(65.9734457253872,66.7576458894364,
67.5418460534856,68.3260462175348,69.110246381584,69.8944465456332,70.6786467096824,
71.4628468737316,72.2470470377808,72.2566310325668),.UNSPECIFIED.);
#577=B_SPLINE_CURVE_WITH_KNOTS('',3,(#21886,#21887,#21888,#21889,#21890,
#21891,#21892,#21893,#21894,#21895,#21896),.UNSPECIFIED.,.F.,.F.,(4,1,1,
1,1,1,1,1,4),(59.6902604182074,60.5899312258966,61.5894189478982,62.5889066698997,
63.5883943919013,64.0881382529021,64.5878821139029,65.5873698359044,65.973445725387),
 .UNSPECIFIED.);
#578=B_SPLINE_CURVE_WITH_KNOTS('',3,(#21897,#21898,#21899,#21900,#21901,
#21902,#21903,#21904,#21905,#21906,#21907,#21908,#21909,#21910,#21911,#21912,
#21913,#21914,#21915,#21916,#21917,#21918,#21919,#21920,#21921,#21922,#21923,
#21924),.UNSPECIFIED.,.F.,.F.,(4,3,3,3,3,3,3,3,3,4),(59.6902604182076,60.4744605822568,
61.258660746306,62.0428609103552,62.8270610744044,63.6112612384536,64.3954614025028,
65.179661566552,65.9638617306012,65.9734457253872),.UNSPECIFIED.);
#579=B_SPLINE_CURVE_WITH_KNOTS('',3,(#21929,#21930,#21931,#21932,#21933,
#21934,#21935,#21936,#21937,#21938,#21939,#21940,#21941,#21942,#21943,#21944,
#21945,#21946,#21947,#21948,#21949,#21950,#21951,#21952,#21953,#21954,#21955,
#21956),.UNSPECIFIED.,.F.,.F.,(4,3,3,3,3,3,3,3,3,4),(53.4070751110278,54.191275275077,
54.9754754391262,55.7596756031754,56.5438757672245,57.3280759312737,58.1122760953229,
58.8964762593721,59.6806764234213,59.6902604182074),.UNSPECIFIED.);
#580=B_SPLINE_CURVE_WITH_KNOTS('',3,(#21957,#21958,#21959,#21960,#21961,
#21962,#21963,#21964,#21965,#21966,#21967),.UNSPECIFIED.,.F.,.F.,(4,1,1,
1,1,1,1,1,4),(53.407075111028,53.7760068063346,54.2757506673354,55.275238389337,
56.2747261113385,57.2742138333401,58.2737015553417,59.2731892773432,59.6902604182076),
 .UNSPECIFIED.);
#581=B_SPLINE_CURVE_WITH_KNOTS('',3,(#21972,#21973,#21974,#21975,#21976,
#21977,#21978,#21979,#21980,#21981,#21982),.UNSPECIFIED.,.F.,.F.,(4,1,1,
1,1,1,1,1,4),(47.1238898038482,47.5965908398762,48.5960785618778,49.5955662838794,
50.0953101448802,50.5950540058809,51.5945417278825,52.5940294498841,53.4070751110278),
 .UNSPECIFIED.);
#582=B_SPLINE_CURVE_WITH_KNOTS('',3,(#21983,#21984,#21985,#21986,#21987,
#21988,#21989,#21990,#21991,#21992,#21993,#21994,#21995,#21996,#21997,#21998,
#21999,#22000,#22001,#22002,#22003,#22004,#22005,#22006,#22007,#22008,#22009,
#22010),.UNSPECIFIED.,.F.,.F.,(4,3,3,3,3,3,3,3,3,4),(47.1238898038484,47.9080899678976,
48.6922901319468,49.4764902959961,50.2606904600453,51.0448906240945,51.8290907881437,
52.6132909521929,53.3974911162422,53.407075111028),.UNSPECIFIED.);
#583=B_SPLINE_CURVE_WITH_KNOTS('',3,(#22015,#22016,#22017,#22018,#22019,
#22020,#22021,#22022,#22023,#22024,#22025,#22026,#22027,#22028,#22029,#22030,
#22031,#22032,#22033,#22034,#22035,#22036,#22037,#22038,#22039,#22040,#22041,
#22042),.UNSPECIFIED.,.F.,.F.,(4,3,3,3,3,3,3,3,3,4),(40.8407044966686,41.6249046607178,
42.409104824767,43.1933049888162,43.9775051528655,44.7617053169147,45.5459054809639,
46.3301056450131,47.1143058090623,47.1238898038482),.UNSPECIFIED.);
#584=B_SPLINE_CURVE_WITH_KNOTS('',3,(#22043,#22044,#22045,#22046,#22047,
#22048,#22049,#22050,#22051,#22052,#22053),.UNSPECIFIED.,.F.,.F.,(4,1,1,
1,1,1,1,1,4),(40.8407044966688,41.282410281315,42.2818980033166,43.2813857253182,
44.2808734473197,45.2803611693213,46.2798488913229,46.7795927523237,47.1238898038484),
 .UNSPECIFIED.);
#585=B_SPLINE_CURVE_WITH_KNOTS('',3,(#22058,#22059,#22060,#22061,#22062,
#22063,#22064,#22065,#22066,#22067,#22068,#22069,#22070,#22071,#22072,#22073,
#22074,#22075,#22076,#22077,#22078,#22079,#22080,#22081,#22082,#22083,#22084,
#22085),.UNSPECIFIED.,.F.,.F.,(4,3,3,3,3,3,3,3,3,4),(34.557519189489,35.3417193535382,
36.1259195175874,36.9101196816366,37.6943198456858,38.478520009735,39.2627201737842,
40.0469203378334,40.8311205018826,40.8407044966686),.UNSPECIFIED.);
#586=B_SPLINE_CURVE_WITH_KNOTS('',3,(#22086,#22087,#22088,#22089,#22090,
#22091,#22092,#22093,#22094,#22095,#22096,#22097,#22098,#22099,#22100,#22101,
#22102,#22103,#22104,#22105,#22106,#22107,#22108,#22109,#22110,#22111,#22112,
#22113),.UNSPECIFIED.,.F.,.F.,(4,3,3,3,3,3,3,3,3,4),(34.5575191894892,35.3417193535384,
36.1259195175876,36.9101196816368,37.694319845686,38.4785200097352,39.2627201737844,
40.0469203378336,40.8311205018828,40.8407044966688),.UNSPECIFIED.);
#587=B_SPLINE_CURVE_WITH_KNOTS('',3,(#22118,#22119,#22120,#22121,#22122,
#22123,#22124,#22125,#22126,#22127,#22128,#22129,#22130,#22131,#22132,#22133,
#22134,#22135,#22136,#22137,#22138,#22139,#22140,#22141,#22142,#22143,#22144,
#22145),.UNSPECIFIED.,.F.,.F.,(4,3,3,3,3,3,3,3,3,4),(28.2743338823094,29.0585340463586,
29.8427342104078,30.6269343744571,31.4111345385063,32.1953347025555,32.9795348666047,
33.7637350306539,34.5479351947031,34.557519189489),.UNSPECIFIED.);
#588=B_SPLINE_CURVE_WITH_KNOTS('',3,(#22146,#22147,#22148,#22149,#22150,
#22151,#22152,#22153,#22154,#22155,#22156,#22157,#22158,#22159,#22160,#22161,
#22162,#22163,#22164,#22165,#22166,#22167,#22168,#22169,#22170,#22171,#22172,
#22173),.UNSPECIFIED.,.F.,.F.,(4,3,3,3,3,3,3,3,3,4),(28.2743338823096,29.0585340463588,
29.842734210408,30.6269343744572,31.4111345385064,32.1953347025557,32.9795348666049,
33.7637350306541,34.5479351947033,34.5575191894892),.UNSPECIFIED.);
#589=B_SPLINE_CURVE_WITH_KNOTS('',3,(#22178,#22179,#22180,#22181,#22182,
#22183,#22184,#22185,#22186,#22187,#22188,#22189,#22190,#22191,#22192,#22193,
#22194,#22195,#22196,#22197,#22198,#22199,#22200,#22201,#22202,#22203,#22204,
#22205),.UNSPECIFIED.,.F.,.F.,(4,3,3,3,3,3,3,3,3,4),(21.9911485751298,22.775348739179,
23.5595489032282,24.3437490672774,25.1279492313266,25.9121493953758,26.696349559425,
27.4805497234742,28.2647498875234,28.2743338823094),.UNSPECIFIED.);
#590=B_SPLINE_CURVE_WITH_KNOTS('',3,(#22206,#22207,#22208,#22209,#22210,
#22211,#22212,#22213,#22214,#22215,#22216),.UNSPECIFIED.,.F.,.F.,(4,1,1,
1,1,1,1,1,4),(21.99114857513,22.2921435632852,23.2916312852868,24.2911190072884,
25.2906067292899,25.7903505902907,26.2900944512915,27.2895821732931,28.2743338823096),
 .UNSPECIFIED.);
#591=B_SPLINE_CURVE_WITH_KNOTS('',3,(#22221,#22222,#22223,#22224,#22225,
#22226,#22227,#22228,#22229,#22230,#22231),.UNSPECIFIED.,.F.,.F.,(4,1,1,
1,1,1,1,1,4),(15.7079632679502,16.1127275968269,16.6124714578277,17.6119591798292,
18.6114469018308,19.6109346238324,20.6104223458339,21.6099100678355,21.9911485751298),
 .UNSPECIFIED.);
#592=B_SPLINE_CURVE_WITH_KNOTS('',3,(#22232,#22233,#22234,#22235,#22236,
#22237,#22238,#22239,#22240,#22241,#22242),.UNSPECIFIED.,.F.,.F.,(4,1,1,
1,1,1,1,1,4),(15.7079632679505,16.2952172312758,17.2947049532774,18.294192675279,
18.7939365362798,19.2936803972805,20.2931681192821,21.2926558412837,21.99114857513),
 .UNSPECIFIED.);
#593=B_SPLINE_CURVE_WITH_KNOTS('',3,(#22283,#22284,#22285,#22286,#22287,
#22288,#22289,#22290,#22291,#22292,#22293,#22294,#22295,#22296),
 .UNSPECIFIED.,.F.,.F.,(4,2,2,2,2,2,4),(0.,0.401864562314507,0.815996863195449,
1.24239114437787,1.68104169475581,1.98676350350074,2.29817876007995),
 .UNSPECIFIED.);
#594=B_SPLINE_CURVE_WITH_KNOTS('',3,(#22298,#22299,#22300,#22301,#22302,
#22303,#22304,#22305,#22306,#22307,#22308,#22309,#22310,#22311,#22312,#22313,
#22314,#22315,#22316,#22317,#22318,#22319,#22320,#22321,#22322,#22323,#22324,
#22325,#22326,#22327,#22328,#22329,#22330,#22331,#22332,#22333,#22334,#22335,
#22336,#22337,#22338,#22339,#22340,#22341,#22342,#22343,#22344,#22345,#22346,
#22347,#22348,#22349,#22350,#22351,#22352,#22353,#22354,#22355,#22356,#22357,
#22358,#22359,#22360,#22361,#22362,#22363,#22364,#22365,#22366,#22367,#22368,
#22369,#22370,#22371,#22372,#22373,#22374,#22375,#22376,#22377,#22378,#22379),
 .UNSPECIFIED.,.F.,.F.,(4,3,3,3,3,3,3,3,3,3,3,3,3,3,3,3,3,3,3,3,3,3,3,3,
3,3,3,4),(0.,0.0926102951683523,0.242481898243462,0.367224141810497,0.42570459697912,
0.455719969557024,0.483685835042882,0.631460986432984,0.783700701519674,
0.853497497696487,0.898154331254642,0.927522777398727,1.07095818631111,
1.21012247382799,1.24041984677974,1.31315875852148,1.35313933924437,1.49322196341175,
1.63841202124878,1.7110070501673,1.74549420777844,1.77435553121022,1.78360207908582,
1.91413601045329,2.0238902612264,2.05537001599445,2.18951620872001,2.3057378045557),
 .UNSPECIFIED.);
#595=B_SPLINE_CURVE_WITH_KNOTS('',3,(#25115,#25116,#25117,#25118,#25119,
#25120,#25121,#25122,#25123,#25124,#25125,#25126,#25127,#25128,#25129,#25130,
#25131,#25132,#25133,#25134,#25135,#25136,#25137,#25138,#25139,#25140,#25141,
#25142,#25143,#25144,#25145,#25146,#25147,#25148,#25149,#25150,#25151,#25152,
#25153,#25154,#25155,#25156,#25157,#25158,#25159,#25160,#25161,#25162,#25163,
#25164,#25165,#25166,#25167,#25168,#25169,#25170,#25171,#25172,#25173,#25174,
#25175,#25176,#25177,#25178,#25179,#25180,#25181,#25182,#25183,#25184,#25185,
#25186,#25187,#25188,#25189,#25190,#25191,#25192,#25193,#25194,#25195,#25196),
 .UNSPECIFIED.,.F.,.F.,(4,3,3,3,3,3,3,3,3,3,3,3,3,3,3,3,3,3,3,3,3,3,3,3,
3,3,3,4),(0.,0.0926102951686331,0.242481898248882,0.367224141815228,0.425704596969164,
0.455719969047205,0.48368583491359,0.631460986269685,0.783700701397176,
0.853497497532231,0.898154330267531,0.92752277734915,1.07095818632606,1.21012247381061,
1.24041984677965,1.31315875851436,1.35313933832513,1.49322196246626,1.63841202077606,
1.71100704993096,1.74549420694238,1.77435553196361,1.78360207908585,1.9141360104532,
2.02389026119983,2.05537001679799,2.18951620952033,2.30573780455522),
 .UNSPECIFIED.);
#596=B_SPLINE_CURVE_WITH_KNOTS('',3,(#25197,#25198,#25199,#25200,#25201,
#25202,#25203,#25204,#25205,#25206,#25207,#25208,#25209,#25210,#25211,#25212,
#25213,#25214,#25215,#25216,#25217,#25218),.UNSPECIFIED.,.F.,.F.,(4,3,3,
3,3,3,3,4),(585.461696073209,585.699805092919,586.69929281492,587.698780536922,
588.198524397923,588.698268258924,589.697755980925,590.619418874881),
 .UNSPECIFIED.);
#597=B_SPLINE_CURVE_WITH_KNOTS('',3,(#25219,#25220,#25221,#25222,#25223,
#25224,#25225,#25226,#25227,#25228),.UNSPECIFIED.,.F.,.F.,(4,1,1,1,1,1,
1,4),(10.3761157273117,11.297778621268,12.2972663432696,12.7970102042703,
13.2967540652711,14.2962417872727,15.2957295092743,15.7079632679505),
 .UNSPECIFIED.);
#598=B_SPLINE_CURVE_WITH_KNOTS('',3,(#25230,#25231,#25232,#25233,#25234,
#25235,#25236,#25237,#25238,#25239,#25240,#25241,#25242,#25243,#25244,#25245,
#25246,#25247,#25248),.UNSPECIFIED.,.F.,.F.,(4,3,3,3,3,3,4),(11.6150328478198,
12.399233011869,13.1834331759182,13.9676333399674,14.7518335040166,15.5360336680658,
15.7079632679502),.UNSPECIFIED.);
#599=B_SPLINE_CURVE_WITH_KNOTS('',3,(#27978,#27979,#27980,#27981,#27982,
#27983,#27984,#27985,#27986,#27987,#27988,#27989,#27990,#27991),
 .UNSPECIFIED.,.F.,.F.,(4,2,2,2,2,2,4),(0.,0.401864562314452,0.815996863195417,
1.2423911443779,1.68104169475587,1.98676350350112,2.29817876008015),
 .UNSPECIFIED.);
#600=B_SPLINE_CURVE_WITH_KNOTS('',3,(#27992,#27993,#27994,#27995,#27996,
#27997,#27998,#27999,#28000,#28001,#28002,#28003,#28004,#28005,#28006,#28007,
#28008,#28009,#28010),.UNSPECIFIED.,.F.,.F.,(4,3,3,3,3,3,4),(-592.696219146929,
-591.94203667819,-591.18785420945,-590.43367174071,-589.67948927197,-588.925306803231,
-588.429163987831),.UNSPECIFIED.);
#601=B_SPLINE_CURVE_WITH_KNOTS('',3,(#28950,#28951,#28952,#28953,#28954,
#28955,#28956),.UNSPECIFIED.,.F.,.F.,(4,3,4),(26.4420020698014,26.6714021351404,
27.1563367194156),.UNSPECIFIED.);
#602=B_SPLINE_CURVE_WITH_KNOTS('',3,(#28959,#28960,#28961,#28962,#28963,
#28964,#28965,#28966,#28967,#28968,#28969,#28970,#28971,#28972,#28973,#28974,
#28975,#28976,#28977),.UNSPECIFIED.,.F.,.F.,(4,3,3,3,3,3,4),(-25.1327412287183,
-24.7316637980392,-24.2467292137639,-23.7617946294887,-23.2768600452134,
-22.7919254609381,-22.7054832247428),.UNSPECIFIED.);
#603=B_SPLINE_CURVE_WITH_KNOTS('',3,(#28982,#28983,#28984,#28985,#28986,
#28987,#28988,#28989,#28990,#28991,#28992,#28993,#28994,#28995,#28996,#28997,
#28998,#28999,#29000,#29001,#29002,#29003,#29004,#29005,#29006,#29007,#29008,
#29009,#29010,#29011,#29012,#29013,#29014,#29015,#29016,#29017,#29018,#29019,
#29020,#29021,#29022,#29023,#29024),.UNSPECIFIED.,.F.,.F.,(4,3,3,3,3,3,
3,3,3,3,3,3,3,3,4),(20.1588167626218,20.3672525395617,20.852187123837,21.3371217081123,
21.8220562923876,22.3069908766628,22.7919254609381,23.2768600452134,23.7617946294887,
24.246729213764,24.7316637980392,25.2165983823145,25.7015329665898,26.1864675508651,
26.4420020698014),.UNSPECIFIED.);
#604=B_SPLINE_CURVE_WITH_KNOTS('',3,(#29025,#29026,#29027,#29028,#29029,
#29030,#29031,#29032,#29033,#29034,#29035,#29036,#29037,#29038,#29039,#29040,
#29041,#29042,#29043,#29044,#29045,#29046,#29047,#29048,#29049,#29050,#29051,
#29052,#29053,#29054,#29055,#29056,#29057,#29058,#29059,#29060,#29061,#29062,
#29063,#29064,#29065,#29066,#29067),.UNSPECIFIED.,.F.,.F.,(4,3,3,3,3,3,
3,3,3,3,3,3,3,3,4),(-22.7054832247428,-22.3069908766628,-21.8220562923876,
-21.3371217081123,-20.852187123837,-20.3672525395617,-19.8823179552864,
-19.3973833710112,-18.9124487867359,-18.4275142024606,-17.9425796181853,
-17.45764503391,-16.9727104496348,-16.4877758653595,-16.4222979175632),
 .UNSPECIFIED.);
#605=B_SPLINE_CURVE_WITH_KNOTS('',3,(#29072,#29073,#29074,#29075,#29076,
#29077,#29078,#29079,#29080,#29081,#29082,#29083,#29084,#29085,#29086,#29087,
#29088,#29089,#29090,#29091,#29092,#29093,#29094,#29095,#29096,#29097,#29098,
#29099,#29100,#29101,#29102,#29103,#29104,#29105,#29106,#29107,#29108,#29109,
#29110,#29111,#29112,#29113,#29114),.UNSPECIFIED.,.F.,.F.,(4,3,3,3,3,3,
3,3,3,3,3,3,3,3,4),(13.8756314554422,14.0631029439831,14.5480375282584,
15.0329721125337,15.5179066968089,16.0028412810842,16.4877758653595,16.9727104496348,
17.45764503391,17.9425796181853,18.4275142024606,18.9124487867359,19.3973833710112,
19.8823179552864,20.1588167626218),.UNSPECIFIED.);
#606=B_SPLINE_CURVE_WITH_KNOTS('',3,(#29115,#29116,#29117,#29118,#29119,
#29120,#29121,#29122,#29123,#29124,#29125,#29126,#29127,#29128,#29129,#29130,
#29131,#29132,#29133,#29134,#29135,#29136,#29137,#29138,#29139,#29140,#29141,
#29142,#29143,#29144,#29145,#29146,#29147,#29148,#29149,#29150,#29151,#29152,
#29153,#29154,#29155,#29156,#29157),.UNSPECIFIED.,.F.,.F.,(4,3,3,3,3,3,
3,3,3,3,3,3,3,3,4),(-16.4222979175632,-16.0028412810842,-15.5179066968089,
-15.0329721125336,-14.5480375282584,-14.0631029439831,-13.5781683597078,
-13.0932337754325,-12.6082991911573,-12.123364606882,-11.6384300226067,
-11.1534954383314,-10.6685608540561,-10.1836262697809,-10.1391126103836),
 .UNSPECIFIED.);
#607=B_SPLINE_CURVE_WITH_KNOTS('',3,(#29163,#29164,#29165,#29166,#29167,
#29168,#29169,#29170,#29171,#29172,#29173,#29174,#29175,#29176,#29177,#29178,
#29179,#29180,#29181,#29182,#29183,#29184,#29185,#29186,#29187),
 .UNSPECIFIED.,.F.,.F.,(4,3,3,3,3,3,3,3,4),(-3.85592730320401,-3.39454208992695,
-2.90960750565167,-2.42467292137639,-1.93973833710111,-1.45480375282584,
-0.969869168550558,-0.484934584275278,0.),.UNSPECIFIED.);
#608=B_SPLINE_CURVE_WITH_KNOTS('',3,(#29190,#29191,#29192,#29193,#29194,
#29195,#29196,#29197,#29198,#29199,#29200,#29201,#29202,#29203,#29204,#29205,
#29206,#29207,#29208,#29209,#29210,#29211,#29212,#29213,#29214,#29215,#29216,
#29217,#29218,#29219,#29220,#29221,#29222,#29223,#29224,#29225,#29226),
 .UNSPECIFIED.,.F.,.F.,(4,3,3,3,3,3,3,3,3,3,3,3,4),(2.02359549069733,2.4246729213764,
2.90960750565168,3.39454208992696,3.87947667420224,4.36441125847751,4.84934584275279,
5.33428042702807,5.81921501130335,6.30414959557863,6.78908417985391,7.27401876412919,
7.59244614826264),.UNSPECIFIED.);
#609=B_SPLINE_CURVE_WITH_KNOTS('',3,(#29232,#29233,#29234,#29235,#29236,
#29237,#29238,#29239,#29240,#29241,#29242,#29243,#29244),.UNSPECIFIED.,
 .F.,.F.,(4,1,1,1,1,1,1,1,1,1,4),(34.5575191894877,34.6439614256831,35.1288960099583,
35.6138305942336,36.0987651785089,36.5836997627842,37.0686343470595,37.5535689313347,
38.03850351561,38.5234380998853,39.0083726841606),.UNSPECIFIED.);
#610=B_SPLINE_CURVE_WITH_KNOTS('',3,(#29247,#29248,#29249,#29250,#29251,
#29252,#29253,#29254,#29255,#29256,#29257,#29258,#29259,#29260),
 .UNSPECIFIED.,.F.,.F.,(4,1,1,1,1,1,1,1,1,1,1,4),(34.5575191894877,34.7659549664276,
35.2508895507029,35.7358241349782,36.2207587192535,36.7056933035287,37.190627887804,
37.6755624720793,38.1604970563546,38.6454316406299,39.1303662249051,39.5314436555842),
 .UNSPECIFIED.);
#611=B_SPLINE_CURVE_WITH_KNOTS('',3,(#29265,#29266,#29267,#29268,#29269,
#29270,#29271,#29272,#29273,#29274,#29275,#29276,#29277,#29278,#29279,#29280,
#29281),.UNSPECIFIED.,.F.,.F.,(4,1,1,1,1,1,1,1,1,1,1,1,1,1,4),(28.2743338823081,
28.3398118301044,28.8247464143797,29.309680998655,29.7946155829303,30.2795501672055,
30.7644847514808,31.2494193357561,31.7343539200314,32.2192885043067,32.7042230885819,
33.1891576728572,33.6740922571325,34.1590268414078,34.5575191894877),
 .UNSPECIFIED.);
#612=B_SPLINE_CURVE_WITH_KNOTS('',3,(#29282,#29283,#29284,#29285,#29286,
#29287,#29288,#29289,#29290,#29291,#29292,#29293,#29294,#29295,#29296,#29297,
#29298),.UNSPECIFIED.,.F.,.F.,(4,1,1,1,1,1,1,1,1,1,1,1,1,1,4),(28.2743338823081,
28.461805370849,28.9467399551243,29.4316745393996,29.9166091236748,30.4015437079501,
30.8864782922254,31.3714128765007,31.856347460776,32.3412820450512,32.8262166293265,
33.3111512136018,33.7960857978771,34.2810203821523,34.5575191894877),
 .UNSPECIFIED.);
#613=B_SPLINE_CURVE_WITH_KNOTS('',3,(#29303,#29304,#29305,#29306,#29307,
#29308,#29309,#29310,#29311,#29312,#29313,#29314,#29315,#29316,#29317,#29318,
#29319),.UNSPECIFIED.,.F.,.F.,(4,1,1,1,1,1,1,1,1,1,1,1,1,1,4),(21.9911485751286,
22.0356622345258,22.5205968188011,23.0055314030764,23.4904659873516,23.9754005716269,
24.4603351559022,24.9452697401775,25.4302043244528,25.915138908728,26.4000734930033,
26.8850080772786,27.3699426615539,27.8548772458292,28.2743338823081),
 .UNSPECIFIED.);
#614=B_SPLINE_CURVE_WITH_KNOTS('',3,(#29320,#29321,#29322,#29323,#29324,
#29325,#29326,#29327,#29328,#29329,#29330,#29331,#29332,#29333,#29334,#29335,
#29336),.UNSPECIFIED.,.F.,.F.,(4,1,1,1,1,1,1,1,1,1,1,1,1,1,4),(21.9911485751286,
22.1576557752704,22.6425903595457,23.1275249438209,23.6124595280962,24.0973941123715,
24.5823286966468,25.067263280922,25.5521978651973,26.0371324494726,26.5220670337479,
27.0070016180232,27.4919362022984,27.9768707865737,28.2743338823081),
 .UNSPECIFIED.);
#615=B_SPLINE_CURVE_WITH_KNOTS('',3,(#29342,#29343,#29344,#29345,#29346,
#29347),.UNSPECIFIED.,.F.,.F.,(4,1,1,4),(14.3987024268659,14.8836370111412,
15.3685715954165,15.707963267949),.UNSPECIFIED.);
#616=B_SPLINE_CURVE_WITH_KNOTS('',3,(#29350,#29351,#29352,#29353,#29354,
#29355,#29356),.UNSPECIFIED.,.F.,.F.,(4,1,1,1,4),(13.8756314554423,14.2767088861213,
14.7616434703966,15.2465780546719,15.707963267949),.UNSPECIFIED.);
#617=B_SPLINE_CURVE_WITH_KNOTS('',3,(#29358,#29359,#29360,#29361,#29362,
#29363,#29364,#29365,#29366,#29367,#29368,#29369,#29370,#29371,#29372,#29373,
#29374),.UNSPECIFIED.,.F.,.F.,(4,1,1,1,1,1,1,1,1,1,1,1,1,1,4),(15.707963267949,
15.7315126389472,16.2164472232225,16.7013818074977,17.186316391773,17.6712509760483,
18.1561855603236,18.6411201445989,19.1260547288741,19.6109893131494,20.0959238974247,
20.5808584817,21.0657930659752,21.5507276502505,21.9911485751286),
 .UNSPECIFIED.);
#618=B_SPLINE_CURVE_WITH_KNOTS('',3,(#29375,#29376,#29377,#29378,#29379,
#29380,#29381,#29382,#29383,#29384,#29385,#29386,#29387,#29388,#29389,#29390,
#29391),.UNSPECIFIED.,.F.,.F.,(4,1,1,1,1,1,1,1,1,1,1,1,1,1,4),(15.707963267949,
15.8535061796917,16.338440763967,16.8233753482423,17.3083099325176,17.7932445167929,
18.2781791010681,18.7631136853434,19.2480482696187,19.732982853894,20.2179174381693,
20.7028520224445,21.1877866067198,21.6727211909951,21.9911485751286),
 .UNSPECIFIED.);
#619=B_SPLINE_CURVE_WITH_KNOTS('',3,(#29628,#29629,#29630,#29631,#29632,
#29633,#29634,#29635,#29636,#29637,#29638,#29639,#29640,#29641,#29642,#29643,
#29644,#29645,#29646,#29647,#29648,#29649,#29650,#29651,#29652,#29653,#29654,
#29655,#29656,#29657,#29658,#29659,#29660,#29661,#29662,#29663,#29664,#29665,
#29666,#29667,#29668,#29669,#29670,#29671,#29672,#29673,#29674,#29675,#29676,
#29677,#29678,#29679,#29680,#29681,#29682,#29683,#29684,#29685,#29686,#29687,
#29688,#29689,#29690,#29691,#29692,#29693,#29694,#29695,#29696,#29697,#29698,
#29699,#29700,#29701,#29702,#29703,#29704,#29705,#29706),.UNSPECIFIED.,
 .F.,.F.,(4,3,3,3,3,3,3,3,3,3,3,3,3,3,3,3,3,3,3,3,3,3,3,3,3,3,4),(0.,0.152217503484067,
0.304359680258418,0.444170485281583,0.471986655324497,0.583981290304748,
0.733405099570558,0.837349441494007,0.892796146824606,0.921013703055727,
0.951233855348084,1.09712094103545,1.14918246726435,1.28571136325166,1.34308233147708,
1.3712989340972,1.51452714133526,1.65613253529925,1.69529805121359,1.76334984211607,
1.7978934044592,1.82919283472952,1.96987767951395,2.04822487844286,2.08147544830853,
2.22116640322431,2.3101075030587),.UNSPECIFIED.);
#620=B_SPLINE_CURVE_WITH_KNOTS('',3,(#29707,#29708,#29709,#29710,#29711,
#29712,#29713,#29714,#29715,#29716,#29717,#29718,#29719,#29720,#29721,#29722,
#29723,#29724,#29725,#29726,#29727,#29728,#29729,#29730,#29731,#29732,#29733,
#29734,#29735,#29736,#29737,#29738,#29739,#29740,#29741,#29742,#29743,#29744,
#29745,#29746,#29747,#29748,#29749,#29750,#29751,#29752,#29753,#29754,#29755,
#29756,#29757,#29758,#29759,#29760,#29761,#29762,#29763,#29764,#29765,#29766,
#29767,#29768,#29769,#29770,#29771,#29772,#29773,#29774,#29775,#29776,#29777,
#29778,#29779,#29780,#29781,#29782),.UNSPECIFIED.,.F.,.F.,(4,3,3,3,3,3,
3,3,3,3,3,3,3,3,3,3,3,3,3,3,3,3,3,3,3,4),(0.,0.136946952689913,0.275845446902835,
0.398834826821011,0.433645114326313,0.521824206739186,0.66322447960231,
0.763149933136536,0.825063822791896,0.861088222426034,1.00600575290352,
1.06292629373921,1.20295657612767,1.26303419900659,1.30095883119802,1.44786439483437,
1.59611049832394,1.62304742329305,1.69648823646563,1.73120190892034,1.76336658984008,
1.91360290275334,1.99760341236776,2.0413262282657,2.20106314648737,2.30292298333826),
 .UNSPECIFIED.);
#621=B_SPLINE_CURVE_WITH_KNOTS('',3,(#29783,#29784,#29785,#29786,#29787,
#29788,#29789,#29790,#29791,#29792,#29793,#29794,#29795,#29796,#29797,#29798,
#29799,#29800,#29801,#29802,#29803,#29804,#29805,#29806,#29807,#29808,#29809,
#29810,#29811,#29812,#29813,#29814,#29815,#29816,#29817,#29818,#29819,#29820,
#29821,#29822,#29823,#29824,#29825),.UNSPECIFIED.,.F.,.F.,(4,3,3,3,3,3,
3,3,3,3,3,3,3,3,4),(-10.1391126103836,-9.69869168550558,-9.2137571012303,
-8.72882251695502,-8.24388793267974,-7.75895334840446,-7.27401876412918,
-6.7890841798539,-6.30414959557862,-5.81921501130335,-5.33428042702807,
-4.84934584275279,-4.36441125847751,-3.87947667420223,-3.85592730320401),
 .UNSPECIFIED.);
#622=B_SPLINE_CURVE_WITH_KNOTS('',3,(#30062,#30063,#30064,#30065,#30066,
#30067,#30068,#30069,#30070,#30071,#30072,#30073,#30074,#30075,#30076,#30077,
#30078,#30079,#30080,#30081,#30082,#30083,#30084,#30085,#30086,#30087,#30088,
#30089,#30090,#30091,#30092,#30093,#30094,#30095,#30096,#30097,#30098,#30099,
#30100,#30101,#30102,#30103,#30104,#30105,#30106,#30107,#30108,#30109,#30110,
#30111,#30112,#30113,#30114,#30115,#30116,#30117,#30118,#30119,#30120,#30121,
#30122,#30123,#30124,#30125,#30126,#30127,#30128,#30129,#30130,#30131,#30132,
#30133,#30134,#30135,#30136,#30137),.UNSPECIFIED.,.F.,.F.,(4,3,3,3,3,3,
3,3,3,3,3,3,3,3,3,3,3,3,3,3,3,3,3,3,3,4),(0.,0.136946810378538,0.275845240706276,
0.398834723722739,0.4336450955117,0.521824206739202,0.663224551971021,0.763149987413078,
0.825063985186383,0.861088231251125,1.00600581272087,1.06292629373925,1.20295657612771,
1.26303419911027,1.30095883168088,1.44786437076391,1.59611047038881,1.6230474232931,
1.69648823731838,1.7312019179875,1.76336659191163,1.9136029038652,1.9976034144013,
2.04132622941513,2.20106314648744,2.30292298333833),.UNSPECIFIED.);
#623=B_SPLINE_CURVE_WITH_KNOTS('',3,(#30138,#30139,#30140,#30141,#30142,
#30143,#30144,#30145,#30146,#30147,#30148,#30149,#30150,#30151,#30152,#30153,
#30154,#30155,#30156,#30157,#30158,#30159,#30160,#30161,#30162,#30163,#30164,
#30165,#30166,#30167,#30168,#30169,#30170,#30171,#30172,#30173,#30174,#30175,
#30176,#30177,#30178,#30179,#30180),.UNSPECIFIED.,.F.,.F.,(4,3,3,3,3,3,
3,3,3,3,3,3,3,3,4),(7.59244614826264,7.75895334840446,8.24388793267975,
8.72882251695503,9.21375710123031,9.69869168550558,10.1836262697809,10.6685608540561,
11.1534954383314,11.6384300226067,12.123364606882,12.6082991911573,13.0932337754325,
13.5781683597078,13.8756314554422),.UNSPECIFIED.);
#624=B_SPLINE_CURVE_WITH_KNOTS('',3,(#30181,#30182,#30183,#30184,#30185,
#30186,#30187,#30188,#30189,#30190,#30191,#30192,#30193,#30194,#30195,#30196,
#30197,#30198,#30199,#30200,#30201,#30202,#30203,#30204,#30205,#30206,#30207,
#30208,#30209,#30210,#30211,#30212,#30213,#30214,#30215,#30216,#30217,#30218,
#30219,#30220,#30221,#30222,#30223,#30224,#30225,#30226,#30227,#30228,#30229,
#30230,#30231,#30232,#30233,#30234,#30235,#30236,#30237,#30238,#30239,#30240,
#30241,#30242,#30243,#30244,#30245,#30246,#30247,#30248,#30249,#30250,#30251,
#30252,#30253,#30254,#30255,#30256,#30257,#30258,#30259),.UNSPECIFIED.,
 .F.,.F.,(4,3,3,3,3,3,3,3,3,3,3,3,3,3,3,3,3,3,3,3,3,3,3,3,3,3,4),(0.,0.152217449424706,
0.304359666709038,0.444170478506893,0.471986651289376,0.583981290304748,
0.733405107154758,0.837349447182159,0.892796173398726,0.921013624406268,
0.951233846940009,1.09712092482237,1.14918246726436,1.28571136325167,1.34308233538123,
1.37129893684867,1.51452714023172,1.65613252898941,1.6952980512136,1.76334984315127,
1.79789341460453,1.829192837075,1.96987768339371,2.04822488467355,2.08147545454654,
2.22116640322432,2.3101075030587),.UNSPECIFIED.);
#625=B_SPLINE_CURVE_WITH_KNOTS('',3,(#30307,#30308,#30309,#30310,#30311,
#30312,#30313),.UNSPECIFIED.,.F.,.F.,(4,3,4),(26.4420020698014,26.6714021351403,
27.1563367194155),.UNSPECIFIED.);
#626=B_SPLINE_CURVE_WITH_KNOTS('',3,(#30316,#30317,#30318,#30319,#30320,
#30321,#30322,#30323,#30324,#30325,#30326,#30327,#30328,#30329,#30330,#30331,
#30332,#30333,#30334),.UNSPECIFIED.,.F.,.F.,(4,3,3,3,3,3,4),(-25.1327412287182,
-24.7316637980391,-24.2467292137639,-23.7617946294886,-23.2768600452133,
-22.791925460938,-22.7054832247427),.UNSPECIFIED.);
#627=B_SPLINE_CURVE_WITH_KNOTS('',3,(#30339,#30340,#30341,#30342,#30343,
#30344,#30345,#30346,#30347,#30348,#30349,#30350,#30351,#30352,#30353,#30354,
#30355,#30356,#30357,#30358,#30359,#30360,#30361,#30362,#30363,#30364,#30365,
#30366,#30367,#30368,#30369,#30370,#30371,#30372,#30373,#30374,#30375,#30376,
#30377,#30378,#30379,#30380,#30381),.UNSPECIFIED.,.F.,.F.,(4,3,3,3,3,3,
3,3,3,3,3,3,3,3,4),(20.1588167626218,20.3672525395616,20.8521871238369,
21.3371217081122,21.8220562923875,22.3069908766628,22.791925460938,23.2768600452133,
23.7617946294886,24.2467292137639,24.7316637980392,25.2165983823144,25.7015329665897,
26.186467550865,26.4420020698014),.UNSPECIFIED.);
#628=B_SPLINE_CURVE_WITH_KNOTS('',3,(#30382,#30383,#30384,#30385,#30386,
#30387,#30388,#30389,#30390,#30391,#30392,#30393,#30394,#30395,#30396,#30397,
#30398,#30399,#30400,#30401,#30402,#30403,#30404,#30405,#30406,#30407,#30408,
#30409,#30410,#30411,#30412,#30413,#30414,#30415,#30416,#30417,#30418,#30419,
#30420,#30421,#30422,#30423,#30424),.UNSPECIFIED.,.F.,.F.,(4,3,3,3,3,3,
3,3,3,3,3,3,3,3,4),(-22.7054832247427,-22.3069908766627,-21.8220562923875,
-21.3371217081122,-20.8521871238369,-20.3672525395616,-19.8823179552864,
-19.3973833710111,-18.9124487867358,-18.4275142024605,-17.9425796181852,
-17.45764503391,-16.9727104496347,-16.4877758653594,-16.4222979175631),
 .UNSPECIFIED.);
#629=B_SPLINE_CURVE_WITH_KNOTS('',3,(#30429,#30430,#30431,#30432,#30433,
#30434,#30435,#30436,#30437,#30438,#30439,#30440,#30441,#30442,#30443,#30444,
#30445,#30446,#30447,#30448,#30449,#30450,#30451,#30452,#30453,#30454,#30455,
#30456,#30457,#30458,#30459,#30460,#30461,#30462,#30463,#30464,#30465,#30466,
#30467,#30468,#30469,#30470,#30471),.UNSPECIFIED.,.F.,.F.,(4,3,3,3,3,3,
3,3,3,3,3,3,3,3,4),(13.8756314554422,14.063102943983,14.5480375282583,15.0329721125336,
15.5179066968089,16.0028412810842,16.4877758653594,16.9727104496347,17.45764503391,
17.9425796181853,18.4275142024605,18.9124487867358,19.3973833710111,19.8823179552864,
20.1588167626218),.UNSPECIFIED.);
#630=B_SPLINE_CURVE_WITH_KNOTS('',3,(#30472,#30473,#30474,#30475,#30476,
#30477,#30478,#30479,#30480,#30481,#30482,#30483,#30484,#30485,#30486,#30487,
#30488,#30489,#30490,#30491,#30492,#30493,#30494,#30495,#30496,#30497,#30498,
#30499,#30500,#30501,#30502,#30503,#30504,#30505,#30506,#30507,#30508,#30509,
#30510,#30511,#30512,#30513,#30514),.UNSPECIFIED.,.F.,.F.,(4,3,3,3,3,3,
3,3,3,3,3,3,3,3,4),(-16.4222979175631,-16.0028412810841,-15.5179066968089,
-15.0329721125336,-14.5480375282583,-14.063102943983,-13.5781683597078,
-13.0932337754325,-12.6082991911572,-12.1233646068819,-11.6384300226066,
-11.1534954383314,-10.6685608540561,-10.1836262697808,-10.1391126103836),
 .UNSPECIFIED.);
#631=B_SPLINE_CURVE_WITH_KNOTS('',3,(#30520,#30521,#30522,#30523,#30524,
#30525,#30526,#30527,#30528,#30529,#30530,#30531,#30532,#30533,#30534,#30535,
#30536,#30537,#30538,#30539,#30540,#30541,#30542,#30543,#30544),
 .UNSPECIFIED.,.F.,.F.,(4,3,3,3,3,3,3,3,4),(-3.85592730320397,-3.39454208992694,
-2.90960750565166,-2.42467292137638,-1.93973833710111,-1.45480375282583,
-0.969869168550556,-0.484934584275276,0.),.UNSPECIFIED.);
#632=B_SPLINE_CURVE_WITH_KNOTS('',3,(#30547,#30548,#30549,#30550,#30551,
#30552,#30553,#30554,#30555,#30556,#30557,#30558,#30559,#30560,#30561,#30562,
#30563,#30564,#30565,#30566,#30567,#30568,#30569,#30570,#30571,#30572,#30573,
#30574,#30575,#30576,#30577,#30578,#30579,#30580,#30581,#30582,#30583),
 .UNSPECIFIED.,.F.,.F.,(4,3,3,3,3,3,3,3,3,3,3,3,4),(2.02359549069725,2.42467292137638,
2.90960750565166,3.39454208992694,3.87947667420222,4.36441125847749,4.84934584275277,
5.33428042702805,5.81921501130332,6.3041495955786,6.78908417985388,7.27401876412916,
7.59244614826257),.UNSPECIFIED.);
#633=B_SPLINE_CURVE_WITH_KNOTS('',3,(#30589,#30590,#30591,#30592,#30593,
#30594,#30595,#30596,#30597,#30598,#30599,#30600,#30601),.UNSPECIFIED.,
 .F.,.F.,(4,1,1,1,1,1,1,1,1,1,4),(34.5575191894877,34.643961425683,35.1288960099583,
35.6138305942336,36.0987651785089,36.5836997627841,37.0686343470594,37.5535689313347,
38.03850351561,38.5234380998853,39.0083726841605),.UNSPECIFIED.);
#634=B_SPLINE_CURVE_WITH_KNOTS('',3,(#30604,#30605,#30606,#30607,#30608,
#30609,#30610,#30611,#30612,#30613,#30614,#30615,#30616,#30617),
 .UNSPECIFIED.,.F.,.F.,(4,1,1,1,1,1,1,1,1,1,1,4),(34.5575191894877,34.7659549664276,
35.2508895507029,35.7358241349782,36.2207587192534,36.7056933035287,37.190627887804,
37.6755624720793,38.1604970563545,38.6454316406298,39.1303662249051,39.5314436555842),
 .UNSPECIFIED.);
#635=B_SPLINE_CURVE_WITH_KNOTS('',3,(#30622,#30623,#30624,#30625,#30626,
#30627,#30628,#30629,#30630,#30631,#30632,#30633,#30634,#30635,#30636,#30637,
#30638),.UNSPECIFIED.,.F.,.F.,(4,1,1,1,1,1,1,1,1,1,1,1,1,1,4),(28.2743338823081,
28.3398118301044,28.8247464143797,29.309680998655,29.7946155829303,30.2795501672055,
30.7644847514808,31.2494193357561,31.7343539200314,32.2192885043067,32.7042230885819,
33.1891576728572,33.6740922571325,34.1590268414078,34.5575191894877),
 .UNSPECIFIED.);
#636=B_SPLINE_CURVE_WITH_KNOTS('',3,(#30639,#30640,#30641,#30642,#30643,
#30644,#30645,#30646,#30647,#30648,#30649,#30650,#30651,#30652,#30653,#30654,
#30655),.UNSPECIFIED.,.F.,.F.,(4,1,1,1,1,1,1,1,1,1,1,1,1,1,4),(28.2743338823081,
28.461805370849,28.9467399551243,29.4316745393996,29.9166091236748,30.4015437079501,
30.8864782922254,31.3714128765007,31.8563474607759,32.3412820450512,32.8262166293265,
33.3111512136018,33.796085797877,34.2810203821523,34.5575191894877),
 .UNSPECIFIED.);
#637=B_SPLINE_CURVE_WITH_KNOTS('',3,(#30660,#30661,#30662,#30663,#30664,
#30665,#30666,#30667,#30668,#30669,#30670,#30671,#30672,#30673,#30674,#30675,
#30676),.UNSPECIFIED.,.F.,.F.,(4,1,1,1,1,1,1,1,1,1,1,1,1,1,4),(21.9911485751285,
22.0356622345258,22.5205968188011,23.0055314030764,23.4904659873517,23.9754005716269,
24.4603351559022,24.9452697401775,25.4302043244528,25.9151389087281,26.4000734930033,
26.8850080772786,27.3699426615539,27.8548772458292,28.2743338823081),
 .UNSPECIFIED.);
#638=B_SPLINE_CURVE_WITH_KNOTS('',3,(#30677,#30678,#30679,#30680,#30681,
#30682,#30683,#30684,#30685,#30686,#30687,#30688,#30689,#30690,#30691,#30692,
#30693),.UNSPECIFIED.,.F.,.F.,(4,1,1,1,1,1,1,1,1,1,1,1,1,1,4),(21.9911485751285,
22.1576557752704,22.6425903595457,23.1275249438209,23.6124595280962,24.0973941123715,
24.5823286966468,25.0672632809221,25.5521978651973,26.0371324494726,26.5220670337479,
27.0070016180232,27.4919362022984,27.9768707865737,28.2743338823081),
 .UNSPECIFIED.);
#639=B_SPLINE_CURVE_WITH_KNOTS('',3,(#30699,#30700,#30701,#30702,#30703,
#30704),.UNSPECIFIED.,.F.,.F.,(4,1,1,4),(14.398702426866,14.8836370111412,
15.3685715954165,15.707963267949),.UNSPECIFIED.);
#640=B_SPLINE_CURVE_WITH_KNOTS('',3,(#30707,#30708,#30709,#30710,#30711,
#30712,#30713),.UNSPECIFIED.,.F.,.F.,(4,1,1,1,4),(13.8756314554423,14.2767088861214,
14.7616434703967,15.246578054672,15.707963267949),.UNSPECIFIED.);
#641=B_SPLINE_CURVE_WITH_KNOTS('',3,(#30715,#30716,#30717,#30718,#30719,
#30720,#30721,#30722,#30723,#30724,#30725,#30726,#30727,#30728,#30729,#30730,
#30731),.UNSPECIFIED.,.F.,.F.,(4,1,1,1,1,1,1,1,1,1,1,1,1,1,4),(15.707963267949,
15.7315126389472,16.2164472232225,16.7013818074978,17.1863163917731,17.6712509760483,
18.1561855603236,18.6411201445989,19.1260547288742,19.6109893131495,20.0959238974247,
20.5808584817,21.0657930659753,21.5507276502506,21.9911485751285),
 .UNSPECIFIED.);
#642=B_SPLINE_CURVE_WITH_KNOTS('',3,(#30732,#30733,#30734,#30735,#30736,
#30737,#30738,#30739,#30740,#30741,#30742,#30743,#30744,#30745,#30746,#30747,
#30748),.UNSPECIFIED.,.F.,.F.,(4,1,1,1,1,1,1,1,1,1,1,1,1,1,4),(15.707963267949,
15.8535061796918,16.3384407639671,16.8233753482423,17.3083099325176,17.7932445167929,
18.2781791010682,18.7631136853434,19.2480482696187,19.732982853894,20.2179174381693,
20.7028520224446,21.1877866067198,21.6727211909951,21.9911485751285),
 .UNSPECIFIED.);
#643=B_SPLINE_CURVE_WITH_KNOTS('',3,(#30985,#30986,#30987,#30988,#30989,
#30990,#30991,#30992,#30993,#30994,#30995,#30996,#30997,#30998,#30999,#31000,
#31001,#31002,#31003,#31004,#31005,#31006,#31007,#31008,#31009,#31010,#31011,
#31012,#31013,#31014,#31015,#31016,#31017,#31018,#31019,#31020,#31021,#31022,
#31023,#31024,#31025,#31026,#31027,#31028,#31029,#31030,#31031,#31032,#31033,
#31034,#31035,#31036,#31037,#31038,#31039,#31040,#31041,#31042,#31043,#31044,
#31045,#31046,#31047,#31048,#31049,#31050,#31051,#31052,#31053,#31054,#31055,
#31056,#31057,#31058,#31059,#31060,#31061,#31062,#31063),.UNSPECIFIED.,
 .F.,.F.,(4,3,3,3,3,3,3,3,3,3,3,3,3,3,3,3,3,3,3,3,3,3,3,3,3,3,4),(0.,0.152217036456305,
0.304359559108715,0.444170424706737,0.471986618924989,0.583981290304758,
0.733405166385902,0.837349491605518,0.892796377491797,0.921013022333204,
0.951233782076786,1.09712080302743,1.14918246726436,1.28571136325167,1.34308236504369,
1.37129895791557,1.51452713235171,1.65613248204747,1.6952980512136,1.76334985118988,
1.79789349372615,1.82919285548252,1.96987771326252,2.04822493259179,2.08147550163167,
2.22116640322437,2.31010750305869),.UNSPECIFIED.);
#644=B_SPLINE_CURVE_WITH_KNOTS('',3,(#31064,#31065,#31066,#31067,#31068,
#31069,#31070,#31071,#31072,#31073,#31074,#31075,#31076,#31077,#31078,#31079,
#31080,#31081,#31082,#31083,#31084,#31085,#31086,#31087,#31088,#31089,#31090,
#31091,#31092,#31093,#31094,#31095,#31096,#31097,#31098,#31099,#31100,#31101,
#31102,#31103,#31104,#31105,#31106,#31107,#31108,#31109,#31110,#31111,#31112,
#31113,#31114,#31115,#31116,#31117,#31118,#31119,#31120,#31121,#31122,#31123,
#31124,#31125,#31126,#31127,#31128,#31129,#31130,#31131,#31132,#31133,#31134,
#31135,#31136,#31137,#31138,#31139),.UNSPECIFIED.,.F.,.F.,(4,3,3,3,3,3,
3,3,3,3,3,3,3,3,3,3,3,3,3,3,3,3,3,3,3,4),(0.,0.136945726883441,0.275843669299818,
0.398833938019505,0.433644951757236,0.521824206739191,0.663225099265181,
0.763150397883695,0.825065214142751,0.86108829768601,1.00600626575755,1.06292629373924,
1.2029565761277,1.26303420019935,1.30095883535296,1.44786419265016,1.59611026313033,
1.6230474232931,1.69648824397694,1.73120198878345,1.76336660816569,1.9136029124139,
1.9976034301376,2.04132623841743,2.20106314648746,2.30292298333827),
 .UNSPECIFIED.);
#645=B_SPLINE_CURVE_WITH_KNOTS('',3,(#31140,#31141,#31142,#31143,#31144,
#31145,#31146,#31147,#31148,#31149,#31150,#31151,#31152,#31153,#31154,#31155,
#31156,#31157,#31158,#31159,#31160,#31161,#31162,#31163,#31164,#31165,#31166,
#31167,#31168,#31169,#31170,#31171,#31172,#31173,#31174,#31175,#31176,#31177,
#31178,#31179,#31180,#31181,#31182),.UNSPECIFIED.,.F.,.F.,(4,3,3,3,3,3,
3,3,3,3,3,3,3,3,4),(-10.1391126103836,-9.69869168550554,-9.21375710123026,
-8.72882251695498,-8.24388793267971,-7.75895334840443,-7.27401876412915,
-6.78908417985388,-6.3041495955786,-5.81921501130332,-5.33428042702805,
-4.84934584275277,-4.36441125847749,-3.87947667420222,-3.85592730320397),
 .UNSPECIFIED.);
#646=B_SPLINE_CURVE_WITH_KNOTS('',3,(#31419,#31420,#31421,#31422,#31423,
#31424,#31425,#31426,#31427,#31428,#31429,#31430,#31431,#31432,#31433,#31434,
#31435,#31436,#31437,#31438,#31439,#31440,#31441,#31442,#31443,#31444,#31445,
#31446,#31447,#31448,#31449,#31450,#31451,#31452,#31453,#31454,#31455,#31456,
#31457,#31458,#31459,#31460,#31461,#31462,#31463,#31464,#31465,#31466,#31467,
#31468,#31469,#31470,#31471,#31472,#31473,#31474,#31475,#31476,#31477,#31478,
#31479,#31480,#31481,#31482,#31483,#31484,#31485,#31486,#31487,#31488,#31489,
#31490,#31491,#31492,#31493,#31494),.UNSPECIFIED.,.F.,.F.,(4,3,3,3,3,3,
3,3,3,3,3,3,3,3,3,3,3,3,3,3,3,3,3,3,3,4),(0.,0.13694559794668,0.275843482121711,
0.398833844430455,0.433644934608767,0.521824206739199,0.663225163953675,
0.763150446400059,0.825065359497682,0.861088305549411,1.00600631943109,
1.06292629373921,1.20295657612767,1.26303420036263,1.30095883585408,1.44786417212767,
1.59611023917669,1.62304742329305,1.69648824478928,1.73120199734959,1.76336661014496,
1.91360291342174,1.99760343201209,2.04132623949843,2.20106314648734,2.30292298333806),
 .UNSPECIFIED.);
#647=B_SPLINE_CURVE_WITH_KNOTS('',3,(#31495,#31496,#31497,#31498,#31499,
#31500,#31501,#31502,#31503,#31504,#31505,#31506,#31507,#31508,#31509,#31510,
#31511,#31512,#31513,#31514,#31515,#31516,#31517,#31518,#31519,#31520,#31521,
#31522,#31523,#31524,#31525,#31526,#31527,#31528,#31529,#31530,#31531,#31532,
#31533,#31534,#31535,#31536,#31537),.UNSPECIFIED.,.F.,.F.,(4,3,3,3,3,3,
3,3,3,3,3,3,3,3,4),(7.59244614826257,7.75895334840444,8.24388793267971,
8.72882251695499,9.21375710123027,9.69869168550555,10.1836262697808,10.6685608540561,
11.1534954383314,11.6384300226067,12.1233646068819,12.6082991911572,13.0932337754325,
13.5781683597078,13.8756314554422),.UNSPECIFIED.);
#648=B_SPLINE_CURVE_WITH_KNOTS('',3,(#31538,#31539,#31540,#31541,#31542,
#31543,#31544,#31545,#31546,#31547,#31548,#31549,#31550,#31551,#31552,#31553,
#31554,#31555,#31556,#31557,#31558,#31559,#31560,#31561,#31562,#31563,#31564,
#31565,#31566,#31567,#31568,#31569,#31570,#31571,#31572,#31573,#31574,#31575,
#31576,#31577,#31578,#31579,#31580,#31581,#31582,#31583,#31584,#31585,#31586,
#31587,#31588,#31589,#31590,#31591,#31592,#31593,#31594,#31595,#31596,#31597,
#31598,#31599,#31600,#31601,#31602,#31603,#31604,#31605,#31606,#31607,#31608,
#31609,#31610,#31611,#31612,#31613,#31614,#31615,#31616),.UNSPECIFIED.,
 .F.,.F.,(4,3,3,3,3,3,3,3,3,3,3,3,3,3,3,3,3,3,3,3,3,3,3,3,3,3,4),(0.,0.152216987149307,
0.304359545775131,0.444170418039944,0.471986614921483,0.583981290304757,
0.733405173606566,0.837349497021023,0.892796401978486,0.921012950047068,
0.951233774221015,1.09712078868938,1.14918246726439,1.2857113632517,1.34308236856545,
1.37129896045007,1.51452713148655,1.65613247659821,1.69529805121362,1.76334985216405,
1.79789350346528,1.82919285775424,1.96987771686527,2.04822493836997,2.08147550729113,
2.22116640322435,2.31010750305867),.UNSPECIFIED.);
#649=B_SPLINE_CURVE_WITH_KNOTS('',3,(#31664,#31665,#31666,#31667,#31668,
#31669,#31670),.UNSPECIFIED.,.F.,.F.,(4,3,4),(26.4420020698013,26.6714021351403,
27.1563367194155),.UNSPECIFIED.);
#650=B_SPLINE_CURVE_WITH_KNOTS('',3,(#31673,#31674,#31675,#31676,#31677,
#31678,#31679,#31680,#31681,#31682,#31683,#31684,#31685,#31686,#31687,#31688,
#31689,#31690,#31691),.UNSPECIFIED.,.F.,.F.,(4,3,3,3,3,3,4),(-25.1327412287182,
-24.7316637980391,-24.2467292137639,-23.7617946294886,-23.2768600452133,
-22.791925460938,-22.7054832247427),.UNSPECIFIED.);
#651=B_SPLINE_CURVE_WITH_KNOTS('',3,(#31696,#31697,#31698,#31699,#31700,
#31701,#31702,#31703,#31704,#31705,#31706,#31707,#31708,#31709,#31710,#31711,
#31712,#31713,#31714,#31715,#31716,#31717,#31718,#31719,#31720,#31721,#31722,
#31723,#31724,#31725,#31726,#31727,#31728,#31729,#31730,#31731,#31732,#31733,
#31734,#31735,#31736,#31737,#31738),.UNSPECIFIED.,.F.,.F.,(4,3,3,3,3,3,
3,3,3,3,3,3,3,3,4),(20.1588167626218,20.3672525395616,20.8521871238369,
21.3371217081122,21.8220562923875,22.3069908766628,22.791925460938,23.2768600452133,
23.7617946294886,24.2467292137639,24.7316637980392,25.2165983823144,25.7015329665897,
26.186467550865,26.4420020698013),.UNSPECIFIED.);
#652=B_SPLINE_CURVE_WITH_KNOTS('',3,(#31739,#31740,#31741,#31742,#31743,
#31744,#31745,#31746,#31747,#31748,#31749,#31750,#31751,#31752,#31753,#31754,
#31755,#31756,#31757,#31758,#31759,#31760,#31761,#31762,#31763,#31764,#31765,
#31766,#31767,#31768,#31769,#31770,#31771,#31772,#31773,#31774,#31775,#31776,
#31777,#31778,#31779,#31780,#31781),.UNSPECIFIED.,.F.,.F.,(4,3,3,3,3,3,
3,3,3,3,3,3,3,3,4),(-22.7054832247427,-22.3069908766628,-21.8220562923875,
-21.3371217081122,-20.8521871238369,-20.3672525395616,-19.8823179552864,
-19.3973833710111,-18.9124487867358,-18.4275142024605,-17.9425796181853,
-17.45764503391,-16.9727104496347,-16.4877758653594,-16.4222979175631),
 .UNSPECIFIED.);
#653=B_SPLINE_CURVE_WITH_KNOTS('',3,(#31786,#31787,#31788,#31789,#31790,
#31791,#31792,#31793,#31794,#31795,#31796,#31797,#31798,#31799,#31800,#31801,
#31802,#31803,#31804,#31805,#31806,#31807,#31808,#31809,#31810,#31811,#31812,
#31813,#31814,#31815,#31816,#31817,#31818,#31819,#31820,#31821,#31822,#31823,
#31824,#31825,#31826,#31827,#31828),.UNSPECIFIED.,.F.,.F.,(4,3,3,3,3,3,
3,3,3,3,3,3,3,3,4),(13.8756314554422,14.063102943983,14.5480375282583,15.0329721125336,
15.5179066968089,16.0028412810842,16.4877758653594,16.9727104496347,17.45764503391,
17.9425796181853,18.4275142024605,18.9124487867358,19.3973833710111,19.8823179552864,
20.1588167626218),.UNSPECIFIED.);
#654=B_SPLINE_CURVE_WITH_KNOTS('',3,(#31829,#31830,#31831,#31832,#31833,
#31834,#31835,#31836,#31837,#31838,#31839,#31840,#31841,#31842,#31843,#31844,
#31845,#31846,#31847,#31848,#31849,#31850,#31851,#31852,#31853,#31854,#31855,
#31856,#31857,#31858,#31859,#31860,#31861,#31862,#31863,#31864,#31865,#31866,
#31867,#31868,#31869,#31870,#31871),.UNSPECIFIED.,.F.,.F.,(4,3,3,3,3,3,
3,3,3,3,3,3,3,3,4),(-16.4222979175631,-16.0028412810841,-15.5179066968089,
-15.0329721125336,-14.5480375282583,-14.063102943983,-13.5781683597078,
-13.0932337754325,-12.6082991911572,-12.1233646068819,-11.6384300226067,
-11.1534954383314,-10.6685608540561,-10.1836262697808,-10.1391126103835),
 .UNSPECIFIED.);
#655=B_SPLINE_CURVE_WITH_KNOTS('',3,(#31877,#31878,#31879,#31880,#31881,
#31882,#31883,#31884,#31885,#31886,#31887,#31888,#31889,#31890,#31891,#31892,
#31893,#31894,#31895,#31896,#31897,#31898,#31899,#31900,#31901),
 .UNSPECIFIED.,.F.,.F.,(4,3,3,3,3,3,3,3,4),(-3.8559273032039,-3.39454208992694,
-2.90960750565166,-2.42467292137639,-1.93973833710111,-1.45480375282583,
-0.969869168550556,-0.484934584275276,0.),.UNSPECIFIED.);
#656=B_SPLINE_CURVE_WITH_KNOTS('',3,(#31904,#31905,#31906,#31907,#31908,
#31909,#31910,#31911,#31912,#31913,#31914,#31915,#31916,#31917,#31918,#31919,
#31920,#31921,#31922,#31923,#31924,#31925,#31926,#31927,#31928,#31929,#31930,
#31931,#31932,#31933,#31934,#31935,#31936,#31937,#31938,#31939,#31940),
 .UNSPECIFIED.,.F.,.F.,(4,3,3,3,3,3,3,3,3,3,3,3,4),(2.02359549069725,2.42467292137639,
2.90960750565167,3.39454208992694,3.87947667420222,4.3644112584775,4.84934584275277,
5.33428042702805,5.81921501130333,6.30414959557861,6.78908417985388,7.27401876412916,
7.59244614826257),.UNSPECIFIED.);
#657=B_SPLINE_CURVE_WITH_KNOTS('',3,(#31946,#31947,#31948,#31949,#31950,
#31951,#31952,#31953,#31954,#31955,#31956,#31957,#31958),.UNSPECIFIED.,
 .F.,.F.,(4,1,1,1,1,1,1,1,1,1,4),(34.5575191894877,34.6439614256831,35.1288960099584,
35.6138305942336,36.0987651785089,36.5836997627842,37.0686343470595,37.5535689313348,
38.03850351561,38.5234380998853,39.0083726841606),.UNSPECIFIED.);
#658=B_SPLINE_CURVE_WITH_KNOTS('',3,(#31961,#31962,#31963,#31964,#31965,
#31966,#31967,#31968,#31969,#31970,#31971,#31972,#31973,#31974),
 .UNSPECIFIED.,.F.,.F.,(4,1,1,1,1,1,1,1,1,1,1,4),(34.5575191894877,34.7659549664276,
35.2508895507029,35.7358241349782,36.2207587192535,36.7056933035287,37.190627887804,
37.6755624720793,38.1604970563546,38.6454316406299,39.1303662249051,39.5314436555842),
 .UNSPECIFIED.);
#659=B_SPLINE_CURVE_WITH_KNOTS('',3,(#31979,#31980,#31981,#31982,#31983,
#31984,#31985,#31986,#31987,#31988,#31989,#31990,#31991,#31992,#31993,#31994,
#31995),.UNSPECIFIED.,.F.,.F.,(4,1,1,1,1,1,1,1,1,1,1,1,1,1,4),(28.2743338823082,
28.3398118301045,28.8247464143798,29.309680998655,29.7946155829303,30.2795501672056,
30.7644847514809,31.2494193357561,31.7343539200314,32.2192885043067,32.704223088582,
33.1891576728573,33.6740922571325,34.1590268414078,34.5575191894877),
 .UNSPECIFIED.);
#660=B_SPLINE_CURVE_WITH_KNOTS('',3,(#31996,#31997,#31998,#31999,#32000,
#32001,#32002,#32003,#32004,#32005,#32006,#32007,#32008,#32009,#32010,#32011,
#32012),.UNSPECIFIED.,.F.,.F.,(4,1,1,1,1,1,1,1,1,1,1,1,1,1,4),(28.2743338823082,
28.461805370849,28.9467399551243,29.4316745393996,29.9166091236749,30.4015437079501,
30.8864782922254,31.3714128765007,31.856347460776,32.3412820450512,32.8262166293265,
33.3111512136018,33.7960857978771,34.2810203821523,34.5575191894877),
 .UNSPECIFIED.);
#661=B_SPLINE_CURVE_WITH_KNOTS('',3,(#32017,#32018,#32019,#32020,#32021,
#32022,#32023,#32024,#32025,#32026,#32027,#32028,#32029,#32030,#32031,#32032,
#32033),.UNSPECIFIED.,.F.,.F.,(4,1,1,1,1,1,1,1,1,1,1,1,1,1,4),(21.9911485751286,
22.0356622345259,22.5205968188012,23.0055314030764,23.4904659873517,23.975400571627,
24.4603351559023,24.9452697401775,25.4302043244528,25.9151389087281,26.4000734930034,
26.8850080772787,27.3699426615539,27.8548772458292,28.2743338823082),
 .UNSPECIFIED.);
#662=B_SPLINE_CURVE_WITH_KNOTS('',3,(#32034,#32035,#32036,#32037,#32038,
#32039,#32040,#32041,#32042,#32043,#32044,#32045,#32046,#32047,#32048,#32049,
#32050),.UNSPECIFIED.,.F.,.F.,(4,1,1,1,1,1,1,1,1,1,1,1,1,1,4),(21.9911485751286,
22.1576557752704,22.6425903595457,23.127524943821,23.6124595280962,24.0973941123715,
24.5823286966468,25.0672632809221,25.5521978651974,26.0371324494726,26.5220670337479,
27.0070016180232,27.4919362022985,27.9768707865737,28.2743338823082),
 .UNSPECIFIED.);
#663=B_SPLINE_CURVE_WITH_KNOTS('',3,(#32056,#32057,#32058,#32059,#32060,
#32061),.UNSPECIFIED.,.F.,.F.,(4,1,1,4),(14.398702426866,14.8836370111413,
15.3685715954165,15.707963267949),.UNSPECIFIED.);
#664=B_SPLINE_CURVE_WITH_KNOTS('',3,(#32064,#32065,#32066,#32067,#32068,
#32069,#32070),.UNSPECIFIED.,.F.,.F.,(4,1,1,1,4),(13.8756314554423,14.2767088861214,
14.7616434703967,15.246578054672,15.707963267949),.UNSPECIFIED.);
#665=B_SPLINE_CURVE_WITH_KNOTS('',3,(#32072,#32073,#32074,#32075,#32076,
#32077,#32078,#32079,#32080,#32081,#32082,#32083,#32084,#32085,#32086,#32087,
#32088),.UNSPECIFIED.,.F.,.F.,(4,1,1,1,1,1,1,1,1,1,1,1,1,1,4),(15.707963267949,
15.7315126389473,16.2164472232226,16.7013818074978,17.1863163917731,17.6712509760484,
18.1561855603237,18.6411201445989,19.1260547288742,19.6109893131495,20.0959238974248,
20.5808584817,21.0657930659753,21.5507276502506,21.9911485751286),
 .UNSPECIFIED.);
#666=B_SPLINE_CURVE_WITH_KNOTS('',3,(#32089,#32090,#32091,#32092,#32093,
#32094,#32095,#32096,#32097,#32098,#32099,#32100,#32101,#32102,#32103,#32104,
#32105),.UNSPECIFIED.,.F.,.F.,(4,1,1,1,1,1,1,1,1,1,1,1,1,1,4),(15.707963267949,
15.8535061796918,16.3384407639671,16.8233753482424,17.3083099325176,17.7932445167929,
18.2781791010682,18.7631136853435,19.2480482696188,19.732982853894,20.2179174381693,
20.7028520224446,21.1877866067199,21.6727211909951,21.9911485751286),
 .UNSPECIFIED.);
#667=B_SPLINE_CURVE_WITH_KNOTS('',3,(#32342,#32343,#32344,#32345,#32346,
#32347,#32348,#32349,#32350,#32351,#32352,#32353,#32354,#32355,#32356,#32357,
#32358,#32359,#32360,#32361,#32362,#32363,#32364,#32365,#32366,#32367,#32368,
#32369,#32370,#32371,#32372,#32373,#32374,#32375,#32376,#32377,#32378,#32379,
#32380,#32381,#32382,#32383,#32384,#32385,#32386,#32387,#32388,#32389,#32390,
#32391,#32392,#32393,#32394,#32395,#32396,#32397,#32398,#32399,#32400,#32401,
#32402,#32403,#32404,#32405,#32406,#32407,#32408,#32409,#32410,#32411,#32412,
#32413,#32414,#32415,#32416,#32417,#32418,#32419,#32420),.UNSPECIFIED.,
 .F.,.F.,(4,3,3,3,3,3,3,3,3,3,3,3,3,3,3,3,3,3,3,3,3,3,3,3,3,3,4),(0.,0.152215941592882,
0.304359238378302,0.44417026434153,0.471986524584209,0.583981290304758,
0.733405333521443,0.837349616957177,0.892796925719252,0.921011414368794,
0.95123360439561,1.09712049653845,1.14918246726438,1.28571136325169,1.34308244168001,
1.37129901391245,1.51452711558388,1.6561323669284,1.69529805121364,1.76334987370452,
1.79789372311875,1.82919290943268,1.96987779531733,2.04822506388956,2.08147563082119,
2.22116640322435,2.31010750305866),.UNSPECIFIED.);
#668=B_SPLINE_CURVE_WITH_KNOTS('',3,(#32421,#32422,#32423,#32424,#32425,
#32426,#32427,#32428,#32429,#32430,#32431,#32432,#32433,#32434,#32435,#32436,
#32437,#32438,#32439,#32440,#32441,#32442,#32443,#32444,#32445,#32446,#32447,
#32448,#32449,#32450,#32451,#32452,#32453,#32454,#32455,#32456,#32457,#32458,
#32459,#32460,#32461,#32462,#32463,#32464,#32465,#32466,#32467,#32468,#32469,
#32470,#32471,#32472,#32473,#32474,#32475,#32476,#32477,#32478,#32479,#32480,
#32481,#32482,#32483,#32484,#32485,#32486,#32487,#32488,#32489,#32490,#32491,
#32492,#32493,#32494,#32495,#32496),.UNSPECIFIED.,.F.,.F.,(4,3,3,3,3,3,
3,3,3,3,3,3,3,3,3,3,3,3,3,3,3,3,3,3,3,4),(0.,0.13694288511905,0.275839534909346,
0.398831870824263,0.43364457290582,0.521824206739181,0.663226502332769,
0.763151450184378,0.825068371201986,0.861088466872379,1.00600743409727,
1.06292629373921,1.20295657612767,1.26303420520301,1.30095884525044,1.44786376844848,
1.59610976549603,1.62304742329305,1.69648826291636,1.73120219323328,1.76336665553203,
1.91360293601108,1.99760347404716,2.04132626333146,2.20106314648734,2.30292298333801),
 .UNSPECIFIED.);
#669=B_SPLINE_CURVE_WITH_KNOTS('',3,(#32497,#32498,#32499,#32500,#32501,
#32502,#32503,#32504,#32505,#32506,#32507,#32508,#32509,#32510,#32511,#32512,
#32513,#32514,#32515,#32516,#32517,#32518,#32519,#32520,#32521,#32522,#32523,
#32524,#32525,#32526,#32527,#32528,#32529,#32530,#32531,#32532,#32533,#32534,
#32535,#32536,#32537,#32538,#32539),.UNSPECIFIED.,.F.,.F.,(4,3,3,3,3,3,
3,3,3,3,3,3,3,3,4),(-10.1391126103835,-9.69869168550554,-9.21375710123027,
-8.72882251695499,-8.24388793267971,-7.75895334840444,-7.27401876412916,
-6.78908417985388,-6.3041495955786,-5.81921501130332,-5.33428042702805,
-4.84934584275277,-4.3644112584775,-3.87947667420222,-3.8559273032039),
 .UNSPECIFIED.);
#670=B_SPLINE_CURVE_WITH_KNOTS('',3,(#32776,#32777,#32778,#32779,#32780,
#32781,#32782,#32783,#32784,#32785,#32786,#32787,#32788,#32789,#32790,#32791,
#32792,#32793,#32794,#32795,#32796,#32797,#32798,#32799,#32800,#32801,#32802,
#32803,#32804,#32805,#32806,#32807,#32808,#32809,#32810,#32811,#32812,#32813,
#32814,#32815,#32816,#32817,#32818,#32819,#32820,#32821,#32822,#32823,#32824,
#32825,#32826,#32827,#32828,#32829,#32830,#32831,#32832,#32833,#32834,#32835,
#32836,#32837,#32838,#32839,#32840,#32841,#32842,#32843,#32844,#32845,#32846,
#32847,#32848,#32849,#32850,#32851),.UNSPECIFIED.,.F.,.F.,(4,3,3,3,3,3,
3,3,3,3,3,3,3,3,3,3,3,3,3,3,3,3,3,3,3,4),(0.,0.136942783675313,0.275839386965687,
0.398831796852438,0.433644559362179,0.52182420673919,0.663226551512937,
0.763151487069502,0.825068482010607,0.861088472748197,1.00600747520934,
1.0629262937392,1.20295657612766,1.2630342054286,1.30095884559252,1.4478637544197,
1.59610974893898,1.62304742329305,1.69648826363017,1.73120220104301,1.76336665734949,
1.91360293688396,1.99760347568968,2.04132626433107,2.20106314648737,2.30292298333823),
 .UNSPECIFIED.);
#671=B_SPLINE_CURVE_WITH_KNOTS('',3,(#32852,#32853,#32854,#32855,#32856,
#32857,#32858,#32859,#32860,#32861,#32862,#32863,#32864,#32865,#32866,#32867,
#32868,#32869,#32870,#32871,#32872,#32873,#32874,#32875,#32876,#32877,#32878,
#32879,#32880,#32881,#32882,#32883,#32884,#32885,#32886,#32887,#32888,#32889,
#32890,#32891,#32892,#32893,#32894),.UNSPECIFIED.,.F.,.F.,(4,3,3,3,3,3,
3,3,3,3,3,3,3,3,4),(7.59244614826257,7.75895334840444,8.24388793267972,
8.728822516955,9.21375710123027,9.69869168550555,10.1836262697808,10.6685608540561,
11.1534954383314,11.6384300226067,12.1233646068819,12.6082991911572,13.0932337754325,
13.5781683597078,13.8756314554422),.UNSPECIFIED.);
#672=B_SPLINE_CURVE_WITH_KNOTS('',3,(#32895,#32896,#32897,#32898,#32899,
#32900,#32901,#32902,#32903,#32904,#32905,#32906,#32907,#32908,#32909,#32910,
#32911,#32912,#32913,#32914,#32915,#32916,#32917,#32918,#32919,#32920,#32921,
#32922,#32923,#32924,#32925,#32926,#32927,#32928,#32929,#32930,#32931,#32932,
#32933,#32934,#32935,#32936,#32937,#32938,#32939,#32940,#32941,#32942,#32943,
#32944,#32945,#32946,#32947,#32948,#32949,#32950,#32951,#32952,#32953,#32954,
#32955,#32956,#32957,#32958,#32959,#32960,#32961,#32962,#32963,#32964,#32965,
#32966,#32967,#32968,#32969,#32970,#32971,#32972,#32973),.UNSPECIFIED.,
 .F.,.F.,(4,3,3,3,3,3,3,3,3,3,3,3,3,3,3,3,3,3,3,3,3,3,3,3,3,3,4),(0.,0.152215902191206,
0.304359225867899,0.444170258086332,0.471986521031257,0.583981290304766,
0.733405339782993,0.837349621653341,0.892796945580561,0.921011356266073,
0.95123359785535,1.09712048593541,1.14918246726438,1.28571136325169,1.34308244436525,
1.37129901598247,1.51452711514042,1.65613236306049,1.69529805121362,1.76334987454827,
1.79789373174083,1.82919291148127,1.9698777983055,2.04822506867616,2.08147563558465,
2.2211664032244,2.31010750305872),.UNSPECIFIED.);
#673=B_SPLINE_CURVE_WITH_KNOTS('',3,(#33021,#33022,#33023,#33024,#33025,
#33026,#33027),.UNSPECIFIED.,.F.,.F.,(4,3,4),(26.4420020698014,26.6714021351403,
27.1563367194156),.UNSPECIFIED.);
#674=B_SPLINE_CURVE_WITH_KNOTS('',3,(#33030,#33031,#33032,#33033,#33034,
#33035,#33036,#33037,#33038,#33039,#33040,#33041,#33042,#33043,#33044,#33045,
#33046,#33047,#33048),.UNSPECIFIED.,.F.,.F.,(4,3,3,3,3,3,4),(-25.1327412287183,
-24.7316637980392,-24.2467292137639,-23.7617946294886,-23.2768600452134,
-22.7919254609381,-22.7054832247428),.UNSPECIFIED.);
#675=B_SPLINE_CURVE_WITH_KNOTS('',3,(#33053,#33054,#33055,#33056,#33057,
#33058,#33059,#33060,#33061,#33062,#33063,#33064,#33065,#33066,#33067,#33068,
#33069,#33070,#33071,#33072,#33073,#33074,#33075,#33076,#33077,#33078,#33079,
#33080,#33081,#33082,#33083,#33084,#33085,#33086,#33087,#33088,#33089,#33090,
#33091,#33092,#33093,#33094,#33095),.UNSPECIFIED.,.F.,.F.,(4,3,3,3,3,3,
3,3,3,3,3,3,3,3,4),(20.1588167626218,20.3672525395617,20.852187123837,21.3371217081123,
21.8220562923875,22.3069908766628,22.7919254609381,23.2768600452134,23.7617946294887,
24.2467292137639,24.7316637980392,25.2165983823145,25.7015329665898,26.1864675508651,
26.4420020698014),.UNSPECIFIED.);
#676=B_SPLINE_CURVE_WITH_KNOTS('',3,(#33096,#33097,#33098,#33099,#33100,
#33101,#33102,#33103,#33104,#33105,#33106,#33107,#33108,#33109,#33110,#33111,
#33112,#33113,#33114,#33115,#33116,#33117,#33118,#33119,#33120,#33121,#33122,
#33123,#33124,#33125,#33126,#33127,#33128,#33129,#33130,#33131,#33132,#33133,
#33134,#33135,#33136,#33137,#33138),.UNSPECIFIED.,.F.,.F.,(4,3,3,3,3,3,
3,3,3,3,3,3,3,3,4),(-22.7054832247428,-22.3069908766628,-21.8220562923875,
-21.3371217081122,-20.852187123837,-20.3672525395617,-19.8823179552864,
-19.3973833710111,-18.9124487867359,-18.4275142024606,-17.9425796181853,
-17.45764503391,-16.9727104496347,-16.4877758653595,-16.4222979175632),
 .UNSPECIFIED.);
#677=B_SPLINE_CURVE_WITH_KNOTS('',3,(#33143,#33144,#33145,#33146,#33147,
#33148,#33149,#33150,#33151,#33152,#33153,#33154,#33155,#33156,#33157,#33158,
#33159,#33160,#33161,#33162,#33163,#33164,#33165,#33166,#33167,#33168,#33169,
#33170,#33171,#33172,#33173,#33174,#33175,#33176,#33177,#33178,#33179,#33180,
#33181,#33182,#33183,#33184,#33185),.UNSPECIFIED.,.F.,.F.,(4,3,3,3,3,3,
3,3,3,3,3,3,3,3,4),(13.8756314554422,14.0631029439831,14.5480375282584,
15.0329721125336,15.5179066968089,16.0028412810842,16.4877758653595,16.9727104496348,
17.45764503391,17.9425796181853,18.4275142024606,18.9124487867359,19.3973833710111,
19.8823179552864,20.1588167626218),.UNSPECIFIED.);
#678=B_SPLINE_CURVE_WITH_KNOTS('',3,(#33186,#33187,#33188,#33189,#33190,
#33191,#33192,#33193,#33194,#33195,#33196,#33197,#33198,#33199,#33200,#33201,
#33202,#33203,#33204,#33205,#33206,#33207,#33208,#33209,#33210,#33211,#33212,
#33213,#33214,#33215,#33216,#33217,#33218,#33219,#33220,#33221,#33222,#33223,
#33224,#33225,#33226,#33227,#33228),.UNSPECIFIED.,.F.,.F.,(4,3,3,3,3,3,
3,3,3,3,3,3,3,3,4),(-16.4222979175632,-16.0028412810842,-15.5179066968089,
-15.0329721125336,-14.5480375282584,-14.0631029439831,-13.5781683597078,
-13.0932337754325,-12.6082991911572,-12.123364606882,-11.6384300226067,
-11.1534954383314,-10.6685608540561,-10.1836262697808,-10.1391126103836),
 .UNSPECIFIED.);
#679=B_SPLINE_CURVE_WITH_KNOTS('',3,(#33234,#33235,#33236,#33237,#33238,
#33239,#33240,#33241,#33242,#33243,#33244,#33245,#33246,#33247,#33248,#33249,
#33250,#33251,#33252,#33253,#33254,#33255,#33256,#33257,#33258),
 .UNSPECIFIED.,.F.,.F.,(4,3,3,3,3,3,3,3,4),(-3.85592730320397,-3.39454208992695,
-2.90960750565167,-2.42467292137639,-1.93973833710111,-1.45480375282583,
-0.969869168550554,-0.484934584275278,0.),.UNSPECIFIED.);
#680=B_SPLINE_CURVE_WITH_KNOTS('',3,(#33261,#33262,#33263,#33264,#33265,
#33266,#33267,#33268,#33269,#33270,#33271,#33272,#33273,#33274,#33275,#33276,
#33277,#33278,#33279,#33280,#33281,#33282,#33283,#33284,#33285,#33286,#33287,
#33288,#33289,#33290,#33291,#33292,#33293,#33294,#33295,#33296,#33297),
 .UNSPECIFIED.,.F.,.F.,(4,3,3,3,3,3,3,3,3,3,3,3,4),(2.02359549069725,2.42467292137639,
2.90960750565167,3.39454208992695,3.87947667420223,4.36441125847751,4.84934584275279,
5.33428042702807,5.81921501130334,6.30414959557862,6.7890841798539,7.27401876412918,
7.59244614826264),.UNSPECIFIED.);
#681=B_SPLINE_CURVE_WITH_KNOTS('',3,(#33303,#33304,#33305,#33306,#33307,
#33308,#33309,#33310,#33311,#33312,#33313,#33314,#33315),.UNSPECIFIED.,
 .F.,.F.,(4,1,1,1,1,1,1,1,1,1,4),(34.5575191894877,34.6439614256831,35.1288960099583,
35.6138305942336,36.0987651785089,36.5836997627842,37.0686343470595,37.5535689313347,
38.03850351561,38.5234380998853,39.0083726841606),.UNSPECIFIED.);
#682=B_SPLINE_CURVE_WITH_KNOTS('',3,(#33318,#33319,#33320,#33321,#33322,
#33323,#33324,#33325,#33326,#33327,#33328,#33329,#33330,#33331),
 .UNSPECIFIED.,.F.,.F.,(4,1,1,1,1,1,1,1,1,1,1,4),(34.5575191894877,34.7659549664276,
35.2508895507029,35.7358241349782,36.2207587192535,36.7056933035287,37.190627887804,
37.6755624720793,38.1604970563546,38.6454316406298,39.1303662249051,39.5314436555842),
 .UNSPECIFIED.);
#683=B_SPLINE_CURVE_WITH_KNOTS('',3,(#33336,#33337,#33338,#33339,#33340,
#33341,#33342,#33343,#33344,#33345,#33346,#33347,#33348,#33349,#33350,#33351,
#33352),.UNSPECIFIED.,.F.,.F.,(4,1,1,1,1,1,1,1,1,1,1,1,1,1,4),(28.2743338823082,
28.3398118301045,28.8247464143797,29.309680998655,29.7946155829303,30.2795501672056,
30.7644847514808,31.2494193357561,31.7343539200314,32.2192885043067,32.704223088582,
33.1891576728572,33.6740922571325,34.1590268414078,34.5575191894877),
 .UNSPECIFIED.);
#684=B_SPLINE_CURVE_WITH_KNOTS('',3,(#33353,#33354,#33355,#33356,#33357,
#33358,#33359,#33360,#33361,#33362,#33363,#33364,#33365,#33366,#33367,#33368,
#33369),.UNSPECIFIED.,.F.,.F.,(4,1,1,1,1,1,1,1,1,1,1,1,1,1,4),(28.2743338823082,
28.461805370849,28.9467399551243,29.4316745393995,29.9166091236748,30.4015437079501,
30.8864782922254,31.3714128765007,31.8563474607759,32.3412820450512,32.8262166293265,
33.3111512136018,33.7960857978771,34.2810203821523,34.5575191894877),
 .UNSPECIFIED.);
#685=B_SPLINE_CURVE_WITH_KNOTS('',3,(#33374,#33375,#33376,#33377,#33378,
#33379,#33380,#33381,#33382,#33383,#33384,#33385,#33386,#33387,#33388,#33389,
#33390),.UNSPECIFIED.,.F.,.F.,(4,1,1,1,1,1,1,1,1,1,1,1,1,1,4),(21.9911485751286,
22.0356622345258,22.5205968188011,23.0055314030764,23.4904659873517,23.9754005716269,
24.4603351559022,24.9452697401775,25.4302043244528,25.9151389087281,26.4000734930033,
26.8850080772786,27.3699426615539,27.8548772458292,28.2743338823082),
 .UNSPECIFIED.);
#686=B_SPLINE_CURVE_WITH_KNOTS('',3,(#33391,#33392,#33393,#33394,#33395,
#33396,#33397,#33398,#33399,#33400,#33401,#33402,#33403,#33404,#33405,#33406,
#33407),.UNSPECIFIED.,.F.,.F.,(4,1,1,1,1,1,1,1,1,1,1,1,1,1,4),(21.9911485751286,
22.1576557752704,22.6425903595456,23.1275249438209,23.6124595280962,24.0973941123715,
24.5823286966468,25.067263280922,25.5521978651973,26.0371324494726,26.5220670337479,
27.0070016180232,27.4919362022984,27.9768707865737,28.2743338823082),
 .UNSPECIFIED.);
#687=B_SPLINE_CURVE_WITH_KNOTS('',3,(#33413,#33414,#33415,#33416,#33417,
#33418),.UNSPECIFIED.,.F.,.F.,(4,1,1,4),(14.3987024268659,14.8836370111412,
15.3685715954165,15.707963267949),.UNSPECIFIED.);
#688=B_SPLINE_CURVE_WITH_KNOTS('',3,(#33421,#33422,#33423,#33424,#33425,
#33426,#33427),.UNSPECIFIED.,.F.,.F.,(4,1,1,1,4),(13.8756314554422,14.2767088861214,
14.7616434703967,15.2465780546719,15.707963267949),.UNSPECIFIED.);
#689=B_SPLINE_CURVE_WITH_KNOTS('',3,(#33429,#33430,#33431,#33432,#33433,
#33434,#33435,#33436,#33437,#33438,#33439,#33440,#33441,#33442,#33443,#33444,
#33445),.UNSPECIFIED.,.F.,.F.,(4,1,1,1,1,1,1,1,1,1,1,1,1,1,4),(15.707963267949,
15.7315126389472,16.2164472232225,16.7013818074978,17.1863163917731,17.6712509760483,
18.1561855603236,18.6411201445989,19.1260547288742,19.6109893131494,20.0959238974247,
20.5808584817,21.0657930659753,21.5507276502506,21.9911485751286),
 .UNSPECIFIED.);
#690=B_SPLINE_CURVE_WITH_KNOTS('',3,(#33446,#33447,#33448,#33449,#33450,
#33451,#33452,#33453,#33454,#33455,#33456,#33457,#33458,#33459,#33460,#33461,
#33462),.UNSPECIFIED.,.F.,.F.,(4,1,1,1,1,1,1,1,1,1,1,1,1,1,4),(15.707963267949,
15.8535061796917,16.338440763967,16.8233753482423,17.3083099325176,17.7932445167929,
18.2781791010681,18.7631136853434,19.2480482696187,19.732982853894,20.2179174381693,
20.7028520224445,21.1877866067198,21.6727211909951,21.9911485751286),
 .UNSPECIFIED.);
#691=B_SPLINE_CURVE_WITH_KNOTS('',3,(#33699,#33700,#33701,#33702,#33703,
#33704,#33705,#33706,#33707,#33708,#33709,#33710,#33711,#33712,#33713,#33714,
#33715,#33716,#33717,#33718,#33719,#33720,#33721,#33722,#33723,#33724,#33725,
#33726,#33727,#33728,#33729,#33730,#33731,#33732,#33733,#33734,#33735,#33736,
#33737,#33738,#33739,#33740,#33741,#33742,#33743,#33744,#33745,#33746,#33747,
#33748,#33749,#33750,#33751,#33752,#33753,#33754,#33755,#33756,#33757,#33758,
#33759,#33760,#33761,#33762,#33763,#33764,#33765,#33766,#33767,#33768,#33769,
#33770,#33771,#33772,#33773,#33774,#33775,#33776,#33777),.UNSPECIFIED.,
 .F.,.F.,(4,3,3,3,3,3,3,3,3,3,3,3,3,3,3,3,3,3,3,3,3,3,3,3,3,3,4),(0.,0.152215598280746,
0.304359127092899,0.444170208698824,0.47198649256547,0.58398129030475,0.733405388599423,
0.837349658265653,0.892797098974412,0.921010909097056,0.951233547269046,
1.0971204053036,1.14918246726435,1.28571136325164,1.34308246486694,1.37129903143152,
1.514527111463,1.65613233320033,1.69529805121353,1.76334988113777,1.79789380048528,
1.82919292778863,1.96987782168459,2.04822510610851,2.08147567267347,2.22116640322417,
2.31010750305849),.UNSPECIFIED.);
#692=B_SPLINE_CURVE_WITH_KNOTS('',3,(#33778,#33779,#33780,#33781,#33782,
#33783,#33784,#33785,#33786,#33787,#33788,#33789,#33790,#33791,#33792,#33793,
#33794,#33795,#33796,#33797,#33798,#33799,#33800,#33801,#33802,#33803,#33804,
#33805,#33806,#33807,#33808,#33809,#33810,#33811,#33812,#33813,#33814,#33815,
#33816,#33817,#33818,#33819,#33820,#33821,#33822,#33823,#33824,#33825,#33826,
#33827,#33828,#33829,#33830,#33831,#33832,#33833,#33834,#33835,#33836,#33837,
#33838,#33839,#33840,#33841,#33842,#33843,#33844,#33845,#33846,#33847,#33848,
#33849,#33850,#33851,#33852,#33853),.UNSPECIFIED.,.F.,.F.,(4,3,3,3,3,3,
3,3,3,3,3,3,3,3,3,3,3,3,3,3,3,3,3,3,3,4),(0.,0.136942003107033,0.275838247773224,
0.398831227256207,0.433644454679001,0.521824206739189,0.663226927758571,
0.763151769253735,0.825069330101608,0.861088517754105,1.00600779023923,
1.06292629373923,1.20295657612769,1.26303420725827,1.30095884831302,1.44786364908515,
1.59610962438193,1.62304742329308,1.69648826922106,1.73120226201003,1.76336667156587,
1.91360294366234,1.99760348846723,2.041326271508,2.20106314648742,2.30292298333822),
 .UNSPECIFIED.);
#693=B_SPLINE_CURVE_WITH_KNOTS('',3,(#33854,#33855,#33856,#33857,#33858,
#33859,#33860,#33861,#33862,#33863,#33864,#33865,#33866,#33867,#33868,#33869,
#33870,#33871,#33872,#33873,#33874,#33875,#33876,#33877,#33878,#33879,#33880,
#33881,#33882,#33883,#33884,#33885,#33886,#33887,#33888,#33889,#33890,#33891,
#33892,#33893,#33894,#33895,#33896),.UNSPECIFIED.,.F.,.F.,(4,3,3,3,3,3,
3,3,3,3,3,3,3,3,4),(-10.1391126103836,-9.69869168550557,-9.21375710123029,
-8.72882251695501,-8.24388793267973,-7.75895334840445,-7.27401876412917,
-6.7890841798539,-6.30414959557862,-5.81921501130334,-5.33428042702806,
-4.84934584275278,-4.3644112584775,-3.87947667420223,-3.85592730320397),
 .UNSPECIFIED.);
#694=B_SPLINE_CURVE_WITH_KNOTS('',3,(#34133,#34134,#34135,#34136,#34137,
#34138,#34139,#34140,#34141,#34142,#34143,#34144,#34145,#34146,#34147,#34148,
#34149,#34150,#34151,#34152,#34153,#34154,#34155,#34156,#34157,#34158,#34159,
#34160,#34161,#34162,#34163,#34164,#34165,#34166,#34167,#34168,#34169,#34170,
#34171,#34172,#34173,#34174,#34175,#34176,#34177,#34178,#34179,#34180,#34181,
#34182,#34183,#34184,#34185,#34186,#34187,#34188,#34189,#34190,#34191,#34192,
#34193,#34194,#34195,#34196,#34197,#34198,#34199,#34200,#34201,#34202,#34203,
#34204,#34205,#34206,#34207,#34208),.UNSPECIFIED.,.F.,.F.,(4,3,3,3,3,3,
3,3,3,3,3,3,3,3,3,3,3,3,3,3,3,3,3,3,3,4),(0.,0.136941909255917,0.275838110703575,
0.39883115872138,0.433644442051902,0.521824206739185,0.663226972733855,
0.763151802985195,0.825069431517984,0.861088523135606,1.00600782795853,
1.06292629373921,1.20295657612768,1.26303420748856,1.30095884865492,1.44786363673769,
1.59610960975183,1.62304742329307,1.69648826990486,1.73120226945793,1.76336667330399,
1.91360294448452,1.99760349002108,2.04132627244116,2.20106314648741,2.30292298333825),
 .UNSPECIFIED.);
#695=B_SPLINE_CURVE_WITH_KNOTS('',3,(#34209,#34210,#34211,#34212,#34213,
#34214,#34215,#34216,#34217,#34218,#34219,#34220,#34221,#34222,#34223,#34224,
#34225,#34226,#34227,#34228,#34229,#34230,#34231,#34232,#34233,#34234,#34235,
#34236,#34237,#34238,#34239,#34240,#34241,#34242,#34243,#34244,#34245,#34246,
#34247,#34248,#34249,#34250,#34251),.UNSPECIFIED.,.F.,.F.,(4,3,3,3,3,3,
3,3,3,3,3,3,3,3,4),(7.59244614826264,7.75895334840446,8.24388793267974,
8.72882251695502,9.2137571012303,9.69869168550558,10.1836262697809,10.6685608540561,
11.1534954383314,11.6384300226067,12.123364606882,12.6082991911572,13.0932337754325,
13.5781683597078,13.8756314554422),.UNSPECIFIED.);
#696=B_SPLINE_CURVE_WITH_KNOTS('',3,(#34252,#34253,#34254,#34255,#34256,
#34257,#34258,#34259,#34260,#34261,#34262,#34263,#34264,#34265,#34266,#34267,
#34268,#34269,#34270,#34271,#34272,#34273,#34274,#34275,#34276,#34277,#34278,
#34279,#34280,#34281,#34282,#34283,#34284,#34285,#34286,#34287,#34288,#34289,
#34290,#34291,#34292,#34293,#34294,#34295,#34296,#34297,#34298,#34299,#34300,
#34301,#34302,#34303,#34304,#34305,#34306,#34307,#34308,#34309,#34310,#34311,
#34312,#34313,#34314,#34315,#34316,#34317,#34318,#34319,#34320,#34321,#34322,
#34323,#34324,#34325,#34326,#34327,#34328,#34329,#34330),.UNSPECIFIED.,
 .F.,.F.,(4,3,3,3,3,3,3,3,3,3,3,3,3,3,3,3,3,3,3,3,3,3,3,3,3,3,4),(0.,0.152215561651553,
0.304359114914711,0.444170202609736,0.471986489091098,0.583981290304761,
0.733405394542357,0.837349662722867,0.892797117478666,0.921010855072337,
0.951233541121055,1.09712039568669,1.1491824672644,1.28571136325172,1.34308246731324,
1.37129903319467,1.51452711094878,1.65613232955333,1.69529805121367,1.76334988194098,
1.79789380901942,1.82919292981007,1.96987782454073,2.04822511067641,2.0814756771912,
2.22116640322435,2.31010750305867),.UNSPECIFIED.);
#697=SHAPE_REPRESENTATION_RELATIONSHIP('SRR','None',#34539,#719);
#698=SHAPE_REPRESENTATION_RELATIONSHIP('SRR','None',#34540,#720);
#699=SHAPE_REPRESENTATION_RELATIONSHIP('SRR','None',#34541,#721);
#700=SHAPE_REPRESENTATION_RELATIONSHIP('SRR','None',#34542,#722);
#701=SHAPE_REPRESENTATION_RELATIONSHIP('SRR','None',#34543,#723);
#702=SHAPE_REPRESENTATION_RELATIONSHIP('SRR','None',#34544,#724);
#703=SHAPE_REPRESENTATION_RELATIONSHIP('SRR','None',#34545,#725);
#704=SHAPE_REPRESENTATION_RELATIONSHIP('SRR','None',#34546,#726);
#705=SHAPE_REPRESENTATION_RELATIONSHIP('SRR','None',#34547,#727);
#706=SHAPE_REPRESENTATION_RELATIONSHIP('SRR','None',#34548,#728);
#707=SHAPE_REPRESENTATION_RELATIONSHIP('SRR','None',#34549,#729);
#708=SHAPE_REPRESENTATION_RELATIONSHIP('SRR','None',#34550,#730);
#709=SHAPE_REPRESENTATION_RELATIONSHIP('SRR','None',#34551,#731);
#710=SHAPE_REPRESENTATION_RELATIONSHIP('SRR','None',#34552,#732);
#711=SHAPE_REPRESENTATION_RELATIONSHIP('SRR','None',#34553,#733);
#712=SHAPE_REPRESENTATION_RELATIONSHIP('SRR','None',#34554,#734);
#713=SHAPE_REPRESENTATION_RELATIONSHIP('SRR','None',#34555,#735);
#714=SHAPE_REPRESENTATION_RELATIONSHIP('SRR','None',#34556,#736);
#715=SHAPE_REPRESENTATION_RELATIONSHIP('SRR','None',#34558,#737);
#716=SHAPE_REPRESENTATION_RELATIONSHIP('SRR','None',#34560,#738);
#717=SHAPE_REPRESENTATION_RELATIONSHIP('SRR','None',#34562,#739);
#718=SHAPE_REPRESENTATION_RELATIONSHIP('SRR','None',#34564,#740);
#719=ADVANCED_BREP_SHAPE_REPRESENTATION('',(#771),#34407);
#720=ADVANCED_BREP_SHAPE_REPRESENTATION('',(#772),#34408);
#721=ADVANCED_BREP_SHAPE_REPRESENTATION('',(#773),#34409);
#722=ADVANCED_BREP_SHAPE_REPRESENTATION('',(#774),#34410);
#723=ADVANCED_BREP_SHAPE_REPRESENTATION('',(#775,#776,#777),#34411);
#724=ADVANCED_BREP_SHAPE_REPRESENTATION('',(#778,#779,#780),#34412);
#725=ADVANCED_BREP_SHAPE_REPRESENTATION('',(#781),#34413);
#726=ADVANCED_BREP_SHAPE_REPRESENTATION('',(#782),#34414);
#727=ADVANCED_BREP_SHAPE_REPRESENTATION('',(#783,#784,#785),#34415);
#728=ADVANCED_BREP_SHAPE_REPRESENTATION('',(#786,#787,#788),#34416);
#729=ADVANCED_BREP_SHAPE_REPRESENTATION('',(#789),#34417);
#730=ADVANCED_BREP_SHAPE_REPRESENTATION('',(#790),#34418);
#731=ADVANCED_BREP_SHAPE_REPRESENTATION('',(#791),#34419);
#732=ADVANCED_BREP_SHAPE_REPRESENTATION('',(#792),#34420);
#733=ADVANCED_BREP_SHAPE_REPRESENTATION('',(#205),#34421);
#734=ADVANCED_BREP_SHAPE_REPRESENTATION('',(#206),#34422);
#735=ADVANCED_BREP_SHAPE_REPRESENTATION('',(#793),#34423);
#736=ADVANCED_BREP_SHAPE_REPRESENTATION('',(#794),#34424);
#737=ADVANCED_BREP_SHAPE_REPRESENTATION('',(#795),#34426);
#738=ADVANCED_BREP_SHAPE_REPRESENTATION('',(#796),#34428);
#739=ADVANCED_BREP_SHAPE_REPRESENTATION('',(#797),#34430);
#740=ADVANCED_BREP_SHAPE_REPRESENTATION('',(#798),#34432);
#741=STYLED_ITEM('',(#34722),#771);
#742=STYLED_ITEM('',(#34757),#772);
#743=STYLED_ITEM('',(#34729),#773);
#744=STYLED_ITEM('',(#34729),#774);
#745=STYLED_ITEM('',(#34729),#775);
#746=STYLED_ITEM('',(#34729),#776);
#747=STYLED_ITEM('',(#34729),#777);
#748=STYLED_ITEM('',(#34729),#778);
#749=STYLED_ITEM('',(#34729),#779);
#750=STYLED_ITEM('',(#34729),#780);
#751=STYLED_ITEM('',(#34736),#781);
#752=STYLED_ITEM('',(#34736),#782);
#753=STYLED_ITEM('',(#34757),#783);
#754=STYLED_ITEM('',(#34757),#784);
#755=STYLED_ITEM('',(#34757),#785);
#756=STYLED_ITEM('',(#34729),#786);
#757=STYLED_ITEM('',(#34729),#787);
#758=STYLED_ITEM('',(#34729),#788);
#759=STYLED_ITEM('',(#34736),#789);
#760=STYLED_ITEM('',(#34736),#790);
#761=STYLED_ITEM('',(#34736),#791);
#762=STYLED_ITEM('',(#34736),#792);
#763=STYLED_ITEM('',(#34750),#205);
#764=STYLED_ITEM('',(#34750),#206);
#765=STYLED_ITEM('',(#34750),#793);
#766=STYLED_ITEM('',(#34750),#794);
#767=STYLED_ITEM('',(#34750),#795);
#768=STYLED_ITEM('',(#34750),#796);
#769=STYLED_ITEM('',(#34750),#797);
#770=STYLED_ITEM('',(#34750),#798);
#771=MANIFOLD_SOLID_BREP('Body1',#8768);
#772=MANIFOLD_SOLID_BREP('Body1',#8769);
#773=MANIFOLD_SOLID_BREP('Body1',#8770);
#774=MANIFOLD_SOLID_BREP('Body1',#8771);
#775=MANIFOLD_SOLID_BREP('Body1',#8772);
#776=MANIFOLD_SOLID_BREP('Body2',#8773);
#777=MANIFOLD_SOLID_BREP('Body3',#8774);
#778=MANIFOLD_SOLID_BREP('Body1',#8775);
#779=MANIFOLD_SOLID_BREP('Body2',#8776);
#780=MANIFOLD_SOLID_BREP('Body3',#8777);
#781=MANIFOLD_SOLID_BREP('Body1',#8778);
#782=MANIFOLD_SOLID_BREP('Body1',#8779);
#783=MANIFOLD_SOLID_BREP('Body1',#8780);
#784=MANIFOLD_SOLID_BREP('Body2',#8781);
#785=MANIFOLD_SOLID_BREP('Body3',#8782);
#786=MANIFOLD_SOLID_BREP('Body1',#8783);
#787=MANIFOLD_SOLID_BREP('Body2',#8784);
#788=MANIFOLD_SOLID_BREP('Body3',#8785);
#789=MANIFOLD_SOLID_BREP('Body1',#8786);
#790=MANIFOLD_SOLID_BREP('Body1',#8787);
#791=MANIFOLD_SOLID_BREP('Body1',#8788);
#792=MANIFOLD_SOLID_BREP('Body1',#8789);
#793=MANIFOLD_SOLID_BREP('Body1',#8794);
#794=MANIFOLD_SOLID_BREP('Body1',#8795);
#795=MANIFOLD_SOLID_BREP('Body1',#8796);
#796=MANIFOLD_SOLID_BREP('Body1',#8797);
#797=MANIFOLD_SOLID_BREP('Body1',#8798);
#798=MANIFOLD_SOLID_BREP('Body1',#8799);
#799=FACE_BOUND('',#1544,.T.);
#800=FACE_BOUND('',#1545,.T.);
#801=FACE_BOUND('',#1546,.T.);
#802=FACE_BOUND('',#1547,.T.);
#803=FACE_BOUND('',#1548,.T.);
#804=FACE_BOUND('',#1549,.T.);
#805=FACE_BOUND('',#1551,.T.);
#806=FACE_BOUND('',#1552,.T.);
#807=FACE_BOUND('',#1553,.T.);
#808=FACE_BOUND('',#1554,.T.);
#809=FACE_BOUND('',#1750,.T.);
#810=FACE_BOUND('',#1751,.T.);
#811=FACE_BOUND('',#1752,.T.);
#812=FACE_BOUND('',#1753,.T.);
#813=FACE_BOUND('',#1754,.T.);
#814=FACE_BOUND('',#1755,.T.);
#815=FACE_BOUND('',#1756,.T.);
#816=FACE_BOUND('',#1759,.T.);
#817=FACE_BOUND('',#1760,.T.);
#818=FACE_BOUND('',#1761,.T.);
#819=FACE_BOUND('',#1762,.T.);
#820=FACE_BOUND('',#1763,.T.);
#821=FACE_BOUND('',#1764,.T.);
#822=FACE_BOUND('',#1783,.T.);
#823=FACE_BOUND('',#1787,.T.);
#824=FACE_BOUND('',#1797,.T.);
#825=FACE_BOUND('',#1800,.T.);
#826=FACE_BOUND('',#1806,.T.);
#827=FACE_BOUND('',#1809,.T.);
#828=FACE_BOUND('',#1821,.T.);
#829=FACE_BOUND('',#1824,.T.);
#830=FACE_BOUND('',#1830,.T.);
#831=FACE_BOUND('',#1833,.T.);
#832=FACE_BOUND('',#1857,.T.);
#833=FACE_BOUND('',#1861,.T.);
#834=FACE_BOUND('',#1869,.T.);
#835=FACE_BOUND('',#1872,.T.);
#836=FACE_BOUND('',#1878,.T.);
#837=FACE_BOUND('',#1881,.T.);
#838=FACE_BOUND('',#1893,.T.);
#839=FACE_BOUND('',#1896,.T.);
#840=FACE_BOUND('',#1902,.T.);
#841=FACE_BOUND('',#1905,.T.);
#842=FACE_BOUND('',#1946,.T.);
#843=FACE_BOUND('',#1958,.T.);
#844=FACE_BOUND('',#1966,.T.);
#845=FACE_BOUND('',#1972,.T.);
#846=FACE_BOUND('',#1974,.T.);
#847=FACE_BOUND('',#1985,.T.);
#848=FACE_BOUND('',#1987,.T.);
#849=FACE_BOUND('',#2000,.T.);
#850=FACE_BOUND('',#2009,.T.);
#851=FACE_BOUND('',#2022,.T.);
#852=FACE_BOUND('',#2031,.T.);
#853=FACE_BOUND('',#2044,.T.);
#854=FACE_BOUND('',#2053,.T.);
#855=FACE_BOUND('',#2066,.T.);
#856=FACE_BOUND('',#2075,.T.);
#857=PLANE('',#9049);
#858=PLANE('',#9053);
#859=PLANE('',#9066);
#860=PLANE('',#9067);
#861=PLANE('',#9068);
#862=PLANE('',#9069);
#863=PLANE('',#9070);
#864=PLANE('',#9071);
#865=PLANE('',#9281);
#866=PLANE('',#9286);
#867=PLANE('',#9288);
#868=PLANE('',#9295);
#869=PLANE('',#9296);
#870=PLANE('',#9301);
#871=PLANE('',#9302);
#872=PLANE('',#9307);
#873=PLANE('',#9310);
#874=PLANE('',#9317);
#875=PLANE('',#9318);
#876=PLANE('',#9319);
#877=PLANE('',#9320);
#878=PLANE('',#9321);
#879=PLANE('',#9322);
#880=PLANE('',#9323);
#881=PLANE('',#9324);
#882=PLANE('',#9329);
#883=PLANE('',#9333);
#884=PLANE('',#9334);
#885=PLANE('',#9335);
#886=PLANE('',#9336);
#887=PLANE('',#9337);
#888=PLANE('',#9338);
#889=PLANE('',#9342);
#890=PLANE('',#9343);
#891=PLANE('',#9344);
#892=PLANE('',#9345);
#893=PLANE('',#9346);
#894=PLANE('',#9347);
#895=PLANE('',#9352);
#896=PLANE('',#9354);
#897=PLANE('',#9355);
#898=PLANE('',#9358);
#899=PLANE('',#9362);
#900=PLANE('',#9363);
#901=PLANE('',#9364);
#902=PLANE('',#9365);
#903=PLANE('',#9366);
#904=PLANE('',#9367);
#905=PLANE('',#9371);
#906=PLANE('',#9372);
#907=PLANE('',#9373);
#908=PLANE('',#9374);
#909=PLANE('',#9375);
#910=PLANE('',#9376);
#911=PLANE('',#9378);
#912=PLANE('',#9379);
#913=PLANE('',#9380);
#914=PLANE('',#9387);
#915=PLANE('',#9389);
#916=PLANE('',#9390);
#917=PLANE('',#9391);
#918=PLANE('',#9398);
#919=PLANE('',#9405);
#920=PLANE('',#9406);
#921=PLANE('',#9408);
#922=PLANE('',#9409);
#923=PLANE('',#9416);
#924=PLANE('',#9417);
#925=PLANE('',#9418);
#926=PLANE('',#9419);
#927=PLANE('',#9420);
#928=PLANE('',#9421);
#929=PLANE('',#9422);
#930=PLANE('',#9423);
#931=PLANE('',#9429);
#932=PLANE('',#9430);
#933=PLANE('',#9431);
#934=PLANE('',#9432);
#935=PLANE('',#9433);
#936=PLANE('',#9434);
#937=PLANE('',#9438);
#938=PLANE('',#9439);
#939=PLANE('',#9440);
#940=PLANE('',#9441);
#941=PLANE('',#9442);
#942=PLANE('',#9443);
#943=PLANE('',#9448);
#944=PLANE('',#9450);
#945=PLANE('',#9451);
#946=PLANE('',#9454);
#947=PLANE('',#9458);
#948=PLANE('',#9459);
#949=PLANE('',#9460);
#950=PLANE('',#9461);
#951=PLANE('',#9462);
#952=PLANE('',#9463);
#953=PLANE('',#9467);
#954=PLANE('',#9468);
#955=PLANE('',#9469);
#956=PLANE('',#9470);
#957=PLANE('',#9471);
#958=PLANE('',#9472);
#959=PLANE('',#9474);
#960=PLANE('',#9475);
#961=PLANE('',#9476);
#962=PLANE('',#9483);
#963=PLANE('',#9485);
#964=PLANE('',#9486);
#965=PLANE('',#9487);
#966=PLANE('',#9494);
#967=PLANE('',#9496);
#968=PLANE('',#9497);
#969=PLANE('',#9498);
#970=PLANE('',#9499);
#971=PLANE('',#9500);
#972=PLANE('',#9501);
#973=PLANE('',#9503);
#974=PLANE('',#9504);
#975=PLANE('',#9505);
#976=PLANE('',#9506);
#977=PLANE('',#9507);
#978=PLANE('',#9508);
#979=PLANE('',#9510);
#980=PLANE('',#9511);
#981=PLANE('',#9512);
#982=PLANE('',#9513);
#983=PLANE('',#9514);
#984=PLANE('',#9515);
#985=PLANE('',#9516);
#986=PLANE('',#9517);
#987=PLANE('',#9518);
#988=PLANE('',#9520);
#989=PLANE('',#9528);
#990=PLANE('',#9534);
#991=PLANE('',#9535);
#992=PLANE('',#9536);
#993=PLANE('',#9537);
#994=PLANE('',#9538);
#995=PLANE('',#9539);
#996=PLANE('',#9540);
#997=PLANE('',#9541);
#998=PLANE('',#9542);
#999=PLANE('',#9547);
#1000=PLANE('',#9548);
#1001=PLANE('',#9556);
#1002=PLANE('',#9568);
#1003=PLANE('',#9569);
#1004=PLANE('',#9575);
#1005=PLANE('',#9576);
#1006=PLANE('',#9577);
#1007=PLANE('',#9581);
#1008=PLANE('',#9582);
#1009=PLANE('',#9583);
#1010=PLANE('',#9584);
#1011=PLANE('',#9585);
#1012=PLANE('',#9635);
#1013=PLANE('',#9637);
#1014=PLANE('',#9638);
#1015=PLANE('',#9639);
#1016=PLANE('',#9640);
#1017=PLANE('',#9641);
#1018=PLANE('',#9642);
#1019=PLANE('',#9643);
#1020=PLANE('',#9660);
#1021=PLANE('',#9662);
#1022=PLANE('',#9663);
#1023=PLANE('',#9664);
#1024=PLANE('',#9665);
#1025=PLANE('',#9666);
#1026=PLANE('',#9667);
#1027=PLANE('',#9668);
#1028=PLANE('',#9685);
#1029=PLANE('',#9687);
#1030=PLANE('',#9688);
#1031=PLANE('',#9689);
#1032=PLANE('',#9690);
#1033=PLANE('',#9691);
#1034=PLANE('',#9692);
#1035=PLANE('',#9693);
#1036=PLANE('',#9710);
#1037=PLANE('',#9712);
#1038=PLANE('',#9713);
#1039=PLANE('',#9714);
#1040=PLANE('',#9715);
#1041=PLANE('',#9716);
#1042=PLANE('',#9717);
#1043=PLANE('',#9718);
#1044=FACE_OUTER_BOUND('',#1531,.T.);
#1045=FACE_OUTER_BOUND('',#1532,.T.);
#1046=FACE_OUTER_BOUND('',#1533,.T.);
#1047=FACE_OUTER_BOUND('',#1534,.T.);
#1048=FACE_OUTER_BOUND('',#1535,.T.);
#1049=FACE_OUTER_BOUND('',#1536,.T.);
#1050=FACE_OUTER_BOUND('',#1537,.T.);
#1051=FACE_OUTER_BOUND('',#1538,.T.);
#1052=FACE_OUTER_BOUND('',#1539,.T.);
#1053=FACE_OUTER_BOUND('',#1540,.T.);
#1054=FACE_OUTER_BOUND('',#1541,.T.);
#1055=FACE_OUTER_BOUND('',#1542,.T.);
#1056=FACE_OUTER_BOUND('',#1543,.T.);
#1057=FACE_OUTER_BOUND('',#1550,.T.);
#1058=FACE_OUTER_BOUND('',#1555,.T.);
#1059=FACE_OUTER_BOUND('',#1556,.T.);
#1060=FACE_OUTER_BOUND('',#1557,.T.);
#1061=FACE_OUTER_BOUND('',#1558,.T.);
#1062=FACE_OUTER_BOUND('',#1559,.T.);
#1063=FACE_OUTER_BOUND('',#1560,.T.);
#1064=FACE_OUTER_BOUND('',#1561,.T.);
#1065=FACE_OUTER_BOUND('',#1562,.T.);
#1066=FACE_OUTER_BOUND('',#1563,.T.);
#1067=FACE_OUTER_BOUND('',#1564,.T.);
#1068=FACE_OUTER_BOUND('',#1565,.T.);
#1069=FACE_OUTER_BOUND('',#1566,.T.);
#1070=FACE_OUTER_BOUND('',#1567,.T.);
#1071=FACE_OUTER_BOUND('',#1568,.T.);
#1072=FACE_OUTER_BOUND('',#1569,.T.);
#1073=FACE_OUTER_BOUND('',#1570,.T.);
#1074=FACE_OUTER_BOUND('',#1571,.T.);
#1075=FACE_OUTER_BOUND('',#1572,.T.);
#1076=FACE_OUTER_BOUND('',#1573,.T.);
#1077=FACE_OUTER_BOUND('',#1574,.T.);
#1078=FACE_OUTER_BOUND('',#1575,.T.);
#1079=FACE_OUTER_BOUND('',#1576,.T.);
#1080=FACE_OUTER_BOUND('',#1577,.T.);
#1081=FACE_OUTER_BOUND('',#1578,.T.);
#1082=FACE_OUTER_BOUND('',#1579,.T.);
#1083=FACE_OUTER_BOUND('',#1580,.T.);
#1084=FACE_OUTER_BOUND('',#1581,.T.);
#1085=FACE_OUTER_BOUND('',#1582,.T.);
#1086=FACE_OUTER_BOUND('',#1583,.T.);
#1087=FACE_OUTER_BOUND('',#1584,.T.);
#1088=FACE_OUTER_BOUND('',#1585,.T.);
#1089=FACE_OUTER_BOUND('',#1586,.T.);
#1090=FACE_OUTER_BOUND('',#1587,.T.);
#1091=FACE_OUTER_BOUND('',#1588,.T.);
#1092=FACE_OUTER_BOUND('',#1589,.T.);
#1093=FACE_OUTER_BOUND('',#1590,.T.);
#1094=FACE_OUTER_BOUND('',#1591,.T.);
#1095=FACE_OUTER_BOUND('',#1592,.T.);
#1096=FACE_OUTER_BOUND('',#1593,.T.);
#1097=FACE_OUTER_BOUND('',#1594,.T.);
#1098=FACE_OUTER_BOUND('',#1595,.T.);
#1099=FACE_OUTER_BOUND('',#1596,.T.);
#1100=FACE_OUTER_BOUND('',#1597,.T.);
#1101=FACE_OUTER_BOUND('',#1598,.T.);
#1102=FACE_OUTER_BOUND('',#1599,.T.);
#1103=FACE_OUTER_BOUND('',#1600,.T.);
#1104=FACE_OUTER_BOUND('',#1601,.T.);
#1105=FACE_OUTER_BOUND('',#1602,.T.);
#1106=FACE_OUTER_BOUND('',#1603,.T.);
#1107=FACE_OUTER_BOUND('',#1604,.T.);
#1108=FACE_OUTER_BOUND('',#1605,.T.);
#1109=FACE_OUTER_BOUND('',#1606,.T.);
#1110=FACE_OUTER_BOUND('',#1607,.T.);
#1111=FACE_OUTER_BOUND('',#1608,.T.);
#1112=FACE_OUTER_BOUND('',#1609,.T.);
#1113=FACE_OUTER_BOUND('',#1610,.T.);
#1114=FACE_OUTER_BOUND('',#1611,.T.);
#1115=FACE_OUTER_BOUND('',#1612,.T.);
#1116=FACE_OUTER_BOUND('',#1613,.T.);
#1117=FACE_OUTER_BOUND('',#1614,.T.);
#1118=FACE_OUTER_BOUND('',#1615,.T.);
#1119=FACE_OUTER_BOUND('',#1616,.T.);
#1120=FACE_OUTER_BOUND('',#1617,.T.);
#1121=FACE_OUTER_BOUND('',#1618,.T.);
#1122=FACE_OUTER_BOUND('',#1619,.T.);
#1123=FACE_OUTER_BOUND('',#1620,.T.);
#1124=FACE_OUTER_BOUND('',#1621,.T.);
#1125=FACE_OUTER_BOUND('',#1622,.T.);
#1126=FACE_OUTER_BOUND('',#1623,.T.);
#1127=FACE_OUTER_BOUND('',#1624,.T.);
#1128=FACE_OUTER_BOUND('',#1625,.T.);
#1129=FACE_OUTER_BOUND('',#1626,.T.);
#1130=FACE_OUTER_BOUND('',#1627,.T.);
#1131=FACE_OUTER_BOUND('',#1628,.T.);
#1132=FACE_OUTER_BOUND('',#1629,.T.);
#1133=FACE_OUTER_BOUND('',#1630,.T.);
#1134=FACE_OUTER_BOUND('',#1631,.T.);
#1135=FACE_OUTER_BOUND('',#1632,.T.);
#1136=FACE_OUTER_BOUND('',#1633,.T.);
#1137=FACE_OUTER_BOUND('',#1634,.T.);
#1138=FACE_OUTER_BOUND('',#1635,.T.);
#1139=FACE_OUTER_BOUND('',#1636,.T.);
#1140=FACE_OUTER_BOUND('',#1637,.T.);
#1141=FACE_OUTER_BOUND('',#1638,.T.);
#1142=FACE_OUTER_BOUND('',#1639,.T.);
#1143=FACE_OUTER_BOUND('',#1640,.T.);
#1144=FACE_OUTER_BOUND('',#1641,.T.);
#1145=FACE_OUTER_BOUND('',#1642,.T.);
#1146=FACE_OUTER_BOUND('',#1643,.T.);
#1147=FACE_OUTER_BOUND('',#1644,.T.);
#1148=FACE_OUTER_BOUND('',#1645,.T.);
#1149=FACE_OUTER_BOUND('',#1646,.T.);
#1150=FACE_OUTER_BOUND('',#1647,.T.);
#1151=FACE_OUTER_BOUND('',#1648,.T.);
#1152=FACE_OUTER_BOUND('',#1649,.T.);
#1153=FACE_OUTER_BOUND('',#1650,.T.);
#1154=FACE_OUTER_BOUND('',#1651,.T.);
#1155=FACE_OUTER_BOUND('',#1652,.T.);
#1156=FACE_OUTER_BOUND('',#1653,.T.);
#1157=FACE_OUTER_BOUND('',#1654,.T.);
#1158=FACE_OUTER_BOUND('',#1655,.T.);
#1159=FACE_OUTER_BOUND('',#1656,.T.);
#1160=FACE_OUTER_BOUND('',#1657,.T.);
#1161=FACE_OUTER_BOUND('',#1658,.T.);
#1162=FACE_OUTER_BOUND('',#1659,.T.);
#1163=FACE_OUTER_BOUND('',#1660,.T.);
#1164=FACE_OUTER_BOUND('',#1661,.T.);
#1165=FACE_OUTER_BOUND('',#1662,.T.);
#1166=FACE_OUTER_BOUND('',#1663,.T.);
#1167=FACE_OUTER_BOUND('',#1664,.T.);
#1168=FACE_OUTER_BOUND('',#1665,.T.);
#1169=FACE_OUTER_BOUND('',#1666,.T.);
#1170=FACE_OUTER_BOUND('',#1667,.T.);
#1171=FACE_OUTER_BOUND('',#1668,.T.);
#1172=FACE_OUTER_BOUND('',#1669,.T.);
#1173=FACE_OUTER_BOUND('',#1670,.T.);
#1174=FACE_OUTER_BOUND('',#1671,.T.);
#1175=FACE_OUTER_BOUND('',#1672,.T.);
#1176=FACE_OUTER_BOUND('',#1673,.T.);
#1177=FACE_OUTER_BOUND('',#1674,.T.);
#1178=FACE_OUTER_BOUND('',#1675,.T.);
#1179=FACE_OUTER_BOUND('',#1676,.T.);
#1180=FACE_OUTER_BOUND('',#1677,.T.);
#1181=FACE_OUTER_BOUND('',#1678,.T.);
#1182=FACE_OUTER_BOUND('',#1679,.T.);
#1183=FACE_OUTER_BOUND('',#1680,.T.);
#1184=FACE_OUTER_BOUND('',#1681,.T.);
#1185=FACE_OUTER_BOUND('',#1682,.T.);
#1186=FACE_OUTER_BOUND('',#1683,.T.);
#1187=FACE_OUTER_BOUND('',#1684,.T.);
#1188=FACE_OUTER_BOUND('',#1685,.T.);
#1189=FACE_OUTER_BOUND('',#1686,.T.);
#1190=FACE_OUTER_BOUND('',#1687,.T.);
#1191=FACE_OUTER_BOUND('',#1688,.T.);
#1192=FACE_OUTER_BOUND('',#1689,.T.);
#1193=FACE_OUTER_BOUND('',#1690,.T.);
#1194=FACE_OUTER_BOUND('',#1691,.T.);
#1195=FACE_OUTER_BOUND('',#1692,.T.);
#1196=FACE_OUTER_BOUND('',#1693,.T.);
#1197=FACE_OUTER_BOUND('',#1694,.T.);
#1198=FACE_OUTER_BOUND('',#1695,.T.);
#1199=FACE_OUTER_BOUND('',#1696,.T.);
#1200=FACE_OUTER_BOUND('',#1697,.T.);
#1201=FACE_OUTER_BOUND('',#1698,.T.);
#1202=FACE_OUTER_BOUND('',#1699,.T.);
#1203=FACE_OUTER_BOUND('',#1700,.T.);
#1204=FACE_OUTER_BOUND('',#1701,.T.);
#1205=FACE_OUTER_BOUND('',#1702,.T.);
#1206=FACE_OUTER_BOUND('',#1703,.T.);
#1207=FACE_OUTER_BOUND('',#1704,.T.);
#1208=FACE_OUTER_BOUND('',#1705,.T.);
#1209=FACE_OUTER_BOUND('',#1706,.T.);
#1210=FACE_OUTER_BOUND('',#1707,.T.);
#1211=FACE_OUTER_BOUND('',#1708,.T.);
#1212=FACE_OUTER_BOUND('',#1709,.T.);
#1213=FACE_OUTER_BOUND('',#1710,.T.);
#1214=FACE_OUTER_BOUND('',#1711,.T.);
#1215=FACE_OUTER_BOUND('',#1712,.T.);
#1216=FACE_OUTER_BOUND('',#1713,.T.);
#1217=FACE_OUTER_BOUND('',#1714,.T.);
#1218=FACE_OUTER_BOUND('',#1715,.T.);
#1219=FACE_OUTER_BOUND('',#1716,.T.);
#1220=FACE_OUTER_BOUND('',#1717,.T.);
#1221=FACE_OUTER_BOUND('',#1718,.T.);
#1222=FACE_OUTER_BOUND('',#1719,.T.);
#1223=FACE_OUTER_BOUND('',#1720,.T.);
#1224=FACE_OUTER_BOUND('',#1721,.T.);
#1225=FACE_OUTER_BOUND('',#1722,.T.);
#1226=FACE_OUTER_BOUND('',#1723,.T.);
#1227=FACE_OUTER_BOUND('',#1724,.T.);
#1228=FACE_OUTER_BOUND('',#1725,.T.);
#1229=FACE_OUTER_BOUND('',#1726,.T.);
#1230=FACE_OUTER_BOUND('',#1727,.T.);
#1231=FACE_OUTER_BOUND('',#1728,.T.);
#1232=FACE_OUTER_BOUND('',#1729,.T.);
#1233=FACE_OUTER_BOUND('',#1730,.T.);
#1234=FACE_OUTER_BOUND('',#1731,.T.);
#1235=FACE_OUTER_BOUND('',#1732,.T.);
#1236=FACE_OUTER_BOUND('',#1733,.T.);
#1237=FACE_OUTER_BOUND('',#1734,.T.);
#1238=FACE_OUTER_BOUND('',#1735,.T.);
#1239=FACE_OUTER_BOUND('',#1736,.T.);
#1240=FACE_OUTER_BOUND('',#1737,.T.);
#1241=FACE_OUTER_BOUND('',#1738,.T.);
#1242=FACE_OUTER_BOUND('',#1739,.T.);
#1243=FACE_OUTER_BOUND('',#1740,.T.);
#1244=FACE_OUTER_BOUND('',#1741,.T.);
#1245=FACE_OUTER_BOUND('',#1742,.T.);
#1246=FACE_OUTER_BOUND('',#1743,.T.);
#1247=FACE_OUTER_BOUND('',#1744,.T.);
#1248=FACE_OUTER_BOUND('',#1745,.T.);
#1249=FACE_OUTER_BOUND('',#1746,.T.);
#1250=FACE_OUTER_BOUND('',#1747,.T.);
#1251=FACE_OUTER_BOUND('',#1748,.T.);
#1252=FACE_OUTER_BOUND('',#1749,.T.);
#1253=FACE_OUTER_BOUND('',#1757,.T.);
#1254=FACE_OUTER_BOUND('',#1758,.T.);
#1255=FACE_OUTER_BOUND('',#1765,.T.);
#1256=FACE_OUTER_BOUND('',#1766,.T.);
#1257=FACE_OUTER_BOUND('',#1767,.T.);
#1258=FACE_OUTER_BOUND('',#1768,.T.);
#1259=FACE_OUTER_BOUND('',#1769,.T.);
#1260=FACE_OUTER_BOUND('',#1770,.T.);
#1261=FACE_OUTER_BOUND('',#1771,.T.);
#1262=FACE_OUTER_BOUND('',#1772,.T.);
#1263=FACE_OUTER_BOUND('',#1773,.T.);
#1264=FACE_OUTER_BOUND('',#1774,.T.);
#1265=FACE_OUTER_BOUND('',#1775,.T.);
#1266=FACE_OUTER_BOUND('',#1776,.T.);
#1267=FACE_OUTER_BOUND('',#1777,.T.);
#1268=FACE_OUTER_BOUND('',#1778,.T.);
#1269=FACE_OUTER_BOUND('',#1779,.T.);
#1270=FACE_OUTER_BOUND('',#1780,.T.);
#1271=FACE_OUTER_BOUND('',#1781,.T.);
#1272=FACE_OUTER_BOUND('',#1782,.T.);
#1273=FACE_OUTER_BOUND('',#1784,.T.);
#1274=FACE_OUTER_BOUND('',#1785,.T.);
#1275=FACE_OUTER_BOUND('',#1786,.T.);
#1276=FACE_OUTER_BOUND('',#1788,.T.);
#1277=FACE_OUTER_BOUND('',#1789,.T.);
#1278=FACE_OUTER_BOUND('',#1790,.T.);
#1279=FACE_OUTER_BOUND('',#1791,.T.);
#1280=FACE_OUTER_BOUND('',#1792,.T.);
#1281=FACE_OUTER_BOUND('',#1793,.T.);
#1282=FACE_OUTER_BOUND('',#1794,.T.);
#1283=FACE_OUTER_BOUND('',#1795,.T.);
#1284=FACE_OUTER_BOUND('',#1796,.T.);
#1285=FACE_OUTER_BOUND('',#1798,.T.);
#1286=FACE_OUTER_BOUND('',#1799,.T.);
#1287=FACE_OUTER_BOUND('',#1801,.T.);
#1288=FACE_OUTER_BOUND('',#1802,.T.);
#1289=FACE_OUTER_BOUND('',#1803,.T.);
#1290=FACE_OUTER_BOUND('',#1804,.T.);
#1291=FACE_OUTER_BOUND('',#1805,.T.);
#1292=FACE_OUTER_BOUND('',#1807,.T.);
#1293=FACE_OUTER_BOUND('',#1808,.T.);
#1294=FACE_OUTER_BOUND('',#1810,.T.);
#1295=FACE_OUTER_BOUND('',#1811,.T.);
#1296=FACE_OUTER_BOUND('',#1812,.T.);
#1297=FACE_OUTER_BOUND('',#1813,.T.);
#1298=FACE_OUTER_BOUND('',#1814,.T.);
#1299=FACE_OUTER_BOUND('',#1815,.T.);
#1300=FACE_OUTER_BOUND('',#1816,.T.);
#1301=FACE_OUTER_BOUND('',#1817,.T.);
#1302=FACE_OUTER_BOUND('',#1818,.T.);
#1303=FACE_OUTER_BOUND('',#1819,.T.);
#1304=FACE_OUTER_BOUND('',#1820,.T.);
#1305=FACE_OUTER_BOUND('',#1822,.T.);
#1306=FACE_OUTER_BOUND('',#1823,.T.);
#1307=FACE_OUTER_BOUND('',#1825,.T.);
#1308=FACE_OUTER_BOUND('',#1826,.T.);
#1309=FACE_OUTER_BOUND('',#1827,.T.);
#1310=FACE_OUTER_BOUND('',#1828,.T.);
#1311=FACE_OUTER_BOUND('',#1829,.T.);
#1312=FACE_OUTER_BOUND('',#1831,.T.);
#1313=FACE_OUTER_BOUND('',#1832,.T.);
#1314=FACE_OUTER_BOUND('',#1834,.T.);
#1315=FACE_OUTER_BOUND('',#1835,.T.);
#1316=FACE_OUTER_BOUND('',#1836,.T.);
#1317=FACE_OUTER_BOUND('',#1837,.T.);
#1318=FACE_OUTER_BOUND('',#1838,.T.);
#1319=FACE_OUTER_BOUND('',#1839,.T.);
#1320=FACE_OUTER_BOUND('',#1840,.T.);
#1321=FACE_OUTER_BOUND('',#1841,.T.);
#1322=FACE_OUTER_BOUND('',#1842,.T.);
#1323=FACE_OUTER_BOUND('',#1843,.T.);
#1324=FACE_OUTER_BOUND('',#1844,.T.);
#1325=FACE_OUTER_BOUND('',#1845,.T.);
#1326=FACE_OUTER_BOUND('',#1846,.T.);
#1327=FACE_OUTER_BOUND('',#1847,.T.);
#1328=FACE_OUTER_BOUND('',#1848,.T.);
#1329=FACE_OUTER_BOUND('',#1849,.T.);
#1330=FACE_OUTER_BOUND('',#1850,.T.);
#1331=FACE_OUTER_BOUND('',#1851,.T.);
#1332=FACE_OUTER_BOUND('',#1852,.T.);
#1333=FACE_OUTER_BOUND('',#1853,.T.);
#1334=FACE_OUTER_BOUND('',#1854,.T.);
#1335=FACE_OUTER_BOUND('',#1855,.T.);
#1336=FACE_OUTER_BOUND('',#1856,.T.);
#1337=FACE_OUTER_BOUND('',#1858,.T.);
#1338=FACE_OUTER_BOUND('',#1859,.T.);
#1339=FACE_OUTER_BOUND('',#1860,.T.);
#1340=FACE_OUTER_BOUND('',#1862,.T.);
#1341=FACE_OUTER_BOUND('',#1863,.T.);
#1342=FACE_OUTER_BOUND('',#1864,.T.);
#1343=FACE_OUTER_BOUND('',#1865,.T.);
#1344=FACE_OUTER_BOUND('',#1866,.T.);
#1345=FACE_OUTER_BOUND('',#1867,.T.);
#1346=FACE_OUTER_BOUND('',#1868,.T.);
#1347=FACE_OUTER_BOUND('',#1870,.T.);
#1348=FACE_OUTER_BOUND('',#1871,.T.);
#1349=FACE_OUTER_BOUND('',#1873,.T.);
#1350=FACE_OUTER_BOUND('',#1874,.T.);
#1351=FACE_OUTER_BOUND('',#1875,.T.);
#1352=FACE_OUTER_BOUND('',#1876,.T.);
#1353=FACE_OUTER_BOUND('',#1877,.T.);
#1354=FACE_OUTER_BOUND('',#1879,.T.);
#1355=FACE_OUTER_BOUND('',#1880,.T.);
#1356=FACE_OUTER_BOUND('',#1882,.T.);
#1357=FACE_OUTER_BOUND('',#1883,.T.);
#1358=FACE_OUTER_BOUND('',#1884,.T.);
#1359=FACE_OUTER_BOUND('',#1885,.T.);
#1360=FACE_OUTER_BOUND('',#1886,.T.);
#1361=FACE_OUTER_BOUND('',#1887,.T.);
#1362=FACE_OUTER_BOUND('',#1888,.T.);
#1363=FACE_OUTER_BOUND('',#1889,.T.);
#1364=FACE_OUTER_BOUND('',#1890,.T.);
#1365=FACE_OUTER_BOUND('',#1891,.T.);
#1366=FACE_OUTER_BOUND('',#1892,.T.);
#1367=FACE_OUTER_BOUND('',#1894,.T.);
#1368=FACE_OUTER_BOUND('',#1895,.T.);
#1369=FACE_OUTER_BOUND('',#1897,.T.);
#1370=FACE_OUTER_BOUND('',#1898,.T.);
#1371=FACE_OUTER_BOUND('',#1899,.T.);
#1372=FACE_OUTER_BOUND('',#1900,.T.);
#1373=FACE_OUTER_BOUND('',#1901,.T.);
#1374=FACE_OUTER_BOUND('',#1903,.T.);
#1375=FACE_OUTER_BOUND('',#1904,.T.);
#1376=FACE_OUTER_BOUND('',#1906,.T.);
#1377=FACE_OUTER_BOUND('',#1907,.T.);
#1378=FACE_OUTER_BOUND('',#1908,.T.);
#1379=FACE_OUTER_BOUND('',#1909,.T.);
#1380=FACE_OUTER_BOUND('',#1910,.T.);
#1381=FACE_OUTER_BOUND('',#1911,.T.);
#1382=FACE_OUTER_BOUND('',#1912,.T.);
#1383=FACE_OUTER_BOUND('',#1913,.T.);
#1384=FACE_OUTER_BOUND('',#1914,.T.);
#1385=FACE_OUTER_BOUND('',#1915,.T.);
#1386=FACE_OUTER_BOUND('',#1916,.T.);
#1387=FACE_OUTER_BOUND('',#1917,.T.);
#1388=FACE_OUTER_BOUND('',#1918,.T.);
#1389=FACE_OUTER_BOUND('',#1919,.T.);
#1390=FACE_OUTER_BOUND('',#1920,.T.);
#1391=FACE_OUTER_BOUND('',#1921,.T.);
#1392=FACE_OUTER_BOUND('',#1922,.T.);
#1393=FACE_OUTER_BOUND('',#1923,.T.);
#1394=FACE_OUTER_BOUND('',#1924,.T.);
#1395=FACE_OUTER_BOUND('',#1925,.T.);
#1396=FACE_OUTER_BOUND('',#1926,.T.);
#1397=FACE_OUTER_BOUND('',#1927,.T.);
#1398=FACE_OUTER_BOUND('',#1928,.T.);
#1399=FACE_OUTER_BOUND('',#1929,.T.);
#1400=FACE_OUTER_BOUND('',#1930,.T.);
#1401=FACE_OUTER_BOUND('',#1931,.T.);
#1402=FACE_OUTER_BOUND('',#1932,.T.);
#1403=FACE_OUTER_BOUND('',#1933,.T.);
#1404=FACE_OUTER_BOUND('',#1934,.T.);
#1405=FACE_OUTER_BOUND('',#1935,.T.);
#1406=FACE_OUTER_BOUND('',#1936,.T.);
#1407=FACE_OUTER_BOUND('',#1937,.T.);
#1408=FACE_OUTER_BOUND('',#1938,.T.);
#1409=FACE_OUTER_BOUND('',#1939,.T.);
#1410=FACE_OUTER_BOUND('',#1940,.T.);
#1411=FACE_OUTER_BOUND('',#1941,.T.);
#1412=FACE_OUTER_BOUND('',#1942,.T.);
#1413=FACE_OUTER_BOUND('',#1943,.T.);
#1414=FACE_OUTER_BOUND('',#1944,.T.);
#1415=FACE_OUTER_BOUND('',#1945,.T.);
#1416=FACE_OUTER_BOUND('',#1947,.T.);
#1417=FACE_OUTER_BOUND('',#1948,.T.);
#1418=FACE_OUTER_BOUND('',#1949,.T.);
#1419=FACE_OUTER_BOUND('',#1950,.T.);
#1420=FACE_OUTER_BOUND('',#1951,.T.);
#1421=FACE_OUTER_BOUND('',#1952,.T.);
#1422=FACE_OUTER_BOUND('',#1953,.T.);
#1423=FACE_OUTER_BOUND('',#1954,.T.);
#1424=FACE_OUTER_BOUND('',#1955,.T.);
#1425=FACE_OUTER_BOUND('',#1956,.T.);
#1426=FACE_OUTER_BOUND('',#1957,.T.);
#1427=FACE_OUTER_BOUND('',#1959,.T.);
#1428=FACE_OUTER_BOUND('',#1960,.T.);
#1429=FACE_OUTER_BOUND('',#1961,.T.);
#1430=FACE_OUTER_BOUND('',#1962,.T.);
#1431=FACE_OUTER_BOUND('',#1963,.T.);
#1432=FACE_OUTER_BOUND('',#1964,.T.);
#1433=FACE_OUTER_BOUND('',#1965,.T.);
#1434=FACE_OUTER_BOUND('',#1967,.T.);
#1435=FACE_OUTER_BOUND('',#1968,.T.);
#1436=FACE_OUTER_BOUND('',#1969,.T.);
#1437=FACE_OUTER_BOUND('',#1970,.T.);
#1438=FACE_OUTER_BOUND('',#1971,.T.);
#1439=FACE_OUTER_BOUND('',#1973,.T.);
#1440=FACE_OUTER_BOUND('',#1975,.T.);
#1441=FACE_OUTER_BOUND('',#1976,.T.);
#1442=FACE_OUTER_BOUND('',#1977,.T.);
#1443=FACE_OUTER_BOUND('',#1978,.T.);
#1444=FACE_OUTER_BOUND('',#1979,.T.);
#1445=FACE_OUTER_BOUND('',#1980,.T.);
#1446=FACE_OUTER_BOUND('',#1981,.T.);
#1447=FACE_OUTER_BOUND('',#1982,.T.);
#1448=FACE_OUTER_BOUND('',#1983,.T.);
#1449=FACE_OUTER_BOUND('',#1984,.T.);
#1450=FACE_OUTER_BOUND('',#1986,.T.);
#1451=FACE_OUTER_BOUND('',#1988,.T.);
#1452=FACE_OUTER_BOUND('',#1989,.T.);
#1453=FACE_OUTER_BOUND('',#1990,.T.);
#1454=FACE_OUTER_BOUND('',#1991,.T.);
#1455=FACE_OUTER_BOUND('',#1992,.T.);
#1456=FACE_OUTER_BOUND('',#1993,.T.);
#1457=FACE_OUTER_BOUND('',#1994,.T.);
#1458=FACE_OUTER_BOUND('',#1995,.T.);
#1459=FACE_OUTER_BOUND('',#1996,.T.);
#1460=FACE_OUTER_BOUND('',#1997,.T.);
#1461=FACE_OUTER_BOUND('',#1998,.T.);
#1462=FACE_OUTER_BOUND('',#1999,.T.);
#1463=FACE_OUTER_BOUND('',#2001,.T.);
#1464=FACE_OUTER_BOUND('',#2002,.T.);
#1465=FACE_OUTER_BOUND('',#2003,.T.);
#1466=FACE_OUTER_BOUND('',#2004,.T.);
#1467=FACE_OUTER_BOUND('',#2005,.T.);
#1468=FACE_OUTER_BOUND('',#2006,.T.);
#1469=FACE_OUTER_BOUND('',#2007,.T.);
#1470=FACE_OUTER_BOUND('',#2008,.T.);
#1471=FACE_OUTER_BOUND('',#2010,.T.);
#1472=FACE_OUTER_BOUND('',#2011,.T.);
#1473=FACE_OUTER_BOUND('',#2012,.T.);
#1474=FACE_OUTER_BOUND('',#2013,.T.);
#1475=FACE_OUTER_BOUND('',#2014,.T.);
#1476=FACE_OUTER_BOUND('',#2015,.T.);
#1477=FACE_OUTER_BOUND('',#2016,.T.);
#1478=FACE_OUTER_BOUND('',#2017,.T.);
#1479=FACE_OUTER_BOUND('',#2018,.T.);
#1480=FACE_OUTER_BOUND('',#2019,.T.);
#1481=FACE_OUTER_BOUND('',#2020,.T.);
#1482=FACE_OUTER_BOUND('',#2021,.T.);
#1483=FACE_OUTER_BOUND('',#2023,.T.);
#1484=FACE_OUTER_BOUND('',#2024,.T.);
#1485=FACE_OUTER_BOUND('',#2025,.T.);
#1486=FACE_OUTER_BOUND('',#2026,.T.);
#1487=FACE_OUTER_BOUND('',#2027,.T.);
#1488=FACE_OUTER_BOUND('',#2028,.T.);
#1489=FACE_OUTER_BOUND('',#2029,.T.);
#1490=FACE_OUTER_BOUND('',#2030,.T.);
#1491=FACE_OUTER_BOUND('',#2032,.T.);
#1492=FACE_OUTER_BOUND('',#2033,.T.);
#1493=FACE_OUTER_BOUND('',#2034,.T.);
#1494=FACE_OUTER_BOUND('',#2035,.T.);
#1495=FACE_OUTER_BOUND('',#2036,.T.);
#1496=FACE_OUTER_BOUND('',#2037,.T.);
#1497=FACE_OUTER_BOUND('',#2038,.T.);
#1498=FACE_OUTER_BOUND('',#2039,.T.);
#1499=FACE_OUTER_BOUND('',#2040,.T.);
#1500=FACE_OUTER_BOUND('',#2041,.T.);
#1501=FACE_OUTER_BOUND('',#2042,.T.);
#1502=FACE_OUTER_BOUND('',#2043,.T.);
#1503=FACE_OUTER_BOUND('',#2045,.T.);
#1504=FACE_OUTER_BOUND('',#2046,.T.);
#1505=FACE_OUTER_BOUND('',#2047,.T.);
#1506=FACE_OUTER_BOUND('',#2048,.T.);
#1507=FACE_OUTER_BOUND('',#2049,.T.);
#1508=FACE_OUTER_BOUND('',#2050,.T.);
#1509=FACE_OUTER_BOUND('',#2051,.T.);
#1510=FACE_OUTER_BOUND('',#2052,.T.);
#1511=FACE_OUTER_BOUND('',#2054,.T.);
#1512=FACE_OUTER_BOUND('',#2055,.T.);
#1513=FACE_OUTER_BOUND('',#2056,.T.);
#1514=FACE_OUTER_BOUND('',#2057,.T.);
#1515=FACE_OUTER_BOUND('',#2058,.T.);
#1516=FACE_OUTER_BOUND('',#2059,.T.);
#1517=FACE_OUTER_BOUND('',#2060,.T.);
#1518=FACE_OUTER_BOUND('',#2061,.T.);
#1519=FACE_OUTER_BOUND('',#2062,.T.);
#1520=FACE_OUTER_BOUND('',#2063,.T.);
#1521=FACE_OUTER_BOUND('',#2064,.T.);
#1522=FACE_OUTER_BOUND('',#2065,.T.);
#1523=FACE_OUTER_BOUND('',#2067,.T.);
#1524=FACE_OUTER_BOUND('',#2068,.T.);
#1525=FACE_OUTER_BOUND('',#2069,.T.);
#1526=FACE_OUTER_BOUND('',#2070,.T.);
#1527=FACE_OUTER_BOUND('',#2071,.T.);
#1528=FACE_OUTER_BOUND('',#2072,.T.);
#1529=FACE_OUTER_BOUND('',#2073,.T.);
#1530=FACE_OUTER_BOUND('',#2074,.T.);
#1531=EDGE_LOOP('',(#5513,#5514,#5515,#5516));
#1532=EDGE_LOOP('',(#5517));
#1533=EDGE_LOOP('',(#5518,#5519,#5520,#5521));
#1534=EDGE_LOOP('',(#5522));
#1535=EDGE_LOOP('',(#5523,#5524,#5525,#5526));
#1536=EDGE_LOOP('',(#5527,#5528,#5529,#5530));
#1537=EDGE_LOOP('',(#5531,#5532,#5533,#5534));
#1538=EDGE_LOOP('',(#5535,#5536,#5537,#5538));
#1539=EDGE_LOOP('',(#5539,#5540,#5541,#5542));
#1540=EDGE_LOOP('',(#5543,#5544,#5545,#5546));
#1541=EDGE_LOOP('',(#5547,#5548,#5549,#5550));
#1542=EDGE_LOOP('',(#5551,#5552,#5553,#5554));
#1543=EDGE_LOOP('',(#5555,#5556,#5557,#5558));
#1544=EDGE_LOOP('',(#5559));
#1545=EDGE_LOOP('',(#5560));
#1546=EDGE_LOOP('',(#5561));
#1547=EDGE_LOOP('',(#5562));
#1548=EDGE_LOOP('',(#5563));
#1549=EDGE_LOOP('',(#5564));
#1550=EDGE_LOOP('',(#5565,#5566,#5567,#5568));
#1551=EDGE_LOOP('',(#5569));
#1552=EDGE_LOOP('',(#5570));
#1553=EDGE_LOOP('',(#5571));
#1554=EDGE_LOOP('',(#5572));
#1555=EDGE_LOOP('',(#5573,#5574,#5575,#5576));
#1556=EDGE_LOOP('',(#5577,#5578,#5579,#5580));
#1557=EDGE_LOOP('',(#5581,#5582,#5583,#5584));
#1558=EDGE_LOOP('',(#5585,#5586,#5587,#5588));
#1559=EDGE_LOOP('',(#5589,#5590,#5591,#5592));
#1560=EDGE_LOOP('',(#5593,#5594,#5595,#5596));
#1561=EDGE_LOOP('',(#5597,#5598,#5599,#5600));
#1562=EDGE_LOOP('',(#5601,#5602,#5603,#5604));
#1563=EDGE_LOOP('',(#5605,#5606,#5607,#5608));
#1564=EDGE_LOOP('',(#5609,#5610,#5611,#5612));
#1565=EDGE_LOOP('',(#5613,#5614,#5615,#5616));
#1566=EDGE_LOOP('',(#5617,#5618,#5619,#5620));
#1567=EDGE_LOOP('',(#5621,#5622,#5623,#5624));
#1568=EDGE_LOOP('',(#5625,#5626,#5627,#5628));
#1569=EDGE_LOOP('',(#5629,#5630,#5631,#5632));
#1570=EDGE_LOOP('',(#5633,#5634,#5635,#5636));
#1571=EDGE_LOOP('',(#5637,#5638,#5639,#5640));
#1572=EDGE_LOOP('',(#5641,#5642,#5643,#5644));
#1573=EDGE_LOOP('',(#5645,#5646,#5647,#5648));
#1574=EDGE_LOOP('',(#5649,#5650,#5651,#5652));
#1575=EDGE_LOOP('',(#5653,#5654,#5655,#5656));
#1576=EDGE_LOOP('',(#5657,#5658,#5659,#5660));
#1577=EDGE_LOOP('',(#5661,#5662,#5663,#5664));
#1578=EDGE_LOOP('',(#5665,#5666,#5667,#5668));
#1579=EDGE_LOOP('',(#5669,#5670,#5671,#5672));
#1580=EDGE_LOOP('',(#5673,#5674,#5675,#5676));
#1581=EDGE_LOOP('',(#5677,#5678,#5679,#5680));
#1582=EDGE_LOOP('',(#5681,#5682,#5683,#5684));
#1583=EDGE_LOOP('',(#5685,#5686,#5687,#5688));
#1584=EDGE_LOOP('',(#5689,#5690,#5691,#5692));
#1585=EDGE_LOOP('',(#5693,#5694,#5695,#5696));
#1586=EDGE_LOOP('',(#5697,#5698,#5699,#5700));
#1587=EDGE_LOOP('',(#5701,#5702,#5703,#5704));
#1588=EDGE_LOOP('',(#5705,#5706,#5707,#5708));
#1589=EDGE_LOOP('',(#5709,#5710,#5711,#5712));
#1590=EDGE_LOOP('',(#5713,#5714,#5715,#5716));
#1591=EDGE_LOOP('',(#5717,#5718,#5719,#5720));
#1592=EDGE_LOOP('',(#5721,#5722,#5723,#5724));
#1593=EDGE_LOOP('',(#5725,#5726,#5727,#5728));
#1594=EDGE_LOOP('',(#5729,#5730,#5731,#5732));
#1595=EDGE_LOOP('',(#5733,#5734,#5735,#5736));
#1596=EDGE_LOOP('',(#5737,#5738,#5739,#5740));
#1597=EDGE_LOOP('',(#5741,#5742,#5743,#5744));
#1598=EDGE_LOOP('',(#5745,#5746,#5747,#5748));
#1599=EDGE_LOOP('',(#5749,#5750,#5751,#5752));
#1600=EDGE_LOOP('',(#5753,#5754,#5755,#5756));
#1601=EDGE_LOOP('',(#5757,#5758,#5759,#5760));
#1602=EDGE_LOOP('',(#5761,#5762,#5763,#5764));
#1603=EDGE_LOOP('',(#5765,#5766,#5767,#5768));
#1604=EDGE_LOOP('',(#5769,#5770,#5771,#5772));
#1605=EDGE_LOOP('',(#5773,#5774,#5775,#5776));
#1606=EDGE_LOOP('',(#5777,#5778,#5779,#5780));
#1607=EDGE_LOOP('',(#5781,#5782,#5783,#5784));
#1608=EDGE_LOOP('',(#5785,#5786,#5787,#5788));
#1609=EDGE_LOOP('',(#5789,#5790,#5791,#5792));
#1610=EDGE_LOOP('',(#5793,#5794,#5795,#5796));
#1611=EDGE_LOOP('',(#5797,#5798,#5799,#5800));
#1612=EDGE_LOOP('',(#5801,#5802,#5803,#5804));
#1613=EDGE_LOOP('',(#5805,#5806,#5807,#5808));
#1614=EDGE_LOOP('',(#5809,#5810,#5811,#5812));
#1615=EDGE_LOOP('',(#5813,#5814,#5815,#5816));
#1616=EDGE_LOOP('',(#5817,#5818,#5819,#5820));
#1617=EDGE_LOOP('',(#5821,#5822,#5823,#5824));
#1618=EDGE_LOOP('',(#5825,#5826,#5827,#5828));
#1619=EDGE_LOOP('',(#5829,#5830,#5831,#5832));
#1620=EDGE_LOOP('',(#5833,#5834,#5835,#5836));
#1621=EDGE_LOOP('',(#5837,#5838,#5839,#5840));
#1622=EDGE_LOOP('',(#5841,#5842,#5843,#5844));
#1623=EDGE_LOOP('',(#5845,#5846,#5847,#5848));
#1624=EDGE_LOOP('',(#5849,#5850,#5851,#5852));
#1625=EDGE_LOOP('',(#5853,#5854,#5855,#5856));
#1626=EDGE_LOOP('',(#5857,#5858,#5859,#5860));
#1627=EDGE_LOOP('',(#5861,#5862,#5863,#5864));
#1628=EDGE_LOOP('',(#5865,#5866,#5867,#5868));
#1629=EDGE_LOOP('',(#5869,#5870,#5871,#5872));
#1630=EDGE_LOOP('',(#5873,#5874,#5875,#5876));
#1631=EDGE_LOOP('',(#5877,#5878,#5879,#5880));
#1632=EDGE_LOOP('',(#5881,#5882,#5883,#5884));
#1633=EDGE_LOOP('',(#5885,#5886,#5887,#5888));
#1634=EDGE_LOOP('',(#5889,#5890,#5891,#5892));
#1635=EDGE_LOOP('',(#5893,#5894,#5895,#5896));
#1636=EDGE_LOOP('',(#5897,#5898,#5899,#5900));
#1637=EDGE_LOOP('',(#5901,#5902,#5903,#5904));
#1638=EDGE_LOOP('',(#5905,#5906,#5907,#5908));
#1639=EDGE_LOOP('',(#5909,#5910,#5911,#5912));
#1640=EDGE_LOOP('',(#5913,#5914,#5915,#5916));
#1641=EDGE_LOOP('',(#5917,#5918,#5919,#5920));
#1642=EDGE_LOOP('',(#5921,#5922,#5923,#5924));
#1643=EDGE_LOOP('',(#5925,#5926,#5927,#5928));
#1644=EDGE_LOOP('',(#5929,#5930,#5931,#5932));
#1645=EDGE_LOOP('',(#5933,#5934,#5935,#5936));
#1646=EDGE_LOOP('',(#5937,#5938,#5939,#5940));
#1647=EDGE_LOOP('',(#5941,#5942,#5943,#5944));
#1648=EDGE_LOOP('',(#5945,#5946,#5947,#5948));
#1649=EDGE_LOOP('',(#5949,#5950,#5951,#5952));
#1650=EDGE_LOOP('',(#5953,#5954,#5955,#5956));
#1651=EDGE_LOOP('',(#5957,#5958,#5959,#5960));
#1652=EDGE_LOOP('',(#5961,#5962,#5963,#5964));
#1653=EDGE_LOOP('',(#5965,#5966,#5967,#5968));
#1654=EDGE_LOOP('',(#5969,#5970,#5971,#5972));
#1655=EDGE_LOOP('',(#5973,#5974,#5975,#5976));
#1656=EDGE_LOOP('',(#5977,#5978,#5979,#5980));
#1657=EDGE_LOOP('',(#5981,#5982,#5983,#5984));
#1658=EDGE_LOOP('',(#5985,#5986,#5987,#5988));
#1659=EDGE_LOOP('',(#5989,#5990,#5991,#5992));
#1660=EDGE_LOOP('',(#5993,#5994,#5995,#5996));
#1661=EDGE_LOOP('',(#5997,#5998,#5999,#6000));
#1662=EDGE_LOOP('',(#6001,#6002,#6003,#6004));
#1663=EDGE_LOOP('',(#6005,#6006,#6007,#6008));
#1664=EDGE_LOOP('',(#6009,#6010,#6011,#6012));
#1665=EDGE_LOOP('',(#6013,#6014,#6015,#6016));
#1666=EDGE_LOOP('',(#6017,#6018,#6019,#6020));
#1667=EDGE_LOOP('',(#6021,#6022,#6023,#6024));
#1668=EDGE_LOOP('',(#6025,#6026,#6027,#6028));
#1669=EDGE_LOOP('',(#6029,#6030,#6031,#6032));
#1670=EDGE_LOOP('',(#6033,#6034,#6035,#6036));
#1671=EDGE_LOOP('',(#6037,#6038,#6039,#6040));
#1672=EDGE_LOOP('',(#6041,#6042,#6043,#6044));
#1673=EDGE_LOOP('',(#6045,#6046,#6047,#6048));
#1674=EDGE_LOOP('',(#6049,#6050,#6051,#6052));
#1675=EDGE_LOOP('',(#6053,#6054,#6055,#6056));
#1676=EDGE_LOOP('',(#6057,#6058,#6059,#6060));
#1677=EDGE_LOOP('',(#6061,#6062,#6063,#6064));
#1678=EDGE_LOOP('',(#6065,#6066,#6067,#6068));
#1679=EDGE_LOOP('',(#6069,#6070,#6071,#6072));
#1680=EDGE_LOOP('',(#6073,#6074,#6075,#6076));
#1681=EDGE_LOOP('',(#6077,#6078,#6079,#6080));
#1682=EDGE_LOOP('',(#6081,#6082,#6083,#6084));
#1683=EDGE_LOOP('',(#6085,#6086,#6087,#6088));
#1684=EDGE_LOOP('',(#6089,#6090,#6091,#6092));
#1685=EDGE_LOOP('',(#6093,#6094,#6095,#6096));
#1686=EDGE_LOOP('',(#6097,#6098,#6099,#6100));
#1687=EDGE_LOOP('',(#6101,#6102,#6103,#6104));
#1688=EDGE_LOOP('',(#6105,#6106,#6107,#6108));
#1689=EDGE_LOOP('',(#6109,#6110,#6111,#6112));
#1690=EDGE_LOOP('',(#6113,#6114,#6115,#6116));
#1691=EDGE_LOOP('',(#6117,#6118,#6119,#6120));
#1692=EDGE_LOOP('',(#6121,#6122,#6123,#6124));
#1693=EDGE_LOOP('',(#6125,#6126,#6127,#6128));
#1694=EDGE_LOOP('',(#6129,#6130,#6131,#6132));
#1695=EDGE_LOOP('',(#6133,#6134,#6135,#6136));
#1696=EDGE_LOOP('',(#6137,#6138,#6139,#6140));
#1697=EDGE_LOOP('',(#6141,#6142,#6143,#6144));
#1698=EDGE_LOOP('',(#6145,#6146,#6147,#6148));
#1699=EDGE_LOOP('',(#6149,#6150,#6151,#6152));
#1700=EDGE_LOOP('',(#6153,#6154,#6155,#6156));
#1701=EDGE_LOOP('',(#6157,#6158,#6159,#6160));
#1702=EDGE_LOOP('',(#6161,#6162,#6163,#6164));
#1703=EDGE_LOOP('',(#6165,#6166,#6167,#6168));
#1704=EDGE_LOOP('',(#6169,#6170,#6171,#6172));
#1705=EDGE_LOOP('',(#6173,#6174,#6175,#6176));
#1706=EDGE_LOOP('',(#6177,#6178,#6179,#6180));
#1707=EDGE_LOOP('',(#6181,#6182,#6183,#6184));
#1708=EDGE_LOOP('',(#6185,#6186,#6187,#6188));
#1709=EDGE_LOOP('',(#6189,#6190,#6191,#6192));
#1710=EDGE_LOOP('',(#6193,#6194,#6195,#6196));
#1711=EDGE_LOOP('',(#6197,#6198,#6199,#6200));
#1712=EDGE_LOOP('',(#6201,#6202,#6203,#6204));
#1713=EDGE_LOOP('',(#6205,#6206,#6207,#6208));
#1714=EDGE_LOOP('',(#6209,#6210,#6211,#6212));
#1715=EDGE_LOOP('',(#6213,#6214,#6215,#6216));
#1716=EDGE_LOOP('',(#6217,#6218,#6219,#6220));
#1717=EDGE_LOOP('',(#6221,#6222,#6223,#6224));
#1718=EDGE_LOOP('',(#6225,#6226,#6227,#6228));
#1719=EDGE_LOOP('',(#6229,#6230,#6231,#6232));
#1720=EDGE_LOOP('',(#6233,#6234,#6235,#6236));
#1721=EDGE_LOOP('',(#6237,#6238,#6239,#6240));
#1722=EDGE_LOOP('',(#6241,#6242,#6243,#6244));
#1723=EDGE_LOOP('',(#6245,#6246,#6247,#6248));
#1724=EDGE_LOOP('',(#6249,#6250,#6251,#6252));
#1725=EDGE_LOOP('',(#6253,#6254,#6255,#6256));
#1726=EDGE_LOOP('',(#6257,#6258,#6259,#6260));
#1727=EDGE_LOOP('',(#6261,#6262,#6263,#6264));
#1728=EDGE_LOOP('',(#6265,#6266,#6267,#6268));
#1729=EDGE_LOOP('',(#6269,#6270,#6271,#6272));
#1730=EDGE_LOOP('',(#6273,#6274,#6275,#6276));
#1731=EDGE_LOOP('',(#6277,#6278,#6279,#6280));
#1732=EDGE_LOOP('',(#6281,#6282,#6283,#6284));
#1733=EDGE_LOOP('',(#6285,#6286,#6287,#6288));
#1734=EDGE_LOOP('',(#6289,#6290,#6291,#6292));
#1735=EDGE_LOOP('',(#6293,#6294,#6295,#6296));
#1736=EDGE_LOOP('',(#6297,#6298,#6299,#6300));
#1737=EDGE_LOOP('',(#6301,#6302,#6303,#6304));
#1738=EDGE_LOOP('',(#6305,#6306,#6307,#6308));
#1739=EDGE_LOOP('',(#6309,#6310,#6311,#6312));
#1740=EDGE_LOOP('',(#6313,#6314,#6315,#6316));
#1741=EDGE_LOOP('',(#6317,#6318,#6319,#6320));
#1742=EDGE_LOOP('',(#6321,#6322,#6323,#6324));
#1743=EDGE_LOOP('',(#6325,#6326,#6327,#6328));
#1744=EDGE_LOOP('',(#6329,#6330,#6331,#6332));
#1745=EDGE_LOOP('',(#6333,#6334,#6335,#6336));
#1746=EDGE_LOOP('',(#6337,#6338,#6339,#6340));
#1747=EDGE_LOOP('',(#6341,#6342,#6343,#6344));
#1748=EDGE_LOOP('',(#6345,#6346,#6347,#6348));
#1749=EDGE_LOOP('',(#6349));
#1750=EDGE_LOOP('',(#6350));
#1751=EDGE_LOOP('',(#6351));
#1752=EDGE_LOOP('',(#6352,#6353,#6354,#6355));
#1753=EDGE_LOOP('',(#6356));
#1754=EDGE_LOOP('',(#6357));
#1755=EDGE_LOOP('',(#6358));
#1756=EDGE_LOOP('',(#6359));
#1757=EDGE_LOOP('',(#6360,#6361,#6362,#6363));
#1758=EDGE_LOOP('',(#6364));
#1759=EDGE_LOOP('',(#6365));
#1760=EDGE_LOOP('',(#6366));
#1761=EDGE_LOOP('',(#6367));
#1762=EDGE_LOOP('',(#6368));
#1763=EDGE_LOOP('',(#6369));
#1764=EDGE_LOOP('',(#6370));
#1765=EDGE_LOOP('',(#6371,#6372,#6373,#6374,#6375,#6376,#6377,#6378,#6379,
#6380,#6381,#6382,#6383,#6384,#6385,#6386,#6387,#6388,#6389,#6390,#6391,
#6392,#6393,#6394,#6395,#6396,#6397,#6398,#6399,#6400,#6401,#6402,#6403,
#6404,#6405,#6406,#6407,#6408,#6409,#6410,#6411,#6412,#6413,#6414,#6415,
#6416,#6417,#6418,#6419,#6420,#6421,#6422,#6423,#6424,#6425,#6426,#6427,
#6428,#6429,#6430,#6431,#6432,#6433,#6434,#6435,#6436,#6437,#6438,#6439,
#6440,#6441,#6442,#6443,#6444,#6445,#6446,#6447,#6448,#6449,#6450,#6451,
#6452,#6453,#6454,#6455,#6456,#6457,#6458,#6459,#6460,#6461,#6462,#6463,
#6464,#6465,#6466,#6467,#6468,#6469,#6470,#6471,#6472,#6473,#6474,#6475,
#6476,#6477,#6478,#6479,#6480,#6481,#6482,#6483,#6484,#6485,#6486,#6487,
#6488,#6489,#6490,#6491,#6492,#6493,#6494,#6495,#6496,#6497,#6498,#6499,
#6500,#6501,#6502,#6503,#6504,#6505,#6506,#6507,#6508,#6509,#6510,#6511,
#6512,#6513,#6514,#6515,#6516,#6517,#6518,#6519,#6520,#6521,#6522,#6523,
#6524,#6525,#6526,#6527,#6528,#6529,#6530,#6531,#6532,#6533,#6534,#6535,
#6536,#6537,#6538,#6539,#6540,#6541,#6542,#6543,#6544,#6545,#6546,#6547,
#6548,#6549,#6550,#6551,#6552,#6553,#6554,#6555,#6556,#6557,#6558,#6559,
#6560,#6561,#6562));
#1766=EDGE_LOOP('',(#6563,#6564,#6565,#6566));
#1767=EDGE_LOOP('',(#6567,#6568,#6569,#6570,#6571,#6572,#6573,#6574,#6575,
#6576,#6577,#6578,#6579,#6580,#6581,#6582,#6583,#6584,#6585,#6586,#6587,
#6588,#6589,#6590,#6591,#6592,#6593,#6594,#6595,#6596,#6597,#6598,#6599,
#6600,#6601,#6602,#6603,#6604,#6605,#6606,#6607,#6608,#6609,#6610,#6611,
#6612,#6613,#6614,#6615,#6616,#6617,#6618,#6619,#6620,#6621,#6622,#6623,
#6624,#6625,#6626,#6627,#6628,#6629,#6630,#6631,#6632,#6633,#6634,#6635,
#6636,#6637,#6638,#6639,#6640,#6641,#6642,#6643,#6644,#6645,#6646,#6647,
#6648,#6649,#6650,#6651,#6652,#6653,#6654,#6655,#6656,#6657,#6658,#6659,
#6660,#6661,#6662,#6663,#6664,#6665,#6666,#6667,#6668,#6669,#6670,#6671,
#6672,#6673,#6674,#6675,#6676,#6677,#6678,#6679,#6680,#6681,#6682,#6683,
#6684,#6685,#6686,#6687,#6688,#6689,#6690,#6691,#6692,#6693,#6694,#6695,
#6696,#6697,#6698,#6699,#6700,#6701,#6702,#6703,#6704,#6705,#6706,#6707,
#6708,#6709,#6710,#6711,#6712,#6713,#6714,#6715,#6716,#6717,#6718,#6719,
#6720,#6721,#6722,#6723,#6724,#6725,#6726,#6727,#6728,#6729,#6730,#6731,
#6732,#6733,#6734,#6735,#6736,#6737,#6738,#6739,#6740,#6741,#6742,#6743,
#6744,#6745,#6746,#6747,#6748,#6749,#6750,#6751,#6752,#6753,#6754,#6755,
#6756,#6757,#6758));
#1768=EDGE_LOOP('',(#6759,#6760,#6761,#6762));
#1769=EDGE_LOOP('',(#6763,#6764,#6765,#6766));
#1770=EDGE_LOOP('',(#6767,#6768,#6769,#6770));
#1771=EDGE_LOOP('',(#6771));
#1772=EDGE_LOOP('',(#6772));
#1773=EDGE_LOOP('',(#6773,#6774,#6775,#6776));
#1774=EDGE_LOOP('',(#6777));
#1775=EDGE_LOOP('',(#6778));
#1776=EDGE_LOOP('',(#6779,#6780,#6781,#6782));
#1777=EDGE_LOOP('',(#6783,#6784,#6785,#6786,#6787,#6788,#6789,#6790));
#1778=EDGE_LOOP('',(#6791,#6792,#6793,#6794));
#1779=EDGE_LOOP('',(#6795,#6796,#6797,#6798));
#1780=EDGE_LOOP('',(#6799,#6800,#6801,#6802));
#1781=EDGE_LOOP('',(#6803,#6804,#6805,#6806));
#1782=EDGE_LOOP('',(#6807,#6808,#6809,#6810,#6811,#6812,#6813));
#1783=EDGE_LOOP('',(#6814));
#1784=EDGE_LOOP('',(#6815,#6816,#6817,#6818));
#1785=EDGE_LOOP('',(#6819,#6820,#6821,#6822));
#1786=EDGE_LOOP('',(#6823,#6824,#6825,#6826,#6827,#6828,#6829));
#1787=EDGE_LOOP('',(#6830));
#1788=EDGE_LOOP('',(#6831,#6832,#6833,#6834,#6835,#6836));
#1789=EDGE_LOOP('',(#6837,#6838,#6839,#6840,#6841,#6842));
#1790=EDGE_LOOP('',(#6843,#6844,#6845,#6846,#6847,#6848,#6849,#6850));
#1791=EDGE_LOOP('',(#6851,#6852,#6853,#6854));
#1792=EDGE_LOOP('',(#6855,#6856,#6857,#6858));
#1793=EDGE_LOOP('',(#6859,#6860,#6861,#6862));
#1794=EDGE_LOOP('',(#6863,#6864,#6865,#6866));
#1795=EDGE_LOOP('',(#6867,#6868,#6869,#6870));
#1796=EDGE_LOOP('',(#6871,#6872,#6873,#6874));
#1797=EDGE_LOOP('',(#6875));
#1798=EDGE_LOOP('',(#6876,#6877,#6878,#6879));
#1799=EDGE_LOOP('',(#6880,#6881,#6882,#6883));
#1800=EDGE_LOOP('',(#6884));
#1801=EDGE_LOOP('',(#6885,#6886,#6887,#6888));
#1802=EDGE_LOOP('',(#6889,#6890,#6891,#6892));
#1803=EDGE_LOOP('',(#6893,#6894,#6895,#6896));
#1804=EDGE_LOOP('',(#6897,#6898,#6899,#6900));
#1805=EDGE_LOOP('',(#6901,#6902,#6903,#6904));
#1806=EDGE_LOOP('',(#6905));
#1807=EDGE_LOOP('',(#6906,#6907,#6908,#6909));
#1808=EDGE_LOOP('',(#6910,#6911,#6912,#6913));
#1809=EDGE_LOOP('',(#6914));
#1810=EDGE_LOOP('',(#6915,#6916,#6917,#6918));
#1811=EDGE_LOOP('',(#6919,#6920,#6921,#6922));
#1812=EDGE_LOOP('',(#6923,#6924,#6925,#6926));
#1813=EDGE_LOOP('',(#6927,#6928,#6929,#6930));
#1814=EDGE_LOOP('',(#6931,#6932,#6933,#6934));
#1815=EDGE_LOOP('',(#6935,#6936,#6937,#6938));
#1816=EDGE_LOOP('',(#6939,#6940,#6941,#6942));
#1817=EDGE_LOOP('',(#6943,#6944,#6945,#6946));
#1818=EDGE_LOOP('',(#6947,#6948,#6949,#6950));
#1819=EDGE_LOOP('',(#6951,#6952,#6953,#6954));
#1820=EDGE_LOOP('',(#6955,#6956,#6957,#6958));
#1821=EDGE_LOOP('',(#6959));
#1822=EDGE_LOOP('',(#6960,#6961,#6962,#6963));
#1823=EDGE_LOOP('',(#6964,#6965,#6966,#6967));
#1824=EDGE_LOOP('',(#6968));
#1825=EDGE_LOOP('',(#6969,#6970,#6971,#6972));
#1826=EDGE_LOOP('',(#6973,#6974,#6975,#6976));
#1827=EDGE_LOOP('',(#6977,#6978,#6979,#6980));
#1828=EDGE_LOOP('',(#6981,#6982,#6983,#6984));
#1829=EDGE_LOOP('',(#6985,#6986,#6987,#6988));
#1830=EDGE_LOOP('',(#6989));
#1831=EDGE_LOOP('',(#6990,#6991,#6992,#6993));
#1832=EDGE_LOOP('',(#6994,#6995,#6996,#6997));
#1833=EDGE_LOOP('',(#6998));
#1834=EDGE_LOOP('',(#6999,#7000,#7001,#7002));
#1835=EDGE_LOOP('',(#7003,#7004,#7005,#7006));
#1836=EDGE_LOOP('',(#7007,#7008,#7009,#7010));
#1837=EDGE_LOOP('',(#7011,#7012,#7013,#7014));
#1838=EDGE_LOOP('',(#7015,#7016,#7017,#7018));
#1839=EDGE_LOOP('',(#7019,#7020,#7021,#7022));
#1840=EDGE_LOOP('',(#7023,#7024,#7025,#7026));
#1841=EDGE_LOOP('',(#7027,#7028,#7029,#7030));
#1842=EDGE_LOOP('',(#7031,#7032,#7033,#7034));
#1843=EDGE_LOOP('',(#7035,#7036,#7037,#7038));
#1844=EDGE_LOOP('',(#7039,#7040,#7041,#7042));
#1845=EDGE_LOOP('',(#7043,#7044,#7045,#7046));
#1846=EDGE_LOOP('',(#7047,#7048,#7049,#7050));
#1847=EDGE_LOOP('',(#7051,#7052,#7053,#7054));
#1848=EDGE_LOOP('',(#7055,#7056,#7057,#7058,#7059,#7060,#7061,#7062));
#1849=EDGE_LOOP('',(#7063,#7064,#7065,#7066));
#1850=EDGE_LOOP('',(#7067,#7068,#7069,#7070));
#1851=EDGE_LOOP('',(#7071,#7072,#7073,#7074));
#1852=EDGE_LOOP('',(#7075,#7076,#7077,#7078,#7079,#7080));
#1853=EDGE_LOOP('',(#7081,#7082,#7083,#7084));
#1854=EDGE_LOOP('',(#7085,#7086,#7087,#7088));
#1855=EDGE_LOOP('',(#7089,#7090,#7091,#7092));
#1856=EDGE_LOOP('',(#7093,#7094,#7095,#7096,#7097,#7098,#7099));
#1857=EDGE_LOOP('',(#7100));
#1858=EDGE_LOOP('',(#7101,#7102,#7103,#7104));
#1859=EDGE_LOOP('',(#7105,#7106,#7107,#7108));
#1860=EDGE_LOOP('',(#7109,#7110,#7111,#7112,#7113,#7114,#7115));
#1861=EDGE_LOOP('',(#7116));
#1862=EDGE_LOOP('',(#7117,#7118,#7119,#7120,#7121,#7122));
#1863=EDGE_LOOP('',(#7123,#7124,#7125,#7126));
#1864=EDGE_LOOP('',(#7127,#7128,#7129,#7130,#7131,#7132,#7133,#7134));
#1865=EDGE_LOOP('',(#7135,#7136,#7137,#7138));
#1866=EDGE_LOOP('',(#7139,#7140,#7141,#7142));
#1867=EDGE_LOOP('',(#7143,#7144,#7145,#7146));
#1868=EDGE_LOOP('',(#7147,#7148,#7149,#7150));
#1869=EDGE_LOOP('',(#7151));
#1870=EDGE_LOOP('',(#7152,#7153,#7154,#7155));
#1871=EDGE_LOOP('',(#7156,#7157,#7158,#7159));
#1872=EDGE_LOOP('',(#7160));
#1873=EDGE_LOOP('',(#7161,#7162,#7163,#7164));
#1874=EDGE_LOOP('',(#7165,#7166,#7167,#7168));
#1875=EDGE_LOOP('',(#7169,#7170,#7171,#7172));
#1876=EDGE_LOOP('',(#7173,#7174,#7175,#7176));
#1877=EDGE_LOOP('',(#7177,#7178,#7179,#7180));
#1878=EDGE_LOOP('',(#7181));
#1879=EDGE_LOOP('',(#7182,#7183,#7184,#7185));
#1880=EDGE_LOOP('',(#7186,#7187,#7188,#7189));
#1881=EDGE_LOOP('',(#7190));
#1882=EDGE_LOOP('',(#7191,#7192,#7193,#7194));
#1883=EDGE_LOOP('',(#7195,#7196,#7197,#7198));
#1884=EDGE_LOOP('',(#7199,#7200,#7201,#7202));
#1885=EDGE_LOOP('',(#7203,#7204,#7205,#7206));
#1886=EDGE_LOOP('',(#7207,#7208,#7209,#7210));
#1887=EDGE_LOOP('',(#7211,#7212,#7213,#7214));
#1888=EDGE_LOOP('',(#7215,#7216,#7217,#7218));
#1889=EDGE_LOOP('',(#7219,#7220,#7221,#7222));
#1890=EDGE_LOOP('',(#7223,#7224,#7225,#7226));
#1891=EDGE_LOOP('',(#7227,#7228,#7229,#7230));
#1892=EDGE_LOOP('',(#7231,#7232,#7233,#7234));
#1893=EDGE_LOOP('',(#7235));
#1894=EDGE_LOOP('',(#7236,#7237,#7238,#7239));
#1895=EDGE_LOOP('',(#7240,#7241,#7242,#7243));
#1896=EDGE_LOOP('',(#7244));
#1897=EDGE_LOOP('',(#7245,#7246,#7247,#7248));
#1898=EDGE_LOOP('',(#7249,#7250,#7251,#7252));
#1899=EDGE_LOOP('',(#7253,#7254,#7255,#7256));
#1900=EDGE_LOOP('',(#7257,#7258,#7259,#7260));
#1901=EDGE_LOOP('',(#7261,#7262,#7263,#7264));
#1902=EDGE_LOOP('',(#7265));
#1903=EDGE_LOOP('',(#7266,#7267,#7268,#7269));
#1904=EDGE_LOOP('',(#7270,#7271,#7272,#7273));
#1905=EDGE_LOOP('',(#7274));
#1906=EDGE_LOOP('',(#7275,#7276,#7277,#7278));
#1907=EDGE_LOOP('',(#7279,#7280,#7281,#7282));
#1908=EDGE_LOOP('',(#7283,#7284,#7285,#7286));
#1909=EDGE_LOOP('',(#7287,#7288,#7289,#7290));
#1910=EDGE_LOOP('',(#7291,#7292,#7293,#7294));
#1911=EDGE_LOOP('',(#7295,#7296,#7297,#7298));
#1912=EDGE_LOOP('',(#7299,#7300,#7301,#7302));
#1913=EDGE_LOOP('',(#7303,#7304,#7305,#7306));
#1914=EDGE_LOOP('',(#7307,#7308,#7309,#7310));
#1915=EDGE_LOOP('',(#7311,#7312,#7313,#7314));
#1916=EDGE_LOOP('',(#7315,#7316,#7317,#7318));
#1917=EDGE_LOOP('',(#7319,#7320,#7321,#7322));
#1918=EDGE_LOOP('',(#7323,#7324,#7325,#7326));
#1919=EDGE_LOOP('',(#7327,#7328,#7329,#7330));
#1920=EDGE_LOOP('',(#7331,#7332,#7333,#7334));
#1921=EDGE_LOOP('',(#7335,#7336,#7337,#7338));
#1922=EDGE_LOOP('',(#7339,#7340,#7341,#7342));
#1923=EDGE_LOOP('',(#7343,#7344,#7345,#7346));
#1924=EDGE_LOOP('',(#7347,#7348,#7349,#7350));
#1925=EDGE_LOOP('',(#7351,#7352,#7353,#7354));
#1926=EDGE_LOOP('',(#7355,#7356,#7357,#7358));
#1927=EDGE_LOOP('',(#7359,#7360,#7361,#7362));
#1928=EDGE_LOOP('',(#7363,#7364,#7365,#7366));
#1929=EDGE_LOOP('',(#7367,#7368,#7369,#7370));
#1930=EDGE_LOOP('',(#7371,#7372,#7373,#7374));
#1931=EDGE_LOOP('',(#7375,#7376,#7377,#7378));
#1932=EDGE_LOOP('',(#7379,#7380,#7381,#7382));
#1933=EDGE_LOOP('',(#7383,#7384,#7385,#7386));
#1934=EDGE_LOOP('',(#7387,#7388,#7389,#7390));
#1935=EDGE_LOOP('',(#7391,#7392,#7393,#7394));
#1936=EDGE_LOOP('',(#7395,#7396,#7397,#7398));
#1937=EDGE_LOOP('',(#7399,#7400,#7401,#7402));
#1938=EDGE_LOOP('',(#7403,#7404,#7405,#7406,#7407,#7408));
#1939=EDGE_LOOP('',(#7409,#7410,#7411,#7412,#7413,#7414));
#1940=EDGE_LOOP('',(#7415));
#1941=EDGE_LOOP('',(#7416));
#1942=EDGE_LOOP('',(#7417,#7418,#7419,#7420));
#1943=EDGE_LOOP('',(#7421,#7422,#7423,#7424));
#1944=EDGE_LOOP('',(#7425,#7426,#7427,#7428));
#1945=EDGE_LOOP('',(#7429));
#1946=EDGE_LOOP('',(#7430));
#1947=EDGE_LOOP('',(#7431,#7432,#7433,#7434));
#1948=EDGE_LOOP('',(#7435,#7436,#7437,#7438));
#1949=EDGE_LOOP('',(#7439,#7440,#7441,#7442));
#1950=EDGE_LOOP('',(#7443,#7444,#7445,#7446));
#1951=EDGE_LOOP('',(#7447,#7448,#7449,#7450));
#1952=EDGE_LOOP('',(#7451,#7452,#7453,#7454));
#1953=EDGE_LOOP('',(#7455,#7456,#7457,#7458));
#1954=EDGE_LOOP('',(#7459,#7460,#7461,#7462));
#1955=EDGE_LOOP('',(#7463,#7464,#7465,#7466,#7467,#7468));
#1956=EDGE_LOOP('',(#7469,#7470,#7471,#7472,#7473,#7474));
#1957=EDGE_LOOP('',(#7475));
#1958=EDGE_LOOP('',(#7476));
#1959=EDGE_LOOP('',(#7477,#7478,#7479,#7480));
#1960=EDGE_LOOP('',(#7481));
#1961=EDGE_LOOP('',(#7482));
#1962=EDGE_LOOP('',(#7483,#7484,#7485,#7486));
#1963=EDGE_LOOP('',(#7487,#7488,#7489,#7490));
#1964=EDGE_LOOP('',(#7491,#7492,#7493,#7494));
#1965=EDGE_LOOP('',(#7495));
#1966=EDGE_LOOP('',(#7496));
#1967=EDGE_LOOP('',(#7497,#7498,#7499,#7500));
#1968=EDGE_LOOP('',(#7501,#7502,#7503,#7504));
#1969=EDGE_LOOP('',(#7505,#7506,#7507,#7508));
#1970=EDGE_LOOP('',(#7509,#7510,#7511,#7512));
#1971=EDGE_LOOP('',(#7513));
#1972=EDGE_LOOP('',(#7514));
#1973=EDGE_LOOP('',(#7515));
#1974=EDGE_LOOP('',(#7516));
#1975=EDGE_LOOP('',(#7517,#7518,#7519,#7520,#7521,#7522,#7523,#7524,#7525));
#1976=EDGE_LOOP('',(#7526,#7527,#7528,#7529,#7530,#7531,#7532,#7533,#7534));
#1977=EDGE_LOOP('',(#7535,#7536,#7537,#7538));
#1978=EDGE_LOOP('',(#7539,#7540,#7541,#7542));
#1979=EDGE_LOOP('',(#7543,#7544,#7545,#7546));
#1980=EDGE_LOOP('',(#7547,#7548,#7549,#7550));
#1981=EDGE_LOOP('',(#7551,#7552,#7553,#7554));
#1982=EDGE_LOOP('',(#7555,#7556,#7557,#7558));
#1983=EDGE_LOOP('',(#7559,#7560,#7561,#7562));
#1984=EDGE_LOOP('',(#7563));
#1985=EDGE_LOOP('',(#7564));
#1986=EDGE_LOOP('',(#7565));
#1987=EDGE_LOOP('',(#7566));
#1988=EDGE_LOOP('',(#7567,#7568,#7569,#7570));
#1989=EDGE_LOOP('',(#7571,#7572,#7573,#7574));
#1990=EDGE_LOOP('',(#7575,#7576,#7577,#7578));
#1991=EDGE_LOOP('',(#7579,#7580,#7581,#7582));
#1992=EDGE_LOOP('',(#7583,#7584,#7585,#7586));
#1993=EDGE_LOOP('',(#7587,#7588,#7589,#7590));
#1994=EDGE_LOOP('',(#7591,#7592,#7593,#7594));
#1995=EDGE_LOOP('',(#7595,#7596,#7597,#7598));
#1996=EDGE_LOOP('',(#7599,#7600,#7601,#7602));
#1997=EDGE_LOOP('',(#7603,#7604,#7605,#7606,#7607,#7608,#7609,#7610,#7611,
#7612,#7613,#7614));
#1998=EDGE_LOOP('',(#7615,#7616,#7617,#7618,#7619,#7620,#7621,#7622,#7623,
#7624,#7625,#7626));
#1999=EDGE_LOOP('',(#7627,#7628,#7629,#7630,#7631,#7632));
#2000=EDGE_LOOP('',(#7633,#7634,#7635,#7636));
#2001=EDGE_LOOP('',(#7637,#7638,#7639,#7640));
#2002=EDGE_LOOP('',(#7641,#7642,#7643,#7644));
#2003=EDGE_LOOP('',(#7645,#7646,#7647,#7648));
#2004=EDGE_LOOP('',(#7649,#7650,#7651,#7652));
#2005=EDGE_LOOP('',(#7653,#7654,#7655,#7656));
#2006=EDGE_LOOP('',(#7657,#7658,#7659,#7660));
#2007=EDGE_LOOP('',(#7661,#7662,#7663,#7664));
#2008=EDGE_LOOP('',(#7665,#7666,#7667,#7668,#7669,#7670));
#2009=EDGE_LOOP('',(#7671,#7672,#7673,#7674));
#2010=EDGE_LOOP('',(#7675,#7676,#7677,#7678));
#2011=EDGE_LOOP('',(#7679,#7680,#7681,#7682));
#2012=EDGE_LOOP('',(#7683,#7684,#7685,#7686));
#2013=EDGE_LOOP('',(#7687,#7688,#7689,#7690));
#2014=EDGE_LOOP('',(#7691,#7692,#7693,#7694));
#2015=EDGE_LOOP('',(#7695,#7696,#7697,#7698));
#2016=EDGE_LOOP('',(#7699,#7700,#7701,#7702));
#2017=EDGE_LOOP('',(#7703,#7704,#7705,#7706));
#2018=EDGE_LOOP('',(#7707,#7708,#7709,#7710));
#2019=EDGE_LOOP('',(#7711,#7712,#7713,#7714,#7715,#7716,#7717,#7718,#7719,
#7720,#7721,#7722));
#2020=EDGE_LOOP('',(#7723,#7724,#7725,#7726,#7727,#7728,#7729,#7730,#7731,
#7732,#7733,#7734));
#2021=EDGE_LOOP('',(#7735,#7736,#7737,#7738,#7739,#7740));
#2022=EDGE_LOOP('',(#7741,#7742,#7743,#7744));
#2023=EDGE_LOOP('',(#7745,#7746,#7747,#7748));
#2024=EDGE_LOOP('',(#7749,#7750,#7751,#7752));
#2025=EDGE_LOOP('',(#7753,#7754,#7755,#7756));
#2026=EDGE_LOOP('',(#7757,#7758,#7759,#7760));
#2027=EDGE_LOOP('',(#7761,#7762,#7763,#7764));
#2028=EDGE_LOOP('',(#7765,#7766,#7767,#7768));
#2029=EDGE_LOOP('',(#7769,#7770,#7771,#7772));
#2030=EDGE_LOOP('',(#7773,#7774,#7775,#7776,#7777,#7778));
#2031=EDGE_LOOP('',(#7779,#7780,#7781,#7782));
#2032=EDGE_LOOP('',(#7783,#7784,#7785,#7786));
#2033=EDGE_LOOP('',(#7787,#7788,#7789,#7790));
#2034=EDGE_LOOP('',(#7791,#7792,#7793,#7794));
#2035=EDGE_LOOP('',(#7795,#7796,#7797,#7798));
#2036=EDGE_LOOP('',(#7799,#7800,#7801,#7802));
#2037=EDGE_LOOP('',(#7803,#7804,#7805,#7806));
#2038=EDGE_LOOP('',(#7807,#7808,#7809,#7810));
#2039=EDGE_LOOP('',(#7811,#7812,#7813,#7814));
#2040=EDGE_LOOP('',(#7815,#7816,#7817,#7818));
#2041=EDGE_LOOP('',(#7819,#7820,#7821,#7822,#7823,#7824,#7825,#7826,#7827,
#7828,#7829,#7830));
#2042=EDGE_LOOP('',(#7831,#7832,#7833,#7834,#7835,#7836,#7837,#7838,#7839,
#7840,#7841,#7842));
#2043=EDGE_LOOP('',(#7843,#7844,#7845,#7846,#7847,#7848));
#2044=EDGE_LOOP('',(#7849,#7850,#7851,#7852));
#2045=EDGE_LOOP('',(#7853,#7854,#7855,#7856));
#2046=EDGE_LOOP('',(#7857,#7858,#7859,#7860));
#2047=EDGE_LOOP('',(#7861,#7862,#7863,#7864));
#2048=EDGE_LOOP('',(#7865,#7866,#7867,#7868));
#2049=EDGE_LOOP('',(#7869,#7870,#7871,#7872));
#2050=EDGE_LOOP('',(#7873,#7874,#7875,#7876));
#2051=EDGE_LOOP('',(#7877,#7878,#7879,#7880));
#2052=EDGE_LOOP('',(#7881,#7882,#7883,#7884,#7885,#7886));
#2053=EDGE_LOOP('',(#7887,#7888,#7889,#7890));
#2054=EDGE_LOOP('',(#7891,#7892,#7893,#7894));
#2055=EDGE_LOOP('',(#7895,#7896,#7897,#7898));
#2056=EDGE_LOOP('',(#7899,#7900,#7901,#7902));
#2057=EDGE_LOOP('',(#7903,#7904,#7905,#7906));
#2058=EDGE_LOOP('',(#7907,#7908,#7909,#7910));
#2059=EDGE_LOOP('',(#7911,#7912,#7913,#7914));
#2060=EDGE_LOOP('',(#7915,#7916,#7917,#7918));
#2061=EDGE_LOOP('',(#7919,#7920,#7921,#7922));
#2062=EDGE_LOOP('',(#7923,#7924,#7925,#7926));
#2063=EDGE_LOOP('',(#7927,#7928,#7929,#7930,#7931,#7932,#7933,#7934,#7935,
#7936,#7937,#7938));
#2064=EDGE_LOOP('',(#7939,#7940,#7941,#7942,#7943,#7944,#7945,#7946,#7947,
#7948,#7949,#7950));
#2065=EDGE_LOOP('',(#7951,#7952,#7953,#7954,#7955,#7956));
#2066=EDGE_LOOP('',(#7957,#7958,#7959,#7960));
#2067=EDGE_LOOP('',(#7961,#7962,#7963,#7964));
#2068=EDGE_LOOP('',(#7965,#7966,#7967,#7968));
#2069=EDGE_LOOP('',(#7969,#7970,#7971,#7972));
#2070=EDGE_LOOP('',(#7973,#7974,#7975,#7976));
#2071=EDGE_LOOP('',(#7977,#7978,#7979,#7980));
#2072=EDGE_LOOP('',(#7981,#7982,#7983,#7984));
#2073=EDGE_LOOP('',(#7985,#7986,#7987,#7988));
#2074=EDGE_LOOP('',(#7989,#7990,#7991,#7992,#7993,#7994));
#2075=EDGE_LOOP('',(#7995,#7996,#7997,#7998));
#2076=LINE('',#11713,#2693);
#2077=LINE('',#11720,#2694);
#2078=LINE('',#11727,#2695);
#2079=LINE('',#11733,#2696);
#2080=LINE('',#11739,#2697);
#2081=LINE('',#11745,#2698);
#2082=LINE('',#11750,#2699);
#2083=LINE('',#11752,#2700);
#2084=LINE('',#11754,#2701);
#2085=LINE('',#11755,#2702);
#2086=LINE('',#11758,#2703);
#2087=LINE('',#11760,#2704);
#2088=LINE('',#11761,#2705);
#2089=LINE('',#11764,#2706);
#2090=LINE('',#11766,#2707);
#2091=LINE('',#11767,#2708);
#2092=LINE('',#11769,#2709);
#2093=LINE('',#11770,#2710);
#2094=LINE('',#11777,#2711);
#2095=LINE('',#11804,#2712);
#2096=LINE('',#11858,#2713);
#2097=LINE('',#11918,#2714);
#2098=LINE('',#11975,#2715);
#2099=LINE('',#12035,#2716);
#2100=LINE('',#12095,#2717);
#2101=LINE('',#12152,#2718);
#2102=LINE('',#12212,#2719);
#2103=LINE('',#12272,#2720);
#2104=LINE('',#12332,#2721);
#2105=LINE('',#12392,#2722);
#2106=LINE('',#12452,#2723);
#2107=LINE('',#12509,#2724);
#2108=LINE('',#12569,#2725);
#2109=LINE('',#12629,#2726);
#2110=LINE('',#12689,#2727);
#2111=LINE('',#12749,#2728);
#2112=LINE('',#12806,#2729);
#2113=LINE('',#12866,#2730);
#2114=LINE('',#12926,#2731);
#2115=LINE('',#12986,#2732);
#2116=LINE('',#13046,#2733);
#2117=LINE('',#13100,#2734);
#2118=LINE('',#13160,#2735);
#2119=LINE('',#13220,#2736);
#2120=LINE('',#13280,#2737);
#2121=LINE('',#13337,#2738);
#2122=LINE('',#13397,#2739);
#2123=LINE('',#13457,#2740);
#2124=LINE('',#13517,#2741);
#2125=LINE('',#13577,#2742);
#2126=LINE('',#13637,#2743);
#2127=LINE('',#13697,#2744);
#2128=LINE('',#13757,#2745);
#2129=LINE('',#13817,#2746);
#2130=LINE('',#13877,#2747);
#2131=LINE('',#13934,#2748);
#2132=LINE('',#13994,#2749);
#2133=LINE('',#14054,#2750);
#2134=LINE('',#14114,#2751);
#2135=LINE('',#14174,#2752);
#2136=LINE('',#14231,#2753);
#2137=LINE('',#14291,#2754);
#2138=LINE('',#14351,#2755);
#2139=LINE('',#14411,#2756);
#2140=LINE('',#14471,#2757);
#2141=LINE('',#14531,#2758);
#2142=LINE('',#14591,#2759);
#2143=LINE('',#14648,#2760);
#2144=LINE('',#14708,#2761);
#2145=LINE('',#14768,#2762);
#2146=LINE('',#14828,#2763);
#2147=LINE('',#14888,#2764);
#2148=LINE('',#14945,#2765);
#2149=LINE('',#15005,#2766);
#2150=LINE('',#15065,#2767);
#2151=LINE('',#15125,#2768);
#2152=LINE('',#15185,#2769);
#2153=LINE('',#15245,#2770);
#2154=LINE('',#15302,#2771);
#2155=LINE('',#15362,#2772);
#2156=LINE('',#15422,#2773);
#2157=LINE('',#15482,#2774);
#2158=LINE('',#15542,#2775);
#2159=LINE('',#15599,#2776);
#2160=LINE('',#15659,#2777);
#2161=LINE('',#15719,#2778);
#2162=LINE('',#15779,#2779);
#2163=LINE('',#15836,#2780);
#2164=LINE('',#15896,#2781);
#2165=LINE('',#15956,#2782);
#2166=LINE('',#16016,#2783);
#2167=LINE('',#16076,#2784);
#2168=LINE('',#16136,#2785);
#2169=LINE('',#16196,#2786);
#2170=LINE('',#16256,#2787);
#2171=LINE('',#16316,#2788);
#2172=LINE('',#16376,#2789);
#2173=LINE('',#16433,#2790);
#2174=LINE('',#16493,#2791);
#2175=LINE('',#16553,#2792);
#2176=LINE('',#16613,#2793);
#2177=LINE('',#16673,#2794);
#2178=LINE('',#16730,#2795);
#2179=LINE('',#16790,#2796);
#2180=LINE('',#16850,#2797);
#2181=LINE('',#16910,#2798);
#2182=LINE('',#16970,#2799);
#2183=LINE('',#17030,#2800);
#2184=LINE('',#17090,#2801);
#2185=LINE('',#17150,#2802);
#2186=LINE('',#17210,#2803);
#2187=LINE('',#17270,#2804);
#2188=LINE('',#17327,#2805);
#2189=LINE('',#17349,#2806);
#2190=LINE('',#17409,#2807);
#2191=LINE('',#17466,#2808);
#2192=LINE('',#17526,#2809);
#2193=LINE('',#17586,#2810);
#2194=LINE('',#17629,#2811);
#2195=LINE('',#17672,#2812);
#2196=LINE('',#17714,#2813);
#2197=LINE('',#17774,#2814);
#2198=LINE('',#17834,#2815);
#2199=LINE('',#17894,#2816);
#2200=LINE('',#17954,#2817);
#2201=LINE('',#17997,#2818);
#2202=LINE('',#18057,#2819);
#2203=LINE('',#18117,#2820);
#2204=LINE('',#18177,#2821);
#2205=LINE('',#18220,#2822);
#2206=LINE('',#18280,#2823);
#2207=LINE('',#18340,#2824);
#2208=LINE('',#18400,#2825);
#2209=LINE('',#18460,#2826);
#2210=LINE('',#18503,#2827);
#2211=LINE('',#18563,#2828);
#2212=LINE('',#18623,#2829);
#2213=LINE('',#18683,#2830);
#2214=LINE('',#18743,#2831);
#2215=LINE('',#18768,#2832);
#2216=LINE('',#18812,#2833);
#2217=LINE('',#18872,#2834);
#2218=LINE('',#18932,#2835);
#2219=LINE('',#18975,#2836);
#2220=LINE('',#19018,#2837);
#2221=LINE('',#19061,#2838);
#2222=LINE('',#19121,#2839);
#2223=LINE('',#19181,#2840);
#2224=LINE('',#19224,#2841);
#2225=LINE('',#19267,#2842);
#2226=LINE('',#19327,#2843);
#2227=LINE('',#19387,#2844);
#2228=LINE('',#19447,#2845);
#2229=LINE('',#19507,#2846);
#2230=LINE('',#19550,#2847);
#2231=LINE('',#19593,#2848);
#2232=LINE('',#19653,#2849);
#2233=LINE('',#19713,#2850);
#2234=LINE('',#19756,#2851);
#2235=LINE('',#19799,#2852);
#2236=LINE('',#19842,#2853);
#2237=LINE('',#19902,#2854);
#2238=LINE('',#19945,#2855);
#2239=LINE('',#20005,#2856);
#2240=LINE('',#20065,#2857);
#2241=LINE('',#20125,#2858);
#2242=LINE('',#20185,#2859);
#2243=LINE('',#20228,#2860);
#2244=LINE('',#20288,#2861);
#2245=LINE('',#20348,#2862);
#2246=LINE('',#20408,#2863);
#2247=LINE('',#20451,#2864);
#2248=LINE('',#20511,#2865);
#2249=LINE('',#20571,#2866);
#2250=LINE('',#20631,#2867);
#2251=LINE('',#20691,#2868);
#2252=LINE('',#20733,#2869);
#2253=LINE('',#20793,#2870);
#2254=LINE('',#20836,#2871);
#2255=LINE('',#20896,#2872);
#2256=LINE('',#20956,#2873);
#2257=LINE('',#20999,#2874);
#2258=LINE('',#21043,#2875);
#2259=LINE('',#21103,#2876);
#2260=LINE('',#21163,#2877);
#2261=LINE('',#21206,#2878);
#2262=LINE('',#21249,#2879);
#2263=LINE('',#21309,#2880);
#2264=LINE('',#21369,#2881);
#2265=LINE('',#21429,#2882);
#2266=LINE('',#21472,#2883);
#2267=LINE('',#21515,#2884);
#2268=LINE('',#21575,#2885);
#2269=LINE('',#21635,#2886);
#2270=LINE('',#21695,#2887);
#2271=LINE('',#21755,#2888);
#2272=LINE('',#21798,#2889);
#2273=LINE('',#21825,#2890);
#2274=LINE('',#21885,#2891);
#2275=LINE('',#21928,#2892);
#2276=LINE('',#21971,#2893);
#2277=LINE('',#22014,#2894);
#2278=LINE('',#22057,#2895);
#2279=LINE('',#22117,#2896);
#2280=LINE('',#22177,#2897);
#2281=LINE('',#22220,#2898);
#2282=LINE('',#22247,#2899);
#2283=LINE('',#22253,#2900);
#2284=LINE('',#22259,#2901);
#2285=LINE('',#22265,#2902);
#2286=LINE('',#22271,#2903);
#2287=LINE('',#22277,#2904);
#2288=LINE('',#22383,#2905);
#2289=LINE('',#28019,#2906);
#2290=LINE('',#28028,#2907);
#2291=LINE('',#28038,#2908);
#2292=LINE('',#28041,#2909);
#2293=LINE('',#28044,#2910);
#2294=LINE('',#28048,#2911);
#2295=LINE('',#28050,#2912);
#2296=LINE('',#28052,#2913);
#2297=LINE('',#28055,#2914);
#2298=LINE('',#28058,#2915);
#2299=LINE('',#28059,#2916);
#2300=LINE('',#28064,#2917);
#2301=LINE('',#28069,#2918);
#2302=LINE('',#28073,#2919);
#2303=LINE('',#28077,#2920);
#2304=LINE('',#28079,#2921);
#2305=LINE('',#28080,#2922);
#2306=LINE('',#28083,#2923);
#2307=LINE('',#28085,#2924);
#2308=LINE('',#28087,#2925);
#2309=LINE('',#28089,#2926);
#2310=LINE('',#28090,#2927);
#2311=LINE('',#28093,#2928);
#2312=LINE('',#28094,#2929);
#2313=LINE('',#28097,#2930);
#2314=LINE('',#28098,#2931);
#2315=LINE('',#28100,#2932);
#2316=LINE('',#28101,#2933);
#2317=LINE('',#28104,#2934);
#2318=LINE('',#28105,#2935);
#2319=LINE('',#28108,#2936);
#2320=LINE('',#28109,#2937);
#2321=LINE('',#28112,#2938);
#2322=LINE('',#28117,#2939);
#2323=LINE('',#28123,#2940);
#2324=LINE('',#28128,#2941);
#2325=LINE('',#28130,#2942);
#2326=LINE('',#28132,#2943);
#2327=LINE('',#28133,#2944);
#2328=LINE('',#28136,#2945);
#2329=LINE('',#28138,#2946);
#2330=LINE('',#28139,#2947);
#2331=LINE('',#28142,#2948);
#2332=LINE('',#28144,#2949);
#2333=LINE('',#28145,#2950);
#2334=LINE('',#28147,#2951);
#2335=LINE('',#28148,#2952);
#2336=LINE('',#28155,#2953);
#2337=LINE('',#28160,#2954);
#2338=LINE('',#28162,#2955);
#2339=LINE('',#28164,#2956);
#2340=LINE('',#28165,#2957);
#2341=LINE('',#28168,#2958);
#2342=LINE('',#28170,#2959);
#2343=LINE('',#28171,#2960);
#2344=LINE('',#28174,#2961);
#2345=LINE('',#28176,#2962);
#2346=LINE('',#28177,#2963);
#2347=LINE('',#28179,#2964);
#2348=LINE('',#28180,#2965);
#2349=LINE('',#28187,#2966);
#2350=LINE('',#28191,#2967);
#2351=LINE('',#28195,#2968);
#2352=LINE('',#28198,#2969);
#2353=LINE('',#28201,#2970);
#2354=LINE('',#28202,#2971);
#2355=LINE('',#28205,#2972);
#2356=LINE('',#28206,#2973);
#2357=LINE('',#28214,#2974);
#2358=LINE('',#28219,#2975);
#2359=LINE('',#28221,#2976);
#2360=LINE('',#28223,#2977);
#2361=LINE('',#28224,#2978);
#2362=LINE('',#28227,#2979);
#2363=LINE('',#28229,#2980);
#2364=LINE('',#28230,#2981);
#2365=LINE('',#28233,#2982);
#2366=LINE('',#28235,#2983);
#2367=LINE('',#28236,#2984);
#2368=LINE('',#28238,#2985);
#2369=LINE('',#28239,#2986);
#2370=LINE('',#28246,#2987);
#2371=LINE('',#28251,#2988);
#2372=LINE('',#28253,#2989);
#2373=LINE('',#28255,#2990);
#2374=LINE('',#28256,#2991);
#2375=LINE('',#28259,#2992);
#2376=LINE('',#28261,#2993);
#2377=LINE('',#28262,#2994);
#2378=LINE('',#28265,#2995);
#2379=LINE('',#28267,#2996);
#2380=LINE('',#28268,#2997);
#2381=LINE('',#28270,#2998);
#2382=LINE('',#28271,#2999);
#2383=LINE('',#28278,#3000);
#2384=LINE('',#28280,#3001);
#2385=LINE('',#28282,#3002);
#2386=LINE('',#28283,#3003);
#2387=LINE('',#28287,#3004);
#2388=LINE('',#28289,#3005);
#2389=LINE('',#28291,#3006);
#2390=LINE('',#28292,#3007);
#2391=LINE('',#28305,#3008);
#2392=LINE('',#28307,#3009);
#2393=LINE('',#28309,#3010);
#2394=LINE('',#28310,#3011);
#2395=LINE('',#28314,#3012);
#2396=LINE('',#28316,#3013);
#2397=LINE('',#28318,#3014);
#2398=LINE('',#28319,#3015);
#2399=LINE('',#28332,#3016);
#2400=LINE('',#28336,#3017);
#2401=LINE('',#28340,#3018);
#2402=LINE('',#28344,#3019);
#2403=LINE('',#28348,#3020);
#2404=LINE('',#28350,#3021);
#2405=LINE('',#28351,#3022);
#2406=LINE('',#28354,#3023);
#2407=LINE('',#28357,#3024);
#2408=LINE('',#28360,#3025);
#2409=LINE('',#28361,#3026);
#2410=LINE('',#28364,#3027);
#2411=LINE('',#28366,#3028);
#2412=LINE('',#28368,#3029);
#2413=LINE('',#28369,#3030);
#2414=LINE('',#28374,#3031);
#2415=LINE('',#28379,#3032);
#2416=LINE('',#28383,#3033);
#2417=LINE('',#28386,#3034);
#2418=LINE('',#28387,#3035);
#2419=LINE('',#28390,#3036);
#2420=LINE('',#28392,#3037);
#2421=LINE('',#28394,#3038);
#2422=LINE('',#28395,#3039);
#2423=LINE('',#28398,#3040);
#2424=LINE('',#28399,#3041);
#2425=LINE('',#28402,#3042);
#2426=LINE('',#28403,#3043);
#2427=LINE('',#28405,#3044);
#2428=LINE('',#28407,#3045);
#2429=LINE('',#28410,#3046);
#2430=LINE('',#28411,#3047);
#2431=LINE('',#28419,#3048);
#2432=LINE('',#28424,#3049);
#2433=LINE('',#28426,#3050);
#2434=LINE('',#28428,#3051);
#2435=LINE('',#28429,#3052);
#2436=LINE('',#28432,#3053);
#2437=LINE('',#28434,#3054);
#2438=LINE('',#28435,#3055);
#2439=LINE('',#28438,#3056);
#2440=LINE('',#28440,#3057);
#2441=LINE('',#28441,#3058);
#2442=LINE('',#28443,#3059);
#2443=LINE('',#28444,#3060);
#2444=LINE('',#28451,#3061);
#2445=LINE('',#28456,#3062);
#2446=LINE('',#28458,#3063);
#2447=LINE('',#28460,#3064);
#2448=LINE('',#28461,#3065);
#2449=LINE('',#28464,#3066);
#2450=LINE('',#28466,#3067);
#2451=LINE('',#28467,#3068);
#2452=LINE('',#28470,#3069);
#2453=LINE('',#28472,#3070);
#2454=LINE('',#28473,#3071);
#2455=LINE('',#28475,#3072);
#2456=LINE('',#28476,#3073);
#2457=LINE('',#28483,#3074);
#2458=LINE('',#28487,#3075);
#2459=LINE('',#28491,#3076);
#2460=LINE('',#28494,#3077);
#2461=LINE('',#28497,#3078);
#2462=LINE('',#28498,#3079);
#2463=LINE('',#28501,#3080);
#2464=LINE('',#28502,#3081);
#2465=LINE('',#28510,#3082);
#2466=LINE('',#28515,#3083);
#2467=LINE('',#28517,#3084);
#2468=LINE('',#28519,#3085);
#2469=LINE('',#28520,#3086);
#2470=LINE('',#28523,#3087);
#2471=LINE('',#28525,#3088);
#2472=LINE('',#28526,#3089);
#2473=LINE('',#28529,#3090);
#2474=LINE('',#28531,#3091);
#2475=LINE('',#28532,#3092);
#2476=LINE('',#28534,#3093);
#2477=LINE('',#28535,#3094);
#2478=LINE('',#28542,#3095);
#2479=LINE('',#28547,#3096);
#2480=LINE('',#28549,#3097);
#2481=LINE('',#28551,#3098);
#2482=LINE('',#28552,#3099);
#2483=LINE('',#28555,#3100);
#2484=LINE('',#28557,#3101);
#2485=LINE('',#28558,#3102);
#2486=LINE('',#28561,#3103);
#2487=LINE('',#28563,#3104);
#2488=LINE('',#28564,#3105);
#2489=LINE('',#28566,#3106);
#2490=LINE('',#28567,#3107);
#2491=LINE('',#28574,#3108);
#2492=LINE('',#28576,#3109);
#2493=LINE('',#28578,#3110);
#2494=LINE('',#28579,#3111);
#2495=LINE('',#28583,#3112);
#2496=LINE('',#28585,#3113);
#2497=LINE('',#28587,#3114);
#2498=LINE('',#28588,#3115);
#2499=LINE('',#28601,#3116);
#2500=LINE('',#28603,#3117);
#2501=LINE('',#28605,#3118);
#2502=LINE('',#28606,#3119);
#2503=LINE('',#28610,#3120);
#2504=LINE('',#28612,#3121);
#2505=LINE('',#28614,#3122);
#2506=LINE('',#28615,#3123);
#2507=LINE('',#28628,#3124);
#2508=LINE('',#28630,#3125);
#2509=LINE('',#28632,#3126);
#2510=LINE('',#28633,#3127);
#2511=LINE('',#28636,#3128);
#2512=LINE('',#28638,#3129);
#2513=LINE('',#28639,#3130);
#2514=LINE('',#28642,#3131);
#2515=LINE('',#28644,#3132);
#2516=LINE('',#28645,#3133);
#2517=LINE('',#28647,#3134);
#2518=LINE('',#28648,#3135);
#2519=LINE('',#28655,#3136);
#2520=LINE('',#28657,#3137);
#2521=LINE('',#28659,#3138);
#2522=LINE('',#28660,#3139);
#2523=LINE('',#28663,#3140);
#2524=LINE('',#28665,#3141);
#2525=LINE('',#28666,#3142);
#2526=LINE('',#28669,#3143);
#2527=LINE('',#28671,#3144);
#2528=LINE('',#28672,#3145);
#2529=LINE('',#28674,#3146);
#2530=LINE('',#28675,#3147);
#2531=LINE('',#28682,#3148);
#2532=LINE('',#28684,#3149);
#2533=LINE('',#28686,#3150);
#2534=LINE('',#28687,#3151);
#2535=LINE('',#28690,#3152);
#2536=LINE('',#28692,#3153);
#2537=LINE('',#28693,#3154);
#2538=LINE('',#28696,#3155);
#2539=LINE('',#28698,#3156);
#2540=LINE('',#28699,#3157);
#2541=LINE('',#28702,#3158);
#2542=LINE('',#28704,#3159);
#2543=LINE('',#28705,#3160);
#2544=LINE('',#28708,#3161);
#2545=LINE('',#28710,#3162);
#2546=LINE('',#28711,#3163);
#2547=LINE('',#28713,#3164);
#2548=LINE('',#28714,#3165);
#2549=LINE('',#28726,#3166);
#2550=LINE('',#28730,#3167);
#2551=LINE('',#28734,#3168);
#2552=LINE('',#28741,#3169);
#2553=LINE('',#28743,#3170);
#2554=LINE('',#28748,#3171);
#2555=LINE('',#28750,#3172);
#2556=LINE('',#28752,#3173);
#2557=LINE('',#28753,#3174);
#2558=LINE('',#28756,#3175);
#2559=LINE('',#28758,#3176);
#2560=LINE('',#28759,#3177);
#2561=LINE('',#28762,#3178);
#2562=LINE('',#28764,#3179);
#2563=LINE('',#28765,#3180);
#2564=LINE('',#28768,#3181);
#2565=LINE('',#28770,#3182);
#2566=LINE('',#28771,#3183);
#2567=LINE('',#28774,#3184);
#2568=LINE('',#28776,#3185);
#2569=LINE('',#28777,#3186);
#2570=LINE('',#28779,#3187);
#2571=LINE('',#28780,#3188);
#2572=LINE('',#28790,#3189);
#2573=LINE('',#28799,#3190);
#2574=LINE('',#28803,#3191);
#2575=LINE('',#28807,#3192);
#2576=LINE('',#28814,#3193);
#2577=LINE('',#28816,#3194);
#2578=LINE('',#28822,#3195);
#2579=LINE('',#28828,#3196);
#2580=LINE('',#28844,#3197);
#2581=LINE('',#28865,#3198);
#2582=LINE('',#28890,#3199);
#2583=LINE('',#28891,#3200);
#2584=LINE('',#28893,#3201);
#2585=LINE('',#28895,#3202);
#2586=LINE('',#28900,#3203);
#2587=LINE('',#28903,#3204);
#2588=LINE('',#28905,#3205);
#2589=LINE('',#28948,#3206);
#2590=LINE('',#28981,#3207);
#2591=LINE('',#29071,#3208);
#2592=LINE('',#29161,#3209);
#2593=LINE('',#29230,#3210);
#2594=LINE('',#29264,#3211);
#2595=LINE('',#29302,#3212);
#2596=LINE('',#29340,#3213);
#2597=LINE('',#30263,#3214);
#2598=LINE('',#30265,#3215);
#2599=LINE('',#30267,#3216);
#2600=LINE('',#30269,#3217);
#2601=LINE('',#30271,#3218);
#2602=LINE('',#30272,#3219);
#2603=LINE('',#30277,#3220);
#2604=LINE('',#30278,#3221);
#2605=LINE('',#30279,#3222);
#2606=LINE('',#30282,#3223);
#2607=LINE('',#30283,#3224);
#2608=LINE('',#30286,#3225);
#2609=LINE('',#30287,#3226);
#2610=LINE('',#30290,#3227);
#2611=LINE('',#30291,#3228);
#2612=LINE('',#30294,#3229);
#2613=LINE('',#30295,#3230);
#2614=LINE('',#30297,#3231);
#2615=LINE('',#30305,#3232);
#2616=LINE('',#30338,#3233);
#2617=LINE('',#30428,#3234);
#2618=LINE('',#30518,#3235);
#2619=LINE('',#30587,#3236);
#2620=LINE('',#30621,#3237);
#2621=LINE('',#30659,#3238);
#2622=LINE('',#30697,#3239);
#2623=LINE('',#31620,#3240);
#2624=LINE('',#31622,#3241);
#2625=LINE('',#31624,#3242);
#2626=LINE('',#31626,#3243);
#2627=LINE('',#31628,#3244);
#2628=LINE('',#31629,#3245);
#2629=LINE('',#31634,#3246);
#2630=LINE('',#31635,#3247);
#2631=LINE('',#31636,#3248);
#2632=LINE('',#31639,#3249);
#2633=LINE('',#31640,#3250);
#2634=LINE('',#31643,#3251);
#2635=LINE('',#31644,#3252);
#2636=LINE('',#31647,#3253);
#2637=LINE('',#31648,#3254);
#2638=LINE('',#31651,#3255);
#2639=LINE('',#31652,#3256);
#2640=LINE('',#31654,#3257);
#2641=LINE('',#31662,#3258);
#2642=LINE('',#31695,#3259);
#2643=LINE('',#31785,#3260);
#2644=LINE('',#31875,#3261);
#2645=LINE('',#31944,#3262);
#2646=LINE('',#31978,#3263);
#2647=LINE('',#32016,#3264);
#2648=LINE('',#32054,#3265);
#2649=LINE('',#32977,#3266);
#2650=LINE('',#32979,#3267);
#2651=LINE('',#32981,#3268);
#2652=LINE('',#32983,#3269);
#2653=LINE('',#32985,#3270);
#2654=LINE('',#32986,#3271);
#2655=LINE('',#32991,#3272);
#2656=LINE('',#32992,#3273);
#2657=LINE('',#32993,#3274);
#2658=LINE('',#32996,#3275);
#2659=LINE('',#32997,#3276);
#2660=LINE('',#33000,#3277);
#2661=LINE('',#33001,#3278);
#2662=LINE('',#33004,#3279);
#2663=LINE('',#33005,#3280);
#2664=LINE('',#33008,#3281);
#2665=LINE('',#33009,#3282);
#2666=LINE('',#33011,#3283);
#2667=LINE('',#33019,#3284);
#2668=LINE('',#33052,#3285);
#2669=LINE('',#33142,#3286);
#2670=LINE('',#33232,#3287);
#2671=LINE('',#33301,#3288);
#2672=LINE('',#33335,#3289);
#2673=LINE('',#33373,#3290);
#2674=LINE('',#33411,#3291);
#2675=LINE('',#34334,#3292);
#2676=LINE('',#34336,#3293);
#2677=LINE('',#34338,#3294);
#2678=LINE('',#34340,#3295);
#2679=LINE('',#34342,#3296);
#2680=LINE('',#34343,#3297);
#2681=LINE('',#34348,#3298);
#2682=LINE('',#34349,#3299);
#2683=LINE('',#34350,#3300);
#2684=LINE('',#34353,#3301);
#2685=LINE('',#34354,#3302);
#2686=LINE('',#34357,#3303);
#2687=LINE('',#34358,#3304);
#2688=LINE('',#34361,#3305);
#2689=LINE('',#34362,#3306);
#2690=LINE('',#34365,#3307);
#2691=LINE('',#34366,#3308);
#2692=LINE('',#34368,#3309);
#2693=VECTOR('',#9735,0.15);
#2694=VECTOR('',#9744,0.15);
#2695=VECTOR('',#9753,0.25);
#2696=VECTOR('',#9760,0.25);
#2697=VECTOR('',#9767,0.25);
#2698=VECTOR('',#9774,0.25);
#2699=VECTOR('',#9779,1.);
#2700=VECTOR('',#9780,1.);
#2701=VECTOR('',#9781,1.);
#2702=VECTOR('',#9782,1.);
#2703=VECTOR('',#9785,1.);
#2704=VECTOR('',#9786,1.);
#2705=VECTOR('',#9787,1.);
#2706=VECTOR('',#9790,1.);
#2707=VECTOR('',#9791,1.);
#2708=VECTOR('',#9792,1.);
#2709=VECTOR('',#9795,1.);
#2710=VECTOR('',#9796,1.);
#2711=VECTOR('',#9805,1.2);
#2712=VECTOR('',#9810,1.2);
#2713=VECTOR('',#9813,1.2);
#2714=VECTOR('',#9816,1.2);
#2715=VECTOR('',#9819,1.2);
#2716=VECTOR('',#9822,1.2);
#2717=VECTOR('',#9825,1.2);
#2718=VECTOR('',#9828,1.2);
#2719=VECTOR('',#9831,1.2);
#2720=VECTOR('',#9834,1.2);
#2721=VECTOR('',#9837,1.2);
#2722=VECTOR('',#9840,1.2);
#2723=VECTOR('',#9843,1.2);
#2724=VECTOR('',#9846,1.2);
#2725=VECTOR('',#9849,1.2);
#2726=VECTOR('',#9852,1.2);
#2727=VECTOR('',#9855,1.2);
#2728=VECTOR('',#9858,1.2);
#2729=VECTOR('',#9861,1.2);
#2730=VECTOR('',#9864,1.2);
#2731=VECTOR('',#9867,1.2);
#2732=VECTOR('',#9870,1.2);
#2733=VECTOR('',#9873,1.2);
#2734=VECTOR('',#9876,1.2);
#2735=VECTOR('',#9879,1.2);
#2736=VECTOR('',#9882,1.2);
#2737=VECTOR('',#9885,1.2);
#2738=VECTOR('',#9888,1.2);
#2739=VECTOR('',#9891,1.2);
#2740=VECTOR('',#9894,1.2);
#2741=VECTOR('',#9897,1.2);
#2742=VECTOR('',#9900,1.2);
#2743=VECTOR('',#9903,1.2);
#2744=VECTOR('',#9906,1.2);
#2745=VECTOR('',#9909,1.2);
#2746=VECTOR('',#9912,1.2);
#2747=VECTOR('',#9915,1.2);
#2748=VECTOR('',#9918,1.2);
#2749=VECTOR('',#9921,1.2);
#2750=VECTOR('',#9924,1.2);
#2751=VECTOR('',#9927,1.2);
#2752=VECTOR('',#9930,1.2);
#2753=VECTOR('',#9933,1.2);
#2754=VECTOR('',#9936,1.2);
#2755=VECTOR('',#9939,1.2);
#2756=VECTOR('',#9942,1.2);
#2757=VECTOR('',#9945,1.2);
#2758=VECTOR('',#9948,1.2);
#2759=VECTOR('',#9951,1.2);
#2760=VECTOR('',#9954,1.2);
#2761=VECTOR('',#9957,1.2);
#2762=VECTOR('',#9960,1.2);
#2763=VECTOR('',#9963,1.2);
#2764=VECTOR('',#9966,1.2);
#2765=VECTOR('',#9969,1.2);
#2766=VECTOR('',#9972,1.2);
#2767=VECTOR('',#9975,1.2);
#2768=VECTOR('',#9978,1.2);
#2769=VECTOR('',#9981,1.2);
#2770=VECTOR('',#9984,1.2);
#2771=VECTOR('',#9987,1.2);
#2772=VECTOR('',#9990,1.2);
#2773=VECTOR('',#9993,1.2);
#2774=VECTOR('',#9996,1.2);
#2775=VECTOR('',#9999,1.2);
#2776=VECTOR('',#10002,1.2);
#2777=VECTOR('',#10005,1.2);
#2778=VECTOR('',#10008,1.2);
#2779=VECTOR('',#10011,1.2);
#2780=VECTOR('',#10014,1.2);
#2781=VECTOR('',#10017,1.2);
#2782=VECTOR('',#10020,1.2);
#2783=VECTOR('',#10023,1.2);
#2784=VECTOR('',#10026,1.2);
#2785=VECTOR('',#10029,1.2);
#2786=VECTOR('',#10032,1.2);
#2787=VECTOR('',#10035,1.2);
#2788=VECTOR('',#10038,1.2);
#2789=VECTOR('',#10041,1.2);
#2790=VECTOR('',#10044,1.2);
#2791=VECTOR('',#10047,1.2);
#2792=VECTOR('',#10050,1.2);
#2793=VECTOR('',#10053,1.2);
#2794=VECTOR('',#10056,1.2);
#2795=VECTOR('',#10059,1.2);
#2796=VECTOR('',#10062,1.2);
#2797=VECTOR('',#10065,1.2);
#2798=VECTOR('',#10068,1.2);
#2799=VECTOR('',#10071,1.2);
#2800=VECTOR('',#10074,1.2);
#2801=VECTOR('',#10077,1.2);
#2802=VECTOR('',#10080,1.2);
#2803=VECTOR('',#10083,1.2);
#2804=VECTOR('',#10086,1.2);
#2805=VECTOR('',#10089,1.016475);
#2806=VECTOR('',#10094,1.016475);
#2807=VECTOR('',#10097,1.016475);
#2808=VECTOR('',#10100,1.016475);
#2809=VECTOR('',#10103,1.016475);
#2810=VECTOR('',#10106,1.016475);
#2811=VECTOR('',#10109,1.016475);
#2812=VECTOR('',#10112,1.016475);
#2813=VECTOR('',#10115,1.016475);
#2814=VECTOR('',#10118,1.016475);
#2815=VECTOR('',#10121,1.016475);
#2816=VECTOR('',#10124,1.016475);
#2817=VECTOR('',#10127,1.016475);
#2818=VECTOR('',#10130,1.016475);
#2819=VECTOR('',#10133,1.016475);
#2820=VECTOR('',#10136,1.016475);
#2821=VECTOR('',#10139,1.016475);
#2822=VECTOR('',#10142,1.016475);
#2823=VECTOR('',#10145,1.016475);
#2824=VECTOR('',#10148,1.016475);
#2825=VECTOR('',#10151,1.016475);
#2826=VECTOR('',#10154,1.016475);
#2827=VECTOR('',#10157,1.016475);
#2828=VECTOR('',#10160,1.016475);
#2829=VECTOR('',#10163,1.016475);
#2830=VECTOR('',#10166,1.016475);
#2831=VECTOR('',#10169,1.016475);
#2832=VECTOR('',#10172,1.016475);
#2833=VECTOR('',#10175,1.016475);
#2834=VECTOR('',#10178,1.016475);
#2835=VECTOR('',#10181,1.016475);
#2836=VECTOR('',#10184,1.016475);
#2837=VECTOR('',#10187,1.016475);
#2838=VECTOR('',#10190,1.016475);
#2839=VECTOR('',#10193,1.016475);
#2840=VECTOR('',#10196,1.016475);
#2841=VECTOR('',#10199,1.016475);
#2842=VECTOR('',#10202,1.016475);
#2843=VECTOR('',#10205,1.016475);
#2844=VECTOR('',#10208,1.016475);
#2845=VECTOR('',#10211,1.016475);
#2846=VECTOR('',#10214,1.016475);
#2847=VECTOR('',#10217,1.016475);
#2848=VECTOR('',#10220,1.016475);
#2849=VECTOR('',#10223,1.016475);
#2850=VECTOR('',#10226,1.016475);
#2851=VECTOR('',#10229,1.016475);
#2852=VECTOR('',#10232,1.016475);
#2853=VECTOR('',#10235,1.016475);
#2854=VECTOR('',#10238,1.016475);
#2855=VECTOR('',#10241,1.016475);
#2856=VECTOR('',#10244,1.016475);
#2857=VECTOR('',#10247,1.016475);
#2858=VECTOR('',#10250,1.016475);
#2859=VECTOR('',#10253,1.016475);
#2860=VECTOR('',#10256,1.016475);
#2861=VECTOR('',#10259,1.016475);
#2862=VECTOR('',#10262,1.016475);
#2863=VECTOR('',#10265,1.016475);
#2864=VECTOR('',#10268,1.016475);
#2865=VECTOR('',#10271,1.016475);
#2866=VECTOR('',#10274,1.016475);
#2867=VECTOR('',#10277,1.016475);
#2868=VECTOR('',#10280,1.016475);
#2869=VECTOR('',#10283,1.016475);
#2870=VECTOR('',#10286,1.016475);
#2871=VECTOR('',#10289,1.016475);
#2872=VECTOR('',#10292,1.016475);
#2873=VECTOR('',#10295,1.016475);
#2874=VECTOR('',#10298,1.016475);
#2875=VECTOR('',#10301,1.016475);
#2876=VECTOR('',#10304,1.016475);
#2877=VECTOR('',#10307,1.016475);
#2878=VECTOR('',#10310,1.016475);
#2879=VECTOR('',#10313,1.016475);
#2880=VECTOR('',#10316,1.016475);
#2881=VECTOR('',#10319,1.016475);
#2882=VECTOR('',#10322,1.016475);
#2883=VECTOR('',#10325,1.016475);
#2884=VECTOR('',#10328,1.016475);
#2885=VECTOR('',#10331,1.016475);
#2886=VECTOR('',#10334,1.016475);
#2887=VECTOR('',#10337,1.016475);
#2888=VECTOR('',#10340,1.016475);
#2889=VECTOR('',#10343,1.016475);
#2890=VECTOR('',#10346,1.016475);
#2891=VECTOR('',#10349,1.016475);
#2892=VECTOR('',#10352,1.016475);
#2893=VECTOR('',#10355,1.016475);
#2894=VECTOR('',#10358,1.016475);
#2895=VECTOR('',#10361,1.016475);
#2896=VECTOR('',#10364,1.016475);
#2897=VECTOR('',#10367,1.016475);
#2898=VECTOR('',#10370,1.016475);
#2899=VECTOR('',#10375,0.15);
#2900=VECTOR('',#10382,0.15);
#2901=VECTOR('',#10389,0.33);
#2902=VECTOR('',#10396,0.33);
#2903=VECTOR('',#10403,0.33);
#2904=VECTOR('',#10410,0.33);
#2905=VECTOR('',#10421,3.8);
#2906=VECTOR('',#10440,0.15);
#2907=VECTOR('',#10453,0.15);
#2908=VECTOR('',#10466,1.);
#2909=VECTOR('',#10469,1.);
#2910=VECTOR('',#10472,1.);
#2911=VECTOR('',#10475,1.);
#2912=VECTOR('',#10476,1.);
#2913=VECTOR('',#10477,1.);
#2914=VECTOR('',#10480,1.);
#2915=VECTOR('',#10483,1.);
#2916=VECTOR('',#10484,1.);
#2917=VECTOR('',#10489,1.21);
#2918=VECTOR('',#10494,1.);
#2919=VECTOR('',#10497,1.);
#2920=VECTOR('',#10502,1.);
#2921=VECTOR('',#10503,1.);
#2922=VECTOR('',#10504,1.);
#2923=VECTOR('',#10507,1.);
#2924=VECTOR('',#10508,1.);
#2925=VECTOR('',#10509,1.);
#2926=VECTOR('',#10510,1.);
#2927=VECTOR('',#10511,1.);
#2928=VECTOR('',#10514,1.);
#2929=VECTOR('',#10515,1.);
#2930=VECTOR('',#10518,1.);
#2931=VECTOR('',#10519,1.);
#2932=VECTOR('',#10522,1.);
#2933=VECTOR('',#10523,1.);
#2934=VECTOR('',#10526,1.);
#2935=VECTOR('',#10527,1.);
#2936=VECTOR('',#10530,1.);
#2937=VECTOR('',#10531,1.);
#2938=VECTOR('',#10534,1.);
#2939=VECTOR('',#10543,1.);
#2940=VECTOR('',#10550,0.425);
#2941=VECTOR('',#10555,1.);
#2942=VECTOR('',#10556,1.);
#2943=VECTOR('',#10557,1.);
#2944=VECTOR('',#10558,1.);
#2945=VECTOR('',#10561,1.);
#2946=VECTOR('',#10562,1.);
#2947=VECTOR('',#10563,1.);
#2948=VECTOR('',#10566,1.);
#2949=VECTOR('',#10567,1.);
#2950=VECTOR('',#10568,1.);
#2951=VECTOR('',#10571,1.);
#2952=VECTOR('',#10572,1.);
#2953=VECTOR('',#10581,0.425);
#2954=VECTOR('',#10586,1.);
#2955=VECTOR('',#10587,1.);
#2956=VECTOR('',#10588,1.);
#2957=VECTOR('',#10589,1.);
#2958=VECTOR('',#10592,1.);
#2959=VECTOR('',#10593,1.);
#2960=VECTOR('',#10594,1.);
#2961=VECTOR('',#10597,1.);
#2962=VECTOR('',#10598,1.);
#2963=VECTOR('',#10599,1.);
#2964=VECTOR('',#10602,1.);
#2965=VECTOR('',#10603,1.);
#2966=VECTOR('',#10612,1.);
#2967=VECTOR('',#10615,1.);
#2968=VECTOR('',#10620,1.);
#2969=VECTOR('',#10623,1.);
#2970=VECTOR('',#10626,1.);
#2971=VECTOR('',#10627,1.);
#2972=VECTOR('',#10630,1.);
#2973=VECTOR('',#10631,1.);
#2974=VECTOR('',#10642,0.425);
#2975=VECTOR('',#10647,1.);
#2976=VECTOR('',#10648,1.);
#2977=VECTOR('',#10649,1.);
#2978=VECTOR('',#10650,1.);
#2979=VECTOR('',#10653,1.);
#2980=VECTOR('',#10654,1.);
#2981=VECTOR('',#10655,1.);
#2982=VECTOR('',#10658,1.);
#2983=VECTOR('',#10659,1.);
#2984=VECTOR('',#10660,1.);
#2985=VECTOR('',#10663,1.);
#2986=VECTOR('',#10664,1.);
#2987=VECTOR('',#10673,0.425);
#2988=VECTOR('',#10678,1.);
#2989=VECTOR('',#10679,1.);
#2990=VECTOR('',#10680,1.);
#2991=VECTOR('',#10681,1.);
#2992=VECTOR('',#10684,1.);
#2993=VECTOR('',#10685,1.);
#2994=VECTOR('',#10686,1.);
#2995=VECTOR('',#10689,1.);
#2996=VECTOR('',#10690,1.);
#2997=VECTOR('',#10691,1.);
#2998=VECTOR('',#10694,1.);
#2999=VECTOR('',#10695,1.);
#3000=VECTOR('',#10704,1.);
#3001=VECTOR('',#10705,1.);
#3002=VECTOR('',#10706,1.);
#3003=VECTOR('',#10707,1.);
#3004=VECTOR('',#10710,1.);
#3005=VECTOR('',#10711,1.);
#3006=VECTOR('',#10712,1.);
#3007=VECTOR('',#10713,1.);
#3008=VECTOR('',#10734,1.);
#3009=VECTOR('',#10735,1.);
#3010=VECTOR('',#10736,1.);
#3011=VECTOR('',#10737,1.);
#3012=VECTOR('',#10740,1.);
#3013=VECTOR('',#10741,1.);
#3014=VECTOR('',#10742,1.);
#3015=VECTOR('',#10743,1.);
#3016=VECTOR('',#10764,1.);
#3017=VECTOR('',#10767,1.);
#3018=VECTOR('',#10770,1.);
#3019=VECTOR('',#10773,1.);
#3020=VECTOR('',#10778,1.);
#3021=VECTOR('',#10779,1.);
#3022=VECTOR('',#10780,1.);
#3023=VECTOR('',#10783,1.);
#3024=VECTOR('',#10786,1.);
#3025=VECTOR('',#10789,1.);
#3026=VECTOR('',#10790,1.);
#3027=VECTOR('',#10793,1.);
#3028=VECTOR('',#10794,1.);
#3029=VECTOR('',#10795,1.);
#3030=VECTOR('',#10796,1.);
#3031=VECTOR('',#10801,1.21);
#3032=VECTOR('',#10806,1.);
#3033=VECTOR('',#10809,1.);
#3034=VECTOR('',#10814,1.);
#3035=VECTOR('',#10815,1.);
#3036=VECTOR('',#10818,1.);
#3037=VECTOR('',#10819,1.);
#3038=VECTOR('',#10820,1.);
#3039=VECTOR('',#10821,1.);
#3040=VECTOR('',#10824,1.);
#3041=VECTOR('',#10825,1.);
#3042=VECTOR('',#10828,1.);
#3043=VECTOR('',#10829,1.);
#3044=VECTOR('',#10832,1.);
#3045=VECTOR('',#10835,1.);
#3046=VECTOR('',#10838,1.);
#3047=VECTOR('',#10839,1.);
#3048=VECTOR('',#10850,0.425);
#3049=VECTOR('',#10855,1.);
#3050=VECTOR('',#10856,1.);
#3051=VECTOR('',#10857,1.);
#3052=VECTOR('',#10858,1.);
#3053=VECTOR('',#10861,1.);
#3054=VECTOR('',#10862,1.);
#3055=VECTOR('',#10863,1.);
#3056=VECTOR('',#10866,1.);
#3057=VECTOR('',#10867,1.);
#3058=VECTOR('',#10868,1.);
#3059=VECTOR('',#10871,1.);
#3060=VECTOR('',#10872,1.);
#3061=VECTOR('',#10881,0.425);
#3062=VECTOR('',#10886,1.);
#3063=VECTOR('',#10887,1.);
#3064=VECTOR('',#10888,1.);
#3065=VECTOR('',#10889,1.);
#3066=VECTOR('',#10892,1.);
#3067=VECTOR('',#10893,1.);
#3068=VECTOR('',#10894,1.);
#3069=VECTOR('',#10897,1.);
#3070=VECTOR('',#10898,1.);
#3071=VECTOR('',#10899,1.);
#3072=VECTOR('',#10902,1.);
#3073=VECTOR('',#10903,1.);
#3074=VECTOR('',#10912,1.);
#3075=VECTOR('',#10915,1.);
#3076=VECTOR('',#10920,1.);
#3077=VECTOR('',#10923,1.);
#3078=VECTOR('',#10926,1.);
#3079=VECTOR('',#10927,1.);
#3080=VECTOR('',#10930,1.);
#3081=VECTOR('',#10931,1.);
#3082=VECTOR('',#10942,0.425);
#3083=VECTOR('',#10947,1.);
#3084=VECTOR('',#10948,1.);
#3085=VECTOR('',#10949,1.);
#3086=VECTOR('',#10950,1.);
#3087=VECTOR('',#10953,1.);
#3088=VECTOR('',#10954,1.);
#3089=VECTOR('',#10955,1.);
#3090=VECTOR('',#10958,1.);
#3091=VECTOR('',#10959,1.);
#3092=VECTOR('',#10960,1.);
#3093=VECTOR('',#10963,1.);
#3094=VECTOR('',#10964,1.);
#3095=VECTOR('',#10973,0.425);
#3096=VECTOR('',#10978,1.);
#3097=VECTOR('',#10979,1.);
#3098=VECTOR('',#10980,1.);
#3099=VECTOR('',#10981,1.);
#3100=VECTOR('',#10984,1.);
#3101=VECTOR('',#10985,1.);
#3102=VECTOR('',#10986,1.);
#3103=VECTOR('',#10989,1.);
#3104=VECTOR('',#10990,1.);
#3105=VECTOR('',#10991,1.);
#3106=VECTOR('',#10994,1.);
#3107=VECTOR('',#10995,1.);
#3108=VECTOR('',#11004,1.);
#3109=VECTOR('',#11005,1.);
#3110=VECTOR('',#11006,1.);
#3111=VECTOR('',#11007,1.);
#3112=VECTOR('',#11010,1.);
#3113=VECTOR('',#11011,1.);
#3114=VECTOR('',#11012,1.);
#3115=VECTOR('',#11013,1.);
#3116=VECTOR('',#11034,1.);
#3117=VECTOR('',#11035,1.);
#3118=VECTOR('',#11036,1.);
#3119=VECTOR('',#11037,1.);
#3120=VECTOR('',#11040,1.);
#3121=VECTOR('',#11041,1.);
#3122=VECTOR('',#11042,1.);
#3123=VECTOR('',#11043,1.);
#3124=VECTOR('',#11064,1.);
#3125=VECTOR('',#11065,1.);
#3126=VECTOR('',#11066,1.);
#3127=VECTOR('',#11067,1.);
#3128=VECTOR('',#11070,1.);
#3129=VECTOR('',#11071,1.);
#3130=VECTOR('',#11072,1.);
#3131=VECTOR('',#11075,1.);
#3132=VECTOR('',#11076,1.);
#3133=VECTOR('',#11077,1.);
#3134=VECTOR('',#11080,1.);
#3135=VECTOR('',#11081,1.);
#3136=VECTOR('',#11090,1.);
#3137=VECTOR('',#11091,1.);
#3138=VECTOR('',#11092,1.);
#3139=VECTOR('',#11093,1.);
#3140=VECTOR('',#11096,1.);
#3141=VECTOR('',#11097,1.);
#3142=VECTOR('',#11098,1.);
#3143=VECTOR('',#11101,1.);
#3144=VECTOR('',#11102,1.);
#3145=VECTOR('',#11103,1.);
#3146=VECTOR('',#11106,1.);
#3147=VECTOR('',#11107,1.);
#3148=VECTOR('',#11116,1.);
#3149=VECTOR('',#11117,1.);
#3150=VECTOR('',#11118,1.);
#3151=VECTOR('',#11119,1.);
#3152=VECTOR('',#11122,1.);
#3153=VECTOR('',#11123,1.);
#3154=VECTOR('',#11124,1.);
#3155=VECTOR('',#11127,1.);
#3156=VECTOR('',#11128,1.);
#3157=VECTOR('',#11129,1.);
#3158=VECTOR('',#11132,1.);
#3159=VECTOR('',#11133,1.);
#3160=VECTOR('',#11134,1.);
#3161=VECTOR('',#11137,1.);
#3162=VECTOR('',#11138,1.);
#3163=VECTOR('',#11139,1.);
#3164=VECTOR('',#11142,1.);
#3165=VECTOR('',#11143,1.);
#3166=VECTOR('',#11160,0.475);
#3167=VECTOR('',#11165,0.5);
#3168=VECTOR('',#11170,0.485);
#3169=VECTOR('',#11179,0.31);
#3170=VECTOR('',#11182,0.3);
#3171=VECTOR('',#11187,1.);
#3172=VECTOR('',#11188,1.);
#3173=VECTOR('',#11189,1.);
#3174=VECTOR('',#11190,1.);
#3175=VECTOR('',#11193,1.);
#3176=VECTOR('',#11194,1.);
#3177=VECTOR('',#11195,1.);
#3178=VECTOR('',#11198,1.);
#3179=VECTOR('',#11199,1.);
#3180=VECTOR('',#11200,1.);
#3181=VECTOR('',#11203,1.);
#3182=VECTOR('',#11204,1.);
#3183=VECTOR('',#11205,1.);
#3184=VECTOR('',#11208,1.);
#3185=VECTOR('',#11209,1.);
#3186=VECTOR('',#11210,1.);
#3187=VECTOR('',#11213,1.);
#3188=VECTOR('',#11214,1.);
#3189=VECTOR('',#11227,0.4);
#3190=VECTOR('',#11240,0.625);
#3191=VECTOR('',#11245,0.65);
#3192=VECTOR('',#11250,0.635);
#3193=VECTOR('',#11259,0.41);
#3194=VECTOR('',#11262,0.4);
#3195=VECTOR('',#11269,0.42);
#3196=VECTOR('',#11276,0.8);
#3197=VECTOR('',#11287,0.734027674973257);
#3198=VECTOR('',#11294,0.734027674973257);
#3199=VECTOR('',#11297,1.);
#3200=VECTOR('',#11298,1.);
#3201=VECTOR('',#11301,1.);
#3202=VECTOR('',#11304,1.);
#3203=VECTOR('',#11309,0.4);
#3204=VECTOR('',#11314,1.);
#3205=VECTOR('',#11317,1.);
#3206=VECTOR('',#11398,1.05);
#3207=VECTOR('',#11403,1.05);
#3208=VECTOR('',#11406,1.05);
#3209=VECTOR('',#11409,1.05);
#3210=VECTOR('',#11414,1.21745);
#3211=VECTOR('',#11419,1.21745);
#3212=VECTOR('',#11422,1.21745);
#3213=VECTOR('',#11425,1.21745);
#3214=VECTOR('',#11432,1.);
#3215=VECTOR('',#11433,1.);
#3216=VECTOR('',#11434,1.);
#3217=VECTOR('',#11435,1.);
#3218=VECTOR('',#11436,1.);
#3219=VECTOR('',#11437,1.);
#3220=VECTOR('',#11442,1.);
#3221=VECTOR('',#11443,1.);
#3222=VECTOR('',#11444,1.);
#3223=VECTOR('',#11447,1.);
#3224=VECTOR('',#11448,1.);
#3225=VECTOR('',#11451,1.);
#3226=VECTOR('',#11452,1.);
#3227=VECTOR('',#11455,1.);
#3228=VECTOR('',#11456,1.);
#3229=VECTOR('',#11459,1.);
#3230=VECTOR('',#11460,1.);
#3231=VECTOR('',#11463,1.);
#3232=VECTOR('',#11474,1.05);
#3233=VECTOR('',#11479,1.05);
#3234=VECTOR('',#11482,1.05);
#3235=VECTOR('',#11485,1.05);
#3236=VECTOR('',#11490,1.21745);
#3237=VECTOR('',#11495,1.21745);
#3238=VECTOR('',#11498,1.21745);
#3239=VECTOR('',#11501,1.21745);
#3240=VECTOR('',#11508,1.);
#3241=VECTOR('',#11509,1.);
#3242=VECTOR('',#11510,1.);
#3243=VECTOR('',#11511,1.);
#3244=VECTOR('',#11512,1.);
#3245=VECTOR('',#11513,1.);
#3246=VECTOR('',#11518,1.);
#3247=VECTOR('',#11519,1.);
#3248=VECTOR('',#11520,1.);
#3249=VECTOR('',#11523,1.);
#3250=VECTOR('',#11524,1.);
#3251=VECTOR('',#11527,1.);
#3252=VECTOR('',#11528,1.);
#3253=VECTOR('',#11531,1.);
#3254=VECTOR('',#11532,1.);
#3255=VECTOR('',#11535,1.);
#3256=VECTOR('',#11536,1.);
#3257=VECTOR('',#11539,1.);
#3258=VECTOR('',#11550,1.05);
#3259=VECTOR('',#11555,1.05);
#3260=VECTOR('',#11558,1.05);
#3261=VECTOR('',#11561,1.05);
#3262=VECTOR('',#11566,1.21745);
#3263=VECTOR('',#11571,1.21745);
#3264=VECTOR('',#11574,1.21745);
#3265=VECTOR('',#11577,1.21745);
#3266=VECTOR('',#11584,1.);
#3267=VECTOR('',#11585,1.);
#3268=VECTOR('',#11586,1.);
#3269=VECTOR('',#11587,1.);
#3270=VECTOR('',#11588,1.);
#3271=VECTOR('',#11589,1.);
#3272=VECTOR('',#11594,1.);
#3273=VECTOR('',#11595,1.);
#3274=VECTOR('',#11596,1.);
#3275=VECTOR('',#11599,1.);
#3276=VECTOR('',#11600,1.);
#3277=VECTOR('',#11603,1.);
#3278=VECTOR('',#11604,1.);
#3279=VECTOR('',#11607,1.);
#3280=VECTOR('',#11608,1.);
#3281=VECTOR('',#11611,1.);
#3282=VECTOR('',#11612,1.);
#3283=VECTOR('',#11615,1.);
#3284=VECTOR('',#11626,1.05);
#3285=VECTOR('',#11631,1.05);
#3286=VECTOR('',#11634,1.05);
#3287=VECTOR('',#11637,1.05);
#3288=VECTOR('',#11642,1.21745);
#3289=VECTOR('',#11647,1.21745);
#3290=VECTOR('',#11650,1.21745);
#3291=VECTOR('',#11653,1.21745);
#3292=VECTOR('',#11660,1.);
#3293=VECTOR('',#11661,1.);
#3294=VECTOR('',#11662,1.);
#3295=VECTOR('',#11663,1.);
#3296=VECTOR('',#11664,1.);
#3297=VECTOR('',#11665,1.);
#3298=VECTOR('',#11670,1.);
#3299=VECTOR('',#11671,1.);
#3300=VECTOR('',#11672,1.);
#3301=VECTOR('',#11675,1.);
#3302=VECTOR('',#11676,1.);
#3303=VECTOR('',#11679,1.);
#3304=VECTOR('',#11680,1.);
#3305=VECTOR('',#11683,1.);
#3306=VECTOR('',#11684,1.);
#3307=VECTOR('',#11687,1.);
#3308=VECTOR('',#11688,1.);
#3309=VECTOR('',#11691,1.);
#3310=CIRCLE('',#9047,0.15);
#3311=CIRCLE('',#9048,0.15);
#3312=CIRCLE('',#9051,0.15);
#3313=CIRCLE('',#9052,0.15);
#3314=CIRCLE('',#9055,0.25);
#3315=CIRCLE('',#9056,0.25);
#3316=CIRCLE('',#9058,0.25);
#3317=CIRCLE('',#9059,0.25);
#3318=CIRCLE('',#9061,0.25);
#3319=CIRCLE('',#9062,0.25);
#3320=CIRCLE('',#9064,0.25);
#3321=CIRCLE('',#9065,0.25);
#3322=CIRCLE('',#9074,1.188225);
#3323=CIRCLE('',#9169,1.016475);
#3324=CIRCLE('',#9264,0.15);
#3325=CIRCLE('',#9265,0.15);
#3326=CIRCLE('',#9267,0.15);
#3327=CIRCLE('',#9268,0.15);
#3328=CIRCLE('',#9270,0.33);
#3329=CIRCLE('',#9271,0.33);
#3330=CIRCLE('',#9273,0.33);
#3331=CIRCLE('',#9274,0.33);
#3332=CIRCLE('',#9276,0.33);
#3333=CIRCLE('',#9277,0.33);
#3334=CIRCLE('',#9279,0.33);
#3335=CIRCLE('',#9280,0.33);
#3336=CIRCLE('',#9282,3.8);
#3337=CIRCLE('',#9283,1.016475);
#3338=CIRCLE('',#9285,3.8);
#3339=CIRCLE('',#9289,1.188225);
#3340=CIRCLE('',#9293,0.15);
#3341=CIRCLE('',#9294,0.15);
#3342=CIRCLE('',#9299,0.15);
#3343=CIRCLE('',#9300,0.15);
#3344=CIRCLE('',#9305,1.1);
#3345=CIRCLE('',#9306,1.1);
#3346=CIRCLE('',#9308,2.);
#3347=CIRCLE('',#9309,2.);
#3348=CIRCLE('',#9312,1.21);
#3349=CIRCLE('',#9313,1.21);
#3350=CIRCLE('',#9315,2.);
#3351=CIRCLE('',#9316,2.);
#3352=CIRCLE('',#9325,2.);
#3353=CIRCLE('',#9326,2.);
#3354=CIRCLE('',#9331,0.425);
#3355=CIRCLE('',#9332,0.425);
#3356=CIRCLE('',#9340,0.425);
#3357=CIRCLE('',#9341,0.425);
#3358=CIRCLE('',#9350,1.1);
#3359=CIRCLE('',#9351,1.1);
#3360=CIRCLE('',#9353,2.);
#3361=CIRCLE('',#9357,2.);
#3362=CIRCLE('',#9360,0.425);
#3363=CIRCLE('',#9361,0.425);
#3364=CIRCLE('',#9369,0.425);
#3365=CIRCLE('',#9370,0.425);
#3366=CIRCLE('',#9381,1.1);
#3367=CIRCLE('',#9382,1.);
#3368=CIRCLE('',#9384,1.);
#3369=CIRCLE('',#9386,1.1);
#3370=CIRCLE('',#9392,1.1);
#3371=CIRCLE('',#9393,1.);
#3372=CIRCLE('',#9395,1.);
#3373=CIRCLE('',#9397,1.1);
#3374=CIRCLE('',#9401,3.1);
#3375=CIRCLE('',#9402,3.1);
#3376=CIRCLE('',#9403,3.1);
#3377=CIRCLE('',#9404,3.1);
#3378=CIRCLE('',#9407,4.2);
#3379=CIRCLE('',#9411,1.21);
#3380=CIRCLE('',#9412,1.21);
#3381=CIRCLE('',#9414,2.);
#3382=CIRCLE('',#9415,2.);
#3383=CIRCLE('',#9424,4.2);
#3384=CIRCLE('',#9427,0.425);
#3385=CIRCLE('',#9428,0.425);
#3386=CIRCLE('',#9436,0.425);
#3387=CIRCLE('',#9437,0.425);
#3388=CIRCLE('',#9446,3.1);
#3389=CIRCLE('',#9447,3.1);
#3390=CIRCLE('',#9449,4.2);
#3391=CIRCLE('',#9453,4.2);
#3392=CIRCLE('',#9456,0.425);
#3393=CIRCLE('',#9457,0.425);
#3394=CIRCLE('',#9465,0.425);
#3395=CIRCLE('',#9466,0.425);
#3396=CIRCLE('',#9477,3.1);
#3397=CIRCLE('',#9478,3.);
#3398=CIRCLE('',#9480,3.);
#3399=CIRCLE('',#9482,3.1);
#3400=CIRCLE('',#9488,3.1);
#3401=CIRCLE('',#9489,3.);
#3402=CIRCLE('',#9491,3.);
#3403=CIRCLE('',#9493,3.1);
#3404=CIRCLE('',#9519,0.2942);
#3405=CIRCLE('',#9521,0.45);
#3406=CIRCLE('',#9523,0.5);
#3407=CIRCLE('',#9525,0.5);
#3408=CIRCLE('',#9527,0.47);
#3409=CIRCLE('',#9529,0.32);
#3410=CIRCLE('',#9531,0.2942);
#3411=CIRCLE('',#9543,0.4);
#3412=CIRCLE('',#9544,0.3933);
#3413=CIRCLE('',#9546,0.4);
#3414=CIRCLE('',#9549,0.6);
#3415=CIRCLE('',#9551,0.65);
#3416=CIRCLE('',#9553,0.65);
#3417=CIRCLE('',#9555,0.62);
#3418=CIRCLE('',#9557,0.42);
#3419=CIRCLE('',#9559,0.3933);
#3420=CIRCLE('',#9563,0.42);
#3421=CIRCLE('',#9564,0.42);
#3422=CIRCLE('',#9566,0.8);
#3423=CIRCLE('',#9567,0.8);
#3424=CIRCLE('',#9572,0.6175);
#3425=CIRCLE('',#9574,0.6175);
#3426=CIRCLE('',#9579,0.338975);
#3427=CIRCLE('',#9580,0.338975);
#3428=CIRCLE('',#9623,1.0501);
#3429=CIRCLE('',#9627,1.0501);
#3430=CIRCLE('',#9629,1.21745);
#3431=CIRCLE('',#9633,1.21745);
#3432=CIRCLE('',#9648,1.0501);
#3433=CIRCLE('',#9652,1.0501);
#3434=CIRCLE('',#9654,1.21745);
#3435=CIRCLE('',#9658,1.21745);
#3436=CIRCLE('',#9673,1.0501);
#3437=CIRCLE('',#9677,1.0501);
#3438=CIRCLE('',#9679,1.21745);
#3439=CIRCLE('',#9683,1.21745);
#3440=CIRCLE('',#9698,1.0501);
#3441=CIRCLE('',#9702,1.0501);
#3442=CIRCLE('',#9704,1.21745);
#3443=CIRCLE('',#9708,1.21745);
#3444=VERTEX_POINT('',#11710);
#3445=VERTEX_POINT('',#11712);
#3446=VERTEX_POINT('',#11717);
#3447=VERTEX_POINT('',#11719);
#3448=VERTEX_POINT('',#11724);
#3449=VERTEX_POINT('',#11726);
#3450=VERTEX_POINT('',#11730);
#3451=VERTEX_POINT('',#11732);
#3452=VERTEX_POINT('',#11736);
#3453=VERTEX_POINT('',#11738);
#3454=VERTEX_POINT('',#11742);
#3455=VERTEX_POINT('',#11744);
#3456=VERTEX_POINT('',#11748);
#3457=VERTEX_POINT('',#11749);
#3458=VERTEX_POINT('',#11751);
#3459=VERTEX_POINT('',#11753);
#3460=VERTEX_POINT('',#11757);
#3461=VERTEX_POINT('',#11759);
#3462=VERTEX_POINT('',#11763);
#3463=VERTEX_POINT('',#11765);
#3464=VERTEX_POINT('',#11775);
#3465=VERTEX_POINT('',#11776);
#3466=VERTEX_POINT('',#11778);
#3467=VERTEX_POINT('',#11789);
#3468=VERTEX_POINT('',#11802);
#3469=VERTEX_POINT('',#11803);
#3470=VERTEX_POINT('',#11856);
#3471=VERTEX_POINT('',#11857);
#3472=VERTEX_POINT('',#11916);
#3473=VERTEX_POINT('',#11917);
#3474=VERTEX_POINT('',#11973);
#3475=VERTEX_POINT('',#11974);
#3476=VERTEX_POINT('',#12033);
#3477=VERTEX_POINT('',#12034);
#3478=VERTEX_POINT('',#12093);
#3479=VERTEX_POINT('',#12094);
#3480=VERTEX_POINT('',#12150);
#3481=VERTEX_POINT('',#12151);
#3482=VERTEX_POINT('',#12210);
#3483=VERTEX_POINT('',#12211);
#3484=VERTEX_POINT('',#12270);
#3485=VERTEX_POINT('',#12271);
#3486=VERTEX_POINT('',#12330);
#3487=VERTEX_POINT('',#12331);
#3488=VERTEX_POINT('',#12390);
#3489=VERTEX_POINT('',#12391);
#3490=VERTEX_POINT('',#12450);
#3491=VERTEX_POINT('',#12451);
#3492=VERTEX_POINT('',#12507);
#3493=VERTEX_POINT('',#12508);
#3494=VERTEX_POINT('',#12567);
#3495=VERTEX_POINT('',#12568);
#3496=VERTEX_POINT('',#12627);
#3497=VERTEX_POINT('',#12628);
#3498=VERTEX_POINT('',#12687);
#3499=VERTEX_POINT('',#12688);
#3500=VERTEX_POINT('',#12747);
#3501=VERTEX_POINT('',#12748);
#3502=VERTEX_POINT('',#12804);
#3503=VERTEX_POINT('',#12805);
#3504=VERTEX_POINT('',#12864);
#3505=VERTEX_POINT('',#12865);
#3506=VERTEX_POINT('',#12924);
#3507=VERTEX_POINT('',#12925);
#3508=VERTEX_POINT('',#12984);
#3509=VERTEX_POINT('',#12985);
#3510=VERTEX_POINT('',#13044);
#3511=VERTEX_POINT('',#13045);
#3512=VERTEX_POINT('',#13098);
#3513=VERTEX_POINT('',#13099);
#3514=VERTEX_POINT('',#13158);
#3515=VERTEX_POINT('',#13159);
#3516=VERTEX_POINT('',#13218);
#3517=VERTEX_POINT('',#13219);
#3518=VERTEX_POINT('',#13278);
#3519=VERTEX_POINT('',#13279);
#3520=VERTEX_POINT('',#13335);
#3521=VERTEX_POINT('',#13336);
#3522=VERTEX_POINT('',#13395);
#3523=VERTEX_POINT('',#13396);
#3524=VERTEX_POINT('',#13455);
#3525=VERTEX_POINT('',#13456);
#3526=VERTEX_POINT('',#13515);
#3527=VERTEX_POINT('',#13516);
#3528=VERTEX_POINT('',#13575);
#3529=VERTEX_POINT('',#13576);
#3530=VERTEX_POINT('',#13635);
#3531=VERTEX_POINT('',#13636);
#3532=VERTEX_POINT('',#13695);
#3533=VERTEX_POINT('',#13696);
#3534=VERTEX_POINT('',#13755);
#3535=VERTEX_POINT('',#13756);
#3536=VERTEX_POINT('',#13815);
#3537=VERTEX_POINT('',#13816);
#3538=VERTEX_POINT('',#13875);
#3539=VERTEX_POINT('',#13876);
#3540=VERTEX_POINT('',#13932);
#3541=VERTEX_POINT('',#13933);
#3542=VERTEX_POINT('',#13992);
#3543=VERTEX_POINT('',#13993);
#3544=VERTEX_POINT('',#14052);
#3545=VERTEX_POINT('',#14053);
#3546=VERTEX_POINT('',#14112);
#3547=VERTEX_POINT('',#14113);
#3548=VERTEX_POINT('',#14172);
#3549=VERTEX_POINT('',#14173);
#3550=VERTEX_POINT('',#14229);
#3551=VERTEX_POINT('',#14230);
#3552=VERTEX_POINT('',#14289);
#3553=VERTEX_POINT('',#14290);
#3554=VERTEX_POINT('',#14349);
#3555=VERTEX_POINT('',#14350);
#3556=VERTEX_POINT('',#14409);
#3557=VERTEX_POINT('',#14410);
#3558=VERTEX_POINT('',#14469);
#3559=VERTEX_POINT('',#14470);
#3560=VERTEX_POINT('',#14529);
#3561=VERTEX_POINT('',#14530);
#3562=VERTEX_POINT('',#14589);
#3563=VERTEX_POINT('',#14590);
#3564=VERTEX_POINT('',#14646);
#3565=VERTEX_POINT('',#14647);
#3566=VERTEX_POINT('',#14706);
#3567=VERTEX_POINT('',#14707);
#3568=VERTEX_POINT('',#14766);
#3569=VERTEX_POINT('',#14767);
#3570=VERTEX_POINT('',#14826);
#3571=VERTEX_POINT('',#14827);
#3572=VERTEX_POINT('',#14886);
#3573=VERTEX_POINT('',#14887);
#3574=VERTEX_POINT('',#14943);
#3575=VERTEX_POINT('',#14944);
#3576=VERTEX_POINT('',#15003);
#3577=VERTEX_POINT('',#15004);
#3578=VERTEX_POINT('',#15063);
#3579=VERTEX_POINT('',#15064);
#3580=VERTEX_POINT('',#15123);
#3581=VERTEX_POINT('',#15124);
#3582=VERTEX_POINT('',#15183);
#3583=VERTEX_POINT('',#15184);
#3584=VERTEX_POINT('',#15243);
#3585=VERTEX_POINT('',#15244);
#3586=VERTEX_POINT('',#15300);
#3587=VERTEX_POINT('',#15301);
#3588=VERTEX_POINT('',#15360);
#3589=VERTEX_POINT('',#15361);
#3590=VERTEX_POINT('',#15420);
#3591=VERTEX_POINT('',#15421);
#3592=VERTEX_POINT('',#15480);
#3593=VERTEX_POINT('',#15481);
#3594=VERTEX_POINT('',#15540);
#3595=VERTEX_POINT('',#15541);
#3596=VERTEX_POINT('',#15597);
#3597=VERTEX_POINT('',#15598);
#3598=VERTEX_POINT('',#15657);
#3599=VERTEX_POINT('',#15658);
#3600=VERTEX_POINT('',#15717);
#3601=VERTEX_POINT('',#15718);
#3602=VERTEX_POINT('',#15777);
#3603=VERTEX_POINT('',#15778);
#3604=VERTEX_POINT('',#15834);
#3605=VERTEX_POINT('',#15835);
#3606=VERTEX_POINT('',#15894);
#3607=VERTEX_POINT('',#15895);
#3608=VERTEX_POINT('',#15954);
#3609=VERTEX_POINT('',#15955);
#3610=VERTEX_POINT('',#16014);
#3611=VERTEX_POINT('',#16015);
#3612=VERTEX_POINT('',#16074);
#3613=VERTEX_POINT('',#16075);
#3614=VERTEX_POINT('',#16134);
#3615=VERTEX_POINT('',#16135);
#3616=VERTEX_POINT('',#16194);
#3617=VERTEX_POINT('',#16195);
#3618=VERTEX_POINT('',#16254);
#3619=VERTEX_POINT('',#16255);
#3620=VERTEX_POINT('',#16314);
#3621=VERTEX_POINT('',#16315);
#3622=VERTEX_POINT('',#16374);
#3623=VERTEX_POINT('',#16375);
#3624=VERTEX_POINT('',#16431);
#3625=VERTEX_POINT('',#16432);
#3626=VERTEX_POINT('',#16491);
#3627=VERTEX_POINT('',#16492);
#3628=VERTEX_POINT('',#16551);
#3629=VERTEX_POINT('',#16552);
#3630=VERTEX_POINT('',#16611);
#3631=VERTEX_POINT('',#16612);
#3632=VERTEX_POINT('',#16671);
#3633=VERTEX_POINT('',#16672);
#3634=VERTEX_POINT('',#16728);
#3635=VERTEX_POINT('',#16729);
#3636=VERTEX_POINT('',#16788);
#3637=VERTEX_POINT('',#16789);
#3638=VERTEX_POINT('',#16848);
#3639=VERTEX_POINT('',#16849);
#3640=VERTEX_POINT('',#16908);
#3641=VERTEX_POINT('',#16909);
#3642=VERTEX_POINT('',#16968);
#3643=VERTEX_POINT('',#16969);
#3644=VERTEX_POINT('',#17028);
#3645=VERTEX_POINT('',#17029);
#3646=VERTEX_POINT('',#17088);
#3647=VERTEX_POINT('',#17089);
#3648=VERTEX_POINT('',#17148);
#3649=VERTEX_POINT('',#17149);
#3650=VERTEX_POINT('',#17208);
#3651=VERTEX_POINT('',#17209);
#3652=VERTEX_POINT('',#17268);
#3653=VERTEX_POINT('',#17269);
#3654=VERTEX_POINT('',#17325);
#3655=VERTEX_POINT('',#17326);
#3656=VERTEX_POINT('',#17328);
#3657=VERTEX_POINT('',#17339);
#3658=VERTEX_POINT('',#17347);
#3659=VERTEX_POINT('',#17348);
#3660=VERTEX_POINT('',#17407);
#3661=VERTEX_POINT('',#17408);
#3662=VERTEX_POINT('',#17464);
#3663=VERTEX_POINT('',#17465);
#3664=VERTEX_POINT('',#17524);
#3665=VERTEX_POINT('',#17525);
#3666=VERTEX_POINT('',#17584);
#3667=VERTEX_POINT('',#17585);
#3668=VERTEX_POINT('',#17627);
#3669=VERTEX_POINT('',#17628);
#3670=VERTEX_POINT('',#17670);
#3671=VERTEX_POINT('',#17671);
#3672=VERTEX_POINT('',#17712);
#3673=VERTEX_POINT('',#17713);
#3674=VERTEX_POINT('',#17772);
#3675=VERTEX_POINT('',#17773);
#3676=VERTEX_POINT('',#17832);
#3677=VERTEX_POINT('',#17833);
#3678=VERTEX_POINT('',#17892);
#3679=VERTEX_POINT('',#17893);
#3680=VERTEX_POINT('',#17952);
#3681=VERTEX_POINT('',#17953);
#3682=VERTEX_POINT('',#17995);
#3683=VERTEX_POINT('',#17996);
#3684=VERTEX_POINT('',#18055);
#3685=VERTEX_POINT('',#18056);
#3686=VERTEX_POINT('',#18115);
#3687=VERTEX_POINT('',#18116);
#3688=VERTEX_POINT('',#18175);
#3689=VERTEX_POINT('',#18176);
#3690=VERTEX_POINT('',#18218);
#3691=VERTEX_POINT('',#18219);
#3692=VERTEX_POINT('',#18278);
#3693=VERTEX_POINT('',#18279);
#3694=VERTEX_POINT('',#18338);
#3695=VERTEX_POINT('',#18339);
#3696=VERTEX_POINT('',#18398);
#3697=VERTEX_POINT('',#18399);
#3698=VERTEX_POINT('',#18458);
#3699=VERTEX_POINT('',#18459);
#3700=VERTEX_POINT('',#18501);
#3701=VERTEX_POINT('',#18502);
#3702=VERTEX_POINT('',#18561);
#3703=VERTEX_POINT('',#18562);
#3704=VERTEX_POINT('',#18621);
#3705=VERTEX_POINT('',#18622);
#3706=VERTEX_POINT('',#18681);
#3707=VERTEX_POINT('',#18682);
#3708=VERTEX_POINT('',#18741);
#3709=VERTEX_POINT('',#18742);
#3710=VERTEX_POINT('',#18766);
#3711=VERTEX_POINT('',#18767);
#3712=VERTEX_POINT('',#18810);
#3713=VERTEX_POINT('',#18811);
#3714=VERTEX_POINT('',#18870);
#3715=VERTEX_POINT('',#18871);
#3716=VERTEX_POINT('',#18930);
#3717=VERTEX_POINT('',#18931);
#3718=VERTEX_POINT('',#18973);
#3719=VERTEX_POINT('',#18974);
#3720=VERTEX_POINT('',#19016);
#3721=VERTEX_POINT('',#19017);
#3722=VERTEX_POINT('',#19059);
#3723=VERTEX_POINT('',#19060);
#3724=VERTEX_POINT('',#19119);
#3725=VERTEX_POINT('',#19120);
#3726=VERTEX_POINT('',#19179);
#3727=VERTEX_POINT('',#19180);
#3728=VERTEX_POINT('',#19222);
#3729=VERTEX_POINT('',#19223);
#3730=VERTEX_POINT('',#19265);
#3731=VERTEX_POINT('',#19266);
#3732=VERTEX_POINT('',#19325);
#3733=VERTEX_POINT('',#19326);
#3734=VERTEX_POINT('',#19385);
#3735=VERTEX_POINT('',#19386);
#3736=VERTEX_POINT('',#19445);
#3737=VERTEX_POINT('',#19446);
#3738=VERTEX_POINT('',#19505);
#3739=VERTEX_POINT('',#19506);
#3740=VERTEX_POINT('',#19548);
#3741=VERTEX_POINT('',#19549);
#3742=VERTEX_POINT('',#19591);
#3743=VERTEX_POINT('',#19592);
#3744=VERTEX_POINT('',#19651);
#3745=VERTEX_POINT('',#19652);
#3746=VERTEX_POINT('',#19711);
#3747=VERTEX_POINT('',#19712);
#3748=VERTEX_POINT('',#19754);
#3749=VERTEX_POINT('',#19755);
#3750=VERTEX_POINT('',#19797);
#3751=VERTEX_POINT('',#19798);
#3752=VERTEX_POINT('',#19840);
#3753=VERTEX_POINT('',#19841);
#3754=VERTEX_POINT('',#19900);
#3755=VERTEX_POINT('',#19901);
#3756=VERTEX_POINT('',#19943);
#3757=VERTEX_POINT('',#19944);
#3758=VERTEX_POINT('',#20003);
#3759=VERTEX_POINT('',#20004);
#3760=VERTEX_POINT('',#20063);
#3761=VERTEX_POINT('',#20064);
#3762=VERTEX_POINT('',#20123);
#3763=VERTEX_POINT('',#20124);
#3764=VERTEX_POINT('',#20183);
#3765=VERTEX_POINT('',#20184);
#3766=VERTEX_POINT('',#20226);
#3767=VERTEX_POINT('',#20227);
#3768=VERTEX_POINT('',#20286);
#3769=VERTEX_POINT('',#20287);
#3770=VERTEX_POINT('',#20346);
#3771=VERTEX_POINT('',#20347);
#3772=VERTEX_POINT('',#20406);
#3773=VERTEX_POINT('',#20407);
#3774=VERTEX_POINT('',#20449);
#3775=VERTEX_POINT('',#20450);
#3776=VERTEX_POINT('',#20509);
#3777=VERTEX_POINT('',#20510);
#3778=VERTEX_POINT('',#20569);
#3779=VERTEX_POINT('',#20570);
#3780=VERTEX_POINT('',#20629);
#3781=VERTEX_POINT('',#20630);
#3782=VERTEX_POINT('',#20689);
#3783=VERTEX_POINT('',#20690);
#3784=VERTEX_POINT('',#20731);
#3785=VERTEX_POINT('',#20732);
#3786=VERTEX_POINT('',#20791);
#3787=VERTEX_POINT('',#20792);
#3788=VERTEX_POINT('',#20834);
#3789=VERTEX_POINT('',#20835);
#3790=VERTEX_POINT('',#20894);
#3791=VERTEX_POINT('',#20895);
#3792=VERTEX_POINT('',#20954);
#3793=VERTEX_POINT('',#20955);
#3794=VERTEX_POINT('',#20997);
#3795=VERTEX_POINT('',#20998);
#3796=VERTEX_POINT('',#21041);
#3797=VERTEX_POINT('',#21042);
#3798=VERTEX_POINT('',#21101);
#3799=VERTEX_POINT('',#21102);
#3800=VERTEX_POINT('',#21161);
#3801=VERTEX_POINT('',#21162);
#3802=VERTEX_POINT('',#21204);
#3803=VERTEX_POINT('',#21205);
#3804=VERTEX_POINT('',#21247);
#3805=VERTEX_POINT('',#21248);
#3806=VERTEX_POINT('',#21307);
#3807=VERTEX_POINT('',#21308);
#3808=VERTEX_POINT('',#21367);
#3809=VERTEX_POINT('',#21368);
#3810=VERTEX_POINT('',#21427);
#3811=VERTEX_POINT('',#21428);
#3812=VERTEX_POINT('',#21470);
#3813=VERTEX_POINT('',#21471);
#3814=VERTEX_POINT('',#21513);
#3815=VERTEX_POINT('',#21514);
#3816=VERTEX_POINT('',#21573);
#3817=VERTEX_POINT('',#21574);
#3818=VERTEX_POINT('',#21633);
#3819=VERTEX_POINT('',#21634);
#3820=VERTEX_POINT('',#21693);
#3821=VERTEX_POINT('',#21694);
#3822=VERTEX_POINT('',#21753);
#3823=VERTEX_POINT('',#21754);
#3824=VERTEX_POINT('',#21796);
#3825=VERTEX_POINT('',#21797);
#3826=VERTEX_POINT('',#21823);
#3827=VERTEX_POINT('',#21824);
#3828=VERTEX_POINT('',#21883);
#3829=VERTEX_POINT('',#21884);
#3830=VERTEX_POINT('',#21926);
#3831=VERTEX_POINT('',#21927);
#3832=VERTEX_POINT('',#21969);
#3833=VERTEX_POINT('',#21970);
#3834=VERTEX_POINT('',#22012);
#3835=VERTEX_POINT('',#22013);
#3836=VERTEX_POINT('',#22055);
#3837=VERTEX_POINT('',#22056);
#3838=VERTEX_POINT('',#22115);
#3839=VERTEX_POINT('',#22116);
#3840=VERTEX_POINT('',#22175);
#3841=VERTEX_POINT('',#22176);
#3842=VERTEX_POINT('',#22218);
#3843=VERTEX_POINT('',#22219);
#3844=VERTEX_POINT('',#22244);
#3845=VERTEX_POINT('',#22246);
#3846=VERTEX_POINT('',#22250);
#3847=VERTEX_POINT('',#22252);
#3848=VERTEX_POINT('',#22256);
#3849=VERTEX_POINT('',#22258);
#3850=VERTEX_POINT('',#22262);
#3851=VERTEX_POINT('',#22264);
#3852=VERTEX_POINT('',#22268);
#3853=VERTEX_POINT('',#22270);
#3854=VERTEX_POINT('',#22274);
#3855=VERTEX_POINT('',#22276);
#3856=VERTEX_POINT('',#22280);
#3857=VERTEX_POINT('',#22282);
#3858=VERTEX_POINT('',#22297);
#3859=VERTEX_POINT('',#22382);
#3860=VERTEX_POINT('',#25114);
#3861=VERTEX_POINT('',#27977);
#3862=VERTEX_POINT('',#28016);
#3863=VERTEX_POINT('',#28018);
#3864=VERTEX_POINT('',#28025);
#3865=VERTEX_POINT('',#28027);
#3866=VERTEX_POINT('',#28034);
#3867=VERTEX_POINT('',#28035);
#3868=VERTEX_POINT('',#28037);
#3869=VERTEX_POINT('',#28039);
#3870=VERTEX_POINT('',#28043);
#3871=VERTEX_POINT('',#28045);
#3872=VERTEX_POINT('',#28047);
#3873=VERTEX_POINT('',#28049);
#3874=VERTEX_POINT('',#28051);
#3875=VERTEX_POINT('',#28053);
#3876=VERTEX_POINT('',#28057);
#3877=VERTEX_POINT('',#28061);
#3878=VERTEX_POINT('',#28063);
#3879=VERTEX_POINT('',#28067);
#3880=VERTEX_POINT('',#28068);
#3881=VERTEX_POINT('',#28070);
#3882=VERTEX_POINT('',#28072);
#3883=VERTEX_POINT('',#28076);
#3884=VERTEX_POINT('',#28078);
#3885=VERTEX_POINT('',#28082);
#3886=VERTEX_POINT('',#28084);
#3887=VERTEX_POINT('',#28086);
#3888=VERTEX_POINT('',#28088);
#3889=VERTEX_POINT('',#28092);
#3890=VERTEX_POINT('',#28096);
#3891=VERTEX_POINT('',#28103);
#3892=VERTEX_POINT('',#28107);
#3893=VERTEX_POINT('',#28111);
#3894=VERTEX_POINT('',#28120);
#3895=VERTEX_POINT('',#28122);
#3896=VERTEX_POINT('',#28126);
#3897=VERTEX_POINT('',#28127);
#3898=VERTEX_POINT('',#28129);
#3899=VERTEX_POINT('',#28131);
#3900=VERTEX_POINT('',#28135);
#3901=VERTEX_POINT('',#28137);
#3902=VERTEX_POINT('',#28141);
#3903=VERTEX_POINT('',#28143);
#3904=VERTEX_POINT('',#28152);
#3905=VERTEX_POINT('',#28154);
#3906=VERTEX_POINT('',#28158);
#3907=VERTEX_POINT('',#28159);
#3908=VERTEX_POINT('',#28161);
#3909=VERTEX_POINT('',#28163);
#3910=VERTEX_POINT('',#28167);
#3911=VERTEX_POINT('',#28169);
#3912=VERTEX_POINT('',#28173);
#3913=VERTEX_POINT('',#28175);
#3914=VERTEX_POINT('',#28185);
#3915=VERTEX_POINT('',#28186);
#3916=VERTEX_POINT('',#28188);
#3917=VERTEX_POINT('',#28190);
#3918=VERTEX_POINT('',#28194);
#3919=VERTEX_POINT('',#28196);
#3920=VERTEX_POINT('',#28200);
#3921=VERTEX_POINT('',#28204);
#3922=VERTEX_POINT('',#28211);
#3923=VERTEX_POINT('',#28213);
#3924=VERTEX_POINT('',#28217);
#3925=VERTEX_POINT('',#28218);
#3926=VERTEX_POINT('',#28220);
#3927=VERTEX_POINT('',#28222);
#3928=VERTEX_POINT('',#28226);
#3929=VERTEX_POINT('',#28228);
#3930=VERTEX_POINT('',#28232);
#3931=VERTEX_POINT('',#28234);
#3932=VERTEX_POINT('',#28243);
#3933=VERTEX_POINT('',#28245);
#3934=VERTEX_POINT('',#28249);
#3935=VERTEX_POINT('',#28250);
#3936=VERTEX_POINT('',#28252);
#3937=VERTEX_POINT('',#28254);
#3938=VERTEX_POINT('',#28258);
#3939=VERTEX_POINT('',#28260);
#3940=VERTEX_POINT('',#28264);
#3941=VERTEX_POINT('',#28266);
#3942=VERTEX_POINT('',#28276);
#3943=VERTEX_POINT('',#28277);
#3944=VERTEX_POINT('',#28279);
#3945=VERTEX_POINT('',#28281);
#3946=VERTEX_POINT('',#28285);
#3947=VERTEX_POINT('',#28286);
#3948=VERTEX_POINT('',#28288);
#3949=VERTEX_POINT('',#28290);
#3950=VERTEX_POINT('',#28303);
#3951=VERTEX_POINT('',#28304);
#3952=VERTEX_POINT('',#28306);
#3953=VERTEX_POINT('',#28308);
#3954=VERTEX_POINT('',#28312);
#3955=VERTEX_POINT('',#28313);
#3956=VERTEX_POINT('',#28315);
#3957=VERTEX_POINT('',#28317);
#3958=VERTEX_POINT('',#28330);
#3959=VERTEX_POINT('',#28331);
#3960=VERTEX_POINT('',#28333);
#3961=VERTEX_POINT('',#28335);
#3962=VERTEX_POINT('',#28337);
#3963=VERTEX_POINT('',#28339);
#3964=VERTEX_POINT('',#28341);
#3965=VERTEX_POINT('',#28343);
#3966=VERTEX_POINT('',#28347);
#3967=VERTEX_POINT('',#28349);
#3968=VERTEX_POINT('',#28353);
#3969=VERTEX_POINT('',#28355);
#3970=VERTEX_POINT('',#28359);
#3971=VERTEX_POINT('',#28363);
#3972=VERTEX_POINT('',#28365);
#3973=VERTEX_POINT('',#28367);
#3974=VERTEX_POINT('',#28371);
#3975=VERTEX_POINT('',#28373);
#3976=VERTEX_POINT('',#28377);
#3977=VERTEX_POINT('',#28378);
#3978=VERTEX_POINT('',#28380);
#3979=VERTEX_POINT('',#28382);
#3980=VERTEX_POINT('',#28389);
#3981=VERTEX_POINT('',#28391);
#3982=VERTEX_POINT('',#28393);
#3983=VERTEX_POINT('',#28397);
#3984=VERTEX_POINT('',#28401);
#3985=VERTEX_POINT('',#28409);
#3986=VERTEX_POINT('',#28416);
#3987=VERTEX_POINT('',#28418);
#3988=VERTEX_POINT('',#28422);
#3989=VERTEX_POINT('',#28423);
#3990=VERTEX_POINT('',#28425);
#3991=VERTEX_POINT('',#28427);
#3992=VERTEX_POINT('',#28431);
#3993=VERTEX_POINT('',#28433);
#3994=VERTEX_POINT('',#28437);
#3995=VERTEX_POINT('',#28439);
#3996=VERTEX_POINT('',#28448);
#3997=VERTEX_POINT('',#28450);
#3998=VERTEX_POINT('',#28454);
#3999=VERTEX_POINT('',#28455);
#4000=VERTEX_POINT('',#28457);
#4001=VERTEX_POINT('',#28459);
#4002=VERTEX_POINT('',#28463);
#4003=VERTEX_POINT('',#28465);
#4004=VERTEX_POINT('',#28469);
#4005=VERTEX_POINT('',#28471);
#4006=VERTEX_POINT('',#28481);
#4007=VERTEX_POINT('',#28482);
#4008=VERTEX_POINT('',#28484);
#4009=VERTEX_POINT('',#28486);
#4010=VERTEX_POINT('',#28490);
#4011=VERTEX_POINT('',#28492);
#4012=VERTEX_POINT('',#28496);
#4013=VERTEX_POINT('',#28500);
#4014=VERTEX_POINT('',#28507);
#4015=VERTEX_POINT('',#28509);
#4016=VERTEX_POINT('',#28513);
#4017=VERTEX_POINT('',#28514);
#4018=VERTEX_POINT('',#28516);
#4019=VERTEX_POINT('',#28518);
#4020=VERTEX_POINT('',#28522);
#4021=VERTEX_POINT('',#28524);
#4022=VERTEX_POINT('',#28528);
#4023=VERTEX_POINT('',#28530);
#4024=VERTEX_POINT('',#28539);
#4025=VERTEX_POINT('',#28541);
#4026=VERTEX_POINT('',#28545);
#4027=VERTEX_POINT('',#28546);
#4028=VERTEX_POINT('',#28548);
#4029=VERTEX_POINT('',#28550);
#4030=VERTEX_POINT('',#28554);
#4031=VERTEX_POINT('',#28556);
#4032=VERTEX_POINT('',#28560);
#4033=VERTEX_POINT('',#28562);
#4034=VERTEX_POINT('',#28572);
#4035=VERTEX_POINT('',#28573);
#4036=VERTEX_POINT('',#28575);
#4037=VERTEX_POINT('',#28577);
#4038=VERTEX_POINT('',#28581);
#4039=VERTEX_POINT('',#28582);
#4040=VERTEX_POINT('',#28584);
#4041=VERTEX_POINT('',#28586);
#4042=VERTEX_POINT('',#28599);
#4043=VERTEX_POINT('',#28600);
#4044=VERTEX_POINT('',#28602);
#4045=VERTEX_POINT('',#28604);
#4046=VERTEX_POINT('',#28608);
#4047=VERTEX_POINT('',#28609);
#4048=VERTEX_POINT('',#28611);
#4049=VERTEX_POINT('',#28613);
#4050=VERTEX_POINT('',#28626);
#4051=VERTEX_POINT('',#28627);
#4052=VERTEX_POINT('',#28629);
#4053=VERTEX_POINT('',#28631);
#4054=VERTEX_POINT('',#28635);
#4055=VERTEX_POINT('',#28637);
#4056=VERTEX_POINT('',#28641);
#4057=VERTEX_POINT('',#28643);
#4058=VERTEX_POINT('',#28653);
#4059=VERTEX_POINT('',#28654);
#4060=VERTEX_POINT('',#28656);
#4061=VERTEX_POINT('',#28658);
#4062=VERTEX_POINT('',#28662);
#4063=VERTEX_POINT('',#28664);
#4064=VERTEX_POINT('',#28668);
#4065=VERTEX_POINT('',#28670);
#4066=VERTEX_POINT('',#28680);
#4067=VERTEX_POINT('',#28681);
#4068=VERTEX_POINT('',#28683);
#4069=VERTEX_POINT('',#28685);
#4070=VERTEX_POINT('',#28689);
#4071=VERTEX_POINT('',#28691);
#4072=VERTEX_POINT('',#28695);
#4073=VERTEX_POINT('',#28697);
#4074=VERTEX_POINT('',#28701);
#4075=VERTEX_POINT('',#28703);
#4076=VERTEX_POINT('',#28707);
#4077=VERTEX_POINT('',#28709);
#4078=VERTEX_POINT('',#28718);
#4079=VERTEX_POINT('',#28721);
#4080=VERTEX_POINT('',#28724);
#4081=VERTEX_POINT('',#28728);
#4082=VERTEX_POINT('',#28732);
#4083=VERTEX_POINT('',#28736);
#4084=VERTEX_POINT('',#28739);
#4085=VERTEX_POINT('',#28746);
#4086=VERTEX_POINT('',#28747);
#4087=VERTEX_POINT('',#28749);
#4088=VERTEX_POINT('',#28751);
#4089=VERTEX_POINT('',#28755);
#4090=VERTEX_POINT('',#28757);
#4091=VERTEX_POINT('',#28761);
#4092=VERTEX_POINT('',#28763);
#4093=VERTEX_POINT('',#28767);
#4094=VERTEX_POINT('',#28769);
#4095=VERTEX_POINT('',#28773);
#4096=VERTEX_POINT('',#28775);
#4097=VERTEX_POINT('',#28784);
#4098=VERTEX_POINT('',#28786);
#4099=VERTEX_POINT('',#28789);
#4100=VERTEX_POINT('',#28794);
#4101=VERTEX_POINT('',#28797);
#4102=VERTEX_POINT('',#28801);
#4103=VERTEX_POINT('',#28805);
#4104=VERTEX_POINT('',#28809);
#4105=VERTEX_POINT('',#28812);
#4106=VERTEX_POINT('',#28819);
#4107=VERTEX_POINT('',#28821);
#4108=VERTEX_POINT('',#28825);
#4109=VERTEX_POINT('',#28827);
#4110=VERTEX_POINT('',#28834);
#4111=VERTEX_POINT('',#28835);
#4112=VERTEX_POINT('',#28839);
#4113=VERTEX_POINT('',#28843);
#4114=VERTEX_POINT('',#28846);
#4115=VERTEX_POINT('',#28850);
#4116=VERTEX_POINT('',#28854);
#4117=VERTEX_POINT('',#28862);
#4118=VERTEX_POINT('',#28864);
#4119=VERTEX_POINT('',#28866);
#4120=VERTEX_POINT('',#28870);
#4121=VERTEX_POINT('',#28874);
#4122=VERTEX_POINT('',#28878);
#4123=VERTEX_POINT('',#28882);
#4124=VERTEX_POINT('',#28897);
#4125=VERTEX_POINT('',#28899);
#4126=VERTEX_POINT('',#28946);
#4127=VERTEX_POINT('',#28947);
#4128=VERTEX_POINT('',#28949);
#4129=VERTEX_POINT('',#28957);
#4130=VERTEX_POINT('',#28979);
#4131=VERTEX_POINT('',#28980);
#4132=VERTEX_POINT('',#29069);
#4133=VERTEX_POINT('',#29070);
#4134=VERTEX_POINT('',#29159);
#4135=VERTEX_POINT('',#29160);
#4136=VERTEX_POINT('',#29162);
#4137=VERTEX_POINT('',#29188);
#4138=VERTEX_POINT('',#29228);
#4139=VERTEX_POINT('',#29229);
#4140=VERTEX_POINT('',#29231);
#4141=VERTEX_POINT('',#29245);
#4142=VERTEX_POINT('',#29262);
#4143=VERTEX_POINT('',#29263);
#4144=VERTEX_POINT('',#29300);
#4145=VERTEX_POINT('',#29301);
#4146=VERTEX_POINT('',#29338);
#4147=VERTEX_POINT('',#29339);
#4148=VERTEX_POINT('',#29341);
#4149=VERTEX_POINT('',#29348);
#4150=VERTEX_POINT('',#30261);
#4151=VERTEX_POINT('',#30262);
#4152=VERTEX_POINT('',#30264);
#4153=VERTEX_POINT('',#30266);
#4154=VERTEX_POINT('',#30268);
#4155=VERTEX_POINT('',#30270);
#4156=VERTEX_POINT('',#30275);
#4157=VERTEX_POINT('',#30276);
#4158=VERTEX_POINT('',#30281);
#4159=VERTEX_POINT('',#30285);
#4160=VERTEX_POINT('',#30289);
#4161=VERTEX_POINT('',#30293);
#4162=VERTEX_POINT('',#30303);
#4163=VERTEX_POINT('',#30304);
#4164=VERTEX_POINT('',#30306);
#4165=VERTEX_POINT('',#30314);
#4166=VERTEX_POINT('',#30336);
#4167=VERTEX_POINT('',#30337);
#4168=VERTEX_POINT('',#30426);
#4169=VERTEX_POINT('',#30427);
#4170=VERTEX_POINT('',#30516);
#4171=VERTEX_POINT('',#30517);
#4172=VERTEX_POINT('',#30519);
#4173=VERTEX_POINT('',#30545);
#4174=VERTEX_POINT('',#30585);
#4175=VERTEX_POINT('',#30586);
#4176=VERTEX_POINT('',#30588);
#4177=VERTEX_POINT('',#30602);
#4178=VERTEX_POINT('',#30619);
#4179=VERTEX_POINT('',#30620);
#4180=VERTEX_POINT('',#30657);
#4181=VERTEX_POINT('',#30658);
#4182=VERTEX_POINT('',#30695);
#4183=VERTEX_POINT('',#30696);
#4184=VERTEX_POINT('',#30698);
#4185=VERTEX_POINT('',#30705);
#4186=VERTEX_POINT('',#31618);
#4187=VERTEX_POINT('',#31619);
#4188=VERTEX_POINT('',#31621);
#4189=VERTEX_POINT('',#31623);
#4190=VERTEX_POINT('',#31625);
#4191=VERTEX_POINT('',#31627);
#4192=VERTEX_POINT('',#31632);
#4193=VERTEX_POINT('',#31633);
#4194=VERTEX_POINT('',#31638);
#4195=VERTEX_POINT('',#31642);
#4196=VERTEX_POINT('',#31646);
#4197=VERTEX_POINT('',#31650);
#4198=VERTEX_POINT('',#31660);
#4199=VERTEX_POINT('',#31661);
#4200=VERTEX_POINT('',#31663);
#4201=VERTEX_POINT('',#31671);
#4202=VERTEX_POINT('',#31693);
#4203=VERTEX_POINT('',#31694);
#4204=VERTEX_POINT('',#31783);
#4205=VERTEX_POINT('',#31784);
#4206=VERTEX_POINT('',#31873);
#4207=VERTEX_POINT('',#31874);
#4208=VERTEX_POINT('',#31876);
#4209=VERTEX_POINT('',#31902);
#4210=VERTEX_POINT('',#31942);
#4211=VERTEX_POINT('',#31943);
#4212=VERTEX_POINT('',#31945);
#4213=VERTEX_POINT('',#31959);
#4214=VERTEX_POINT('',#31976);
#4215=VERTEX_POINT('',#31977);
#4216=VERTEX_POINT('',#32014);
#4217=VERTEX_POINT('',#32015);
#4218=VERTEX_POINT('',#32052);
#4219=VERTEX_POINT('',#32053);
#4220=VERTEX_POINT('',#32055);
#4221=VERTEX_POINT('',#32062);
#4222=VERTEX_POINT('',#32975);
#4223=VERTEX_POINT('',#32976);
#4224=VERTEX_POINT('',#32978);
#4225=VERTEX_POINT('',#32980);
#4226=VERTEX_POINT('',#32982);
#4227=VERTEX_POINT('',#32984);
#4228=VERTEX_POINT('',#32989);
#4229=VERTEX_POINT('',#32990);
#4230=VERTEX_POINT('',#32995);
#4231=VERTEX_POINT('',#32999);
#4232=VERTEX_POINT('',#33003);
#4233=VERTEX_POINT('',#33007);
#4234=VERTEX_POINT('',#33017);
#4235=VERTEX_POINT('',#33018);
#4236=VERTEX_POINT('',#33020);
#4237=VERTEX_POINT('',#33028);
#4238=VERTEX_POINT('',#33050);
#4239=VERTEX_POINT('',#33051);
#4240=VERTEX_POINT('',#33140);
#4241=VERTEX_POINT('',#33141);
#4242=VERTEX_POINT('',#33230);
#4243=VERTEX_POINT('',#33231);
#4244=VERTEX_POINT('',#33233);
#4245=VERTEX_POINT('',#33259);
#4246=VERTEX_POINT('',#33299);
#4247=VERTEX_POINT('',#33300);
#4248=VERTEX_POINT('',#33302);
#4249=VERTEX_POINT('',#33316);
#4250=VERTEX_POINT('',#33333);
#4251=VERTEX_POINT('',#33334);
#4252=VERTEX_POINT('',#33371);
#4253=VERTEX_POINT('',#33372);
#4254=VERTEX_POINT('',#33409);
#4255=VERTEX_POINT('',#33410);
#4256=VERTEX_POINT('',#33412);
#4257=VERTEX_POINT('',#33419);
#4258=VERTEX_POINT('',#34332);
#4259=VERTEX_POINT('',#34333);
#4260=VERTEX_POINT('',#34335);
#4261=VERTEX_POINT('',#34337);
#4262=VERTEX_POINT('',#34339);
#4263=VERTEX_POINT('',#34341);
#4264=VERTEX_POINT('',#34346);
#4265=VERTEX_POINT('',#34347);
#4266=VERTEX_POINT('',#34352);
#4267=VERTEX_POINT('',#34356);
#4268=VERTEX_POINT('',#34360);
#4269=VERTEX_POINT('',#34364);
#4270=EDGE_CURVE('',#3444,#3444,#3310,.T.);
#4271=EDGE_CURVE('',#3444,#3445,#2076,.T.);
#4272=EDGE_CURVE('',#3445,#3445,#3311,.T.);
#4273=EDGE_CURVE('',#3446,#3446,#3312,.T.);
#4274=EDGE_CURVE('',#3446,#3447,#2077,.T.);
#4275=EDGE_CURVE('',#3447,#3447,#3313,.T.);
#4276=EDGE_CURVE('',#3448,#3448,#3314,.T.);
#4277=EDGE_CURVE('',#3448,#3449,#2078,.T.);
#4278=EDGE_CURVE('',#3449,#3449,#3315,.T.);
#4279=EDGE_CURVE('',#3450,#3450,#3316,.T.);
#4280=EDGE_CURVE('',#3450,#3451,#2079,.T.);
#4281=EDGE_CURVE('',#3451,#3451,#3317,.T.);
#4282=EDGE_CURVE('',#3452,#3452,#3318,.T.);
#4283=EDGE_CURVE('',#3452,#3453,#2080,.T.);
#4284=EDGE_CURVE('',#3453,#3453,#3319,.T.);
#4285=EDGE_CURVE('',#3454,#3454,#3320,.T.);
#4286=EDGE_CURVE('',#3454,#3455,#2081,.T.);
#4287=EDGE_CURVE('',#3455,#3455,#3321,.T.);
#4288=EDGE_CURVE('',#3456,#3457,#2082,.T.);
#4289=EDGE_CURVE('',#3457,#3458,#2083,.T.);
#4290=EDGE_CURVE('',#3459,#3458,#2084,.T.);
#4291=EDGE_CURVE('',#3456,#3459,#2085,.T.);
#4292=EDGE_CURVE('',#3460,#3456,#2086,.T.);
#4293=EDGE_CURVE('',#3461,#3459,#2087,.T.);
#4294=EDGE_CURVE('',#3460,#3461,#2088,.T.);
#4295=EDGE_CURVE('',#3462,#3460,#2089,.T.);
#4296=EDGE_CURVE('',#3463,#3461,#2090,.T.);
#4297=EDGE_CURVE('',#3462,#3463,#2091,.T.);
#4298=EDGE_CURVE('',#3457,#3462,#2092,.T.);
#4299=EDGE_CURVE('',#3458,#3463,#2093,.T.);
#4300=EDGE_CURVE('',#3464,#3465,#2094,.T.);
#4301=EDGE_CURVE('',#3464,#3466,#217,.T.);
#4302=EDGE_CURVE('',#3466,#3467,#3322,.F.);
#4303=EDGE_CURVE('',#3467,#3465,#218,.T.);
#4304=EDGE_CURVE('',#3468,#3469,#2095,.T.);
#4305=EDGE_CURVE('',#3468,#3464,#219,.T.);
#4306=EDGE_CURVE('',#3465,#3469,#220,.T.);
#4307=EDGE_CURVE('',#3470,#3471,#2096,.T.);
#4308=EDGE_CURVE('',#3470,#3468,#221,.T.);
#4309=EDGE_CURVE('',#3469,#3471,#222,.T.);
#4310=EDGE_CURVE('',#3472,#3473,#2097,.T.);
#4311=EDGE_CURVE('',#3472,#3470,#223,.T.);
#4312=EDGE_CURVE('',#3471,#3473,#224,.T.);
#4313=EDGE_CURVE('',#3474,#3475,#2098,.T.);
#4314=EDGE_CURVE('',#3474,#3472,#225,.T.);
#4315=EDGE_CURVE('',#3473,#3475,#226,.T.);
#4316=EDGE_CURVE('',#3476,#3477,#2099,.T.);
#4317=EDGE_CURVE('',#3476,#3474,#227,.T.);
#4318=EDGE_CURVE('',#3475,#3477,#228,.T.);
#4319=EDGE_CURVE('',#3478,#3479,#2100,.T.);
#4320=EDGE_CURVE('',#3478,#3476,#229,.T.);
#4321=EDGE_CURVE('',#3477,#3479,#230,.T.);
#4322=EDGE_CURVE('',#3480,#3481,#2101,.T.);
#4323=EDGE_CURVE('',#3480,#3478,#231,.T.);
#4324=EDGE_CURVE('',#3479,#3481,#232,.T.);
#4325=EDGE_CURVE('',#3482,#3483,#2102,.T.);
#4326=EDGE_CURVE('',#3482,#3480,#233,.T.);
#4327=EDGE_CURVE('',#3481,#3483,#234,.T.);
#4328=EDGE_CURVE('',#3484,#3485,#2103,.T.);
#4329=EDGE_CURVE('',#3484,#3482,#235,.T.);
#4330=EDGE_CURVE('',#3483,#3485,#236,.T.);
#4331=EDGE_CURVE('',#3486,#3487,#2104,.T.);
#4332=EDGE_CURVE('',#3486,#3484,#237,.T.);
#4333=EDGE_CURVE('',#3485,#3487,#238,.T.);
#4334=EDGE_CURVE('',#3488,#3489,#2105,.T.);
#4335=EDGE_CURVE('',#3488,#3486,#239,.T.);
#4336=EDGE_CURVE('',#3487,#3489,#240,.T.);
#4337=EDGE_CURVE('',#3490,#3491,#2106,.T.);
#4338=EDGE_CURVE('',#3490,#3488,#241,.T.);
#4339=EDGE_CURVE('',#3489,#3491,#242,.T.);
#4340=EDGE_CURVE('',#3492,#3493,#2107,.T.);
#4341=EDGE_CURVE('',#3492,#3490,#243,.T.);
#4342=EDGE_CURVE('',#3491,#3493,#244,.T.);
#4343=EDGE_CURVE('',#3494,#3495,#2108,.T.);
#4344=EDGE_CURVE('',#3494,#3492,#245,.T.);
#4345=EDGE_CURVE('',#3493,#3495,#246,.T.);
#4346=EDGE_CURVE('',#3496,#3497,#2109,.T.);
#4347=EDGE_CURVE('',#3496,#3494,#247,.T.);
#4348=EDGE_CURVE('',#3495,#3497,#248,.T.);
#4349=EDGE_CURVE('',#3498,#3499,#2110,.T.);
#4350=EDGE_CURVE('',#3498,#3496,#249,.T.);
#4351=EDGE_CURVE('',#3497,#3499,#250,.T.);
#4352=EDGE_CURVE('',#3500,#3501,#2111,.T.);
#4353=EDGE_CURVE('',#3500,#3498,#251,.T.);
#4354=EDGE_CURVE('',#3499,#3501,#252,.T.);
#4355=EDGE_CURVE('',#3502,#3503,#2112,.T.);
#4356=EDGE_CURVE('',#3502,#3500,#253,.T.);
#4357=EDGE_CURVE('',#3501,#3503,#254,.T.);
#4358=EDGE_CURVE('',#3504,#3505,#2113,.T.);
#4359=EDGE_CURVE('',#3504,#3502,#255,.T.);
#4360=EDGE_CURVE('',#3503,#3505,#256,.T.);
#4361=EDGE_CURVE('',#3506,#3507,#2114,.T.);
#4362=EDGE_CURVE('',#3506,#3504,#257,.T.);
#4363=EDGE_CURVE('',#3505,#3507,#258,.T.);
#4364=EDGE_CURVE('',#3508,#3509,#2115,.T.);
#4365=EDGE_CURVE('',#3508,#3506,#259,.T.);
#4366=EDGE_CURVE('',#3507,#3509,#260,.T.);
#4367=EDGE_CURVE('',#3510,#3511,#2116,.T.);
#4368=EDGE_CURVE('',#3510,#3508,#261,.T.);
#4369=EDGE_CURVE('',#3509,#3511,#262,.T.);
#4370=EDGE_CURVE('',#3512,#3513,#2117,.T.);
#4371=EDGE_CURVE('',#3512,#3510,#263,.T.);
#4372=EDGE_CURVE('',#3511,#3513,#264,.T.);
#4373=EDGE_CURVE('',#3514,#3515,#2118,.T.);
#4374=EDGE_CURVE('',#3514,#3512,#265,.T.);
#4375=EDGE_CURVE('',#3513,#3515,#266,.T.);
#4376=EDGE_CURVE('',#3516,#3517,#2119,.T.);
#4377=EDGE_CURVE('',#3516,#3514,#267,.T.);
#4378=EDGE_CURVE('',#3515,#3517,#268,.T.);
#4379=EDGE_CURVE('',#3518,#3519,#2120,.T.);
#4380=EDGE_CURVE('',#3518,#3516,#269,.T.);
#4381=EDGE_CURVE('',#3517,#3519,#270,.T.);
#4382=EDGE_CURVE('',#3520,#3521,#2121,.T.);
#4383=EDGE_CURVE('',#3520,#3518,#271,.T.);
#4384=EDGE_CURVE('',#3519,#3521,#272,.T.);
#4385=EDGE_CURVE('',#3522,#3523,#2122,.T.);
#4386=EDGE_CURVE('',#3522,#3520,#273,.T.);
#4387=EDGE_CURVE('',#3521,#3523,#274,.T.);
#4388=EDGE_CURVE('',#3524,#3525,#2123,.T.);
#4389=EDGE_CURVE('',#3524,#3522,#275,.T.);
#4390=EDGE_CURVE('',#3523,#3525,#276,.T.);
#4391=EDGE_CURVE('',#3526,#3527,#2124,.T.);
#4392=EDGE_CURVE('',#3526,#3524,#277,.T.);
#4393=EDGE_CURVE('',#3525,#3527,#278,.T.);
#4394=EDGE_CURVE('',#3528,#3529,#2125,.T.);
#4395=EDGE_CURVE('',#3528,#3526,#279,.T.);
#4396=EDGE_CURVE('',#3527,#3529,#280,.T.);
#4397=EDGE_CURVE('',#3530,#3531,#2126,.T.);
#4398=EDGE_CURVE('',#3530,#3528,#281,.T.);
#4399=EDGE_CURVE('',#3529,#3531,#282,.T.);
#4400=EDGE_CURVE('',#3532,#3533,#2127,.T.);
#4401=EDGE_CURVE('',#3532,#3530,#283,.T.);
#4402=EDGE_CURVE('',#3531,#3533,#284,.T.);
#4403=EDGE_CURVE('',#3534,#3535,#2128,.T.);
#4404=EDGE_CURVE('',#3534,#3532,#285,.T.);
#4405=EDGE_CURVE('',#3533,#3535,#286,.T.);
#4406=EDGE_CURVE('',#3536,#3537,#2129,.T.);
#4407=EDGE_CURVE('',#3536,#3534,#287,.T.);
#4408=EDGE_CURVE('',#3535,#3537,#288,.T.);
#4409=EDGE_CURVE('',#3538,#3539,#2130,.T.);
#4410=EDGE_CURVE('',#3538,#3536,#289,.T.);
#4411=EDGE_CURVE('',#3537,#3539,#290,.T.);
#4412=EDGE_CURVE('',#3540,#3541,#2131,.T.);
#4413=EDGE_CURVE('',#3540,#3538,#291,.T.);
#4414=EDGE_CURVE('',#3539,#3541,#292,.T.);
#4415=EDGE_CURVE('',#3542,#3543,#2132,.T.);
#4416=EDGE_CURVE('',#3542,#3540,#293,.T.);
#4417=EDGE_CURVE('',#3541,#3543,#294,.T.);
#4418=EDGE_CURVE('',#3544,#3545,#2133,.T.);
#4419=EDGE_CURVE('',#3544,#3542,#295,.T.);
#4420=EDGE_CURVE('',#3543,#3545,#296,.T.);
#4421=EDGE_CURVE('',#3546,#3547,#2134,.T.);
#4422=EDGE_CURVE('',#3546,#3544,#297,.T.);
#4423=EDGE_CURVE('',#3545,#3547,#298,.T.);
#4424=EDGE_CURVE('',#3548,#3549,#2135,.T.);
#4425=EDGE_CURVE('',#3548,#3546,#299,.T.);
#4426=EDGE_CURVE('',#3547,#3549,#300,.T.);
#4427=EDGE_CURVE('',#3550,#3551,#2136,.T.);
#4428=EDGE_CURVE('',#3550,#3548,#301,.T.);
#4429=EDGE_CURVE('',#3549,#3551,#302,.T.);
#4430=EDGE_CURVE('',#3552,#3553,#2137,.T.);
#4431=EDGE_CURVE('',#3552,#3550,#303,.T.);
#4432=EDGE_CURVE('',#3551,#3553,#304,.T.);
#4433=EDGE_CURVE('',#3554,#3555,#2138,.T.);
#4434=EDGE_CURVE('',#3554,#3552,#305,.T.);
#4435=EDGE_CURVE('',#3553,#3555,#306,.T.);
#4436=EDGE_CURVE('',#3556,#3557,#2139,.T.);
#4437=EDGE_CURVE('',#3556,#3554,#307,.T.);
#4438=EDGE_CURVE('',#3555,#3557,#308,.T.);
#4439=EDGE_CURVE('',#3558,#3559,#2140,.T.);
#4440=EDGE_CURVE('',#3558,#3556,#309,.T.);
#4441=EDGE_CURVE('',#3557,#3559,#310,.T.);
#4442=EDGE_CURVE('',#3560,#3561,#2141,.T.);
#4443=EDGE_CURVE('',#3560,#3558,#311,.T.);
#4444=EDGE_CURVE('',#3559,#3561,#312,.T.);
#4445=EDGE_CURVE('',#3562,#3563,#2142,.T.);
#4446=EDGE_CURVE('',#3562,#3560,#313,.T.);
#4447=EDGE_CURVE('',#3561,#3563,#314,.T.);
#4448=EDGE_CURVE('',#3564,#3565,#2143,.T.);
#4449=EDGE_CURVE('',#3564,#3562,#315,.T.);
#4450=EDGE_CURVE('',#3563,#3565,#316,.T.);
#4451=EDGE_CURVE('',#3566,#3567,#2144,.T.);
#4452=EDGE_CURVE('',#3566,#3564,#317,.T.);
#4453=EDGE_CURVE('',#3565,#3567,#318,.T.);
#4454=EDGE_CURVE('',#3568,#3569,#2145,.T.);
#4455=EDGE_CURVE('',#3568,#3566,#319,.T.);
#4456=EDGE_CURVE('',#3567,#3569,#320,.T.);
#4457=EDGE_CURVE('',#3570,#3571,#2146,.T.);
#4458=EDGE_CURVE('',#3570,#3568,#321,.T.);
#4459=EDGE_CURVE('',#3569,#3571,#322,.T.);
#4460=EDGE_CURVE('',#3572,#3573,#2147,.T.);
#4461=EDGE_CURVE('',#3572,#3570,#323,.T.);
#4462=EDGE_CURVE('',#3571,#3573,#324,.T.);
#4463=EDGE_CURVE('',#3574,#3575,#2148,.T.);
#4464=EDGE_CURVE('',#3574,#3572,#325,.T.);
#4465=EDGE_CURVE('',#3573,#3575,#326,.T.);
#4466=EDGE_CURVE('',#3576,#3577,#2149,.T.);
#4467=EDGE_CURVE('',#3576,#3574,#327,.T.);
#4468=EDGE_CURVE('',#3575,#3577,#328,.T.);
#4469=EDGE_CURVE('',#3578,#3579,#2150,.T.);
#4470=EDGE_CURVE('',#3578,#3576,#329,.T.);
#4471=EDGE_CURVE('',#3577,#3579,#330,.T.);
#4472=EDGE_CURVE('',#3580,#3581,#2151,.T.);
#4473=EDGE_CURVE('',#3580,#3578,#331,.T.);
#4474=EDGE_CURVE('',#3579,#3581,#332,.T.);
#4475=EDGE_CURVE('',#3582,#3583,#2152,.T.);
#4476=EDGE_CURVE('',#3582,#3580,#333,.T.);
#4477=EDGE_CURVE('',#3581,#3583,#334,.T.);
#4478=EDGE_CURVE('',#3584,#3585,#2153,.T.);
#4479=EDGE_CURVE('',#3584,#3582,#335,.T.);
#4480=EDGE_CURVE('',#3583,#3585,#336,.T.);
#4481=EDGE_CURVE('',#3586,#3587,#2154,.T.);
#4482=EDGE_CURVE('',#3586,#3584,#337,.T.);
#4483=EDGE_CURVE('',#3585,#3587,#338,.T.);
#4484=EDGE_CURVE('',#3588,#3589,#2155,.T.);
#4485=EDGE_CURVE('',#3588,#3586,#339,.T.);
#4486=EDGE_CURVE('',#3587,#3589,#340,.T.);
#4487=EDGE_CURVE('',#3590,#3591,#2156,.T.);
#4488=EDGE_CURVE('',#3590,#3588,#341,.T.);
#4489=EDGE_CURVE('',#3589,#3591,#342,.T.);
#4490=EDGE_CURVE('',#3592,#3593,#2157,.T.);
#4491=EDGE_CURVE('',#3592,#3590,#343,.T.);
#4492=EDGE_CURVE('',#3591,#3593,#344,.T.);
#4493=EDGE_CURVE('',#3594,#3595,#2158,.T.);
#4494=EDGE_CURVE('',#3594,#3592,#345,.T.);
#4495=EDGE_CURVE('',#3593,#3595,#346,.T.);
#4496=EDGE_CURVE('',#3596,#3597,#2159,.T.);
#4497=EDGE_CURVE('',#3596,#3594,#347,.T.);
#4498=EDGE_CURVE('',#3595,#3597,#348,.T.);
#4499=EDGE_CURVE('',#3598,#3599,#2160,.T.);
#4500=EDGE_CURVE('',#3598,#3596,#349,.T.);
#4501=EDGE_CURVE('',#3597,#3599,#350,.T.);
#4502=EDGE_CURVE('',#3600,#3601,#2161,.T.);
#4503=EDGE_CURVE('',#3600,#3598,#351,.T.);
#4504=EDGE_CURVE('',#3599,#3601,#352,.T.);
#4505=EDGE_CURVE('',#3602,#3603,#2162,.T.);
#4506=EDGE_CURVE('',#3602,#3600,#353,.T.);
#4507=EDGE_CURVE('',#3601,#3603,#354,.T.);
#4508=EDGE_CURVE('',#3604,#3605,#2163,.T.);
#4509=EDGE_CURVE('',#3604,#3602,#355,.T.);
#4510=EDGE_CURVE('',#3603,#3605,#356,.T.);
#4511=EDGE_CURVE('',#3606,#3607,#2164,.T.);
#4512=EDGE_CURVE('',#3606,#3604,#357,.T.);
#4513=EDGE_CURVE('',#3605,#3607,#358,.T.);
#4514=EDGE_CURVE('',#3608,#3609,#2165,.T.);
#4515=EDGE_CURVE('',#3608,#3606,#359,.T.);
#4516=EDGE_CURVE('',#3607,#3609,#360,.T.);
#4517=EDGE_CURVE('',#3610,#3611,#2166,.T.);
#4518=EDGE_CURVE('',#3610,#3608,#361,.T.);
#4519=EDGE_CURVE('',#3609,#3611,#362,.T.);
#4520=EDGE_CURVE('',#3612,#3613,#2167,.T.);
#4521=EDGE_CURVE('',#3612,#3610,#363,.T.);
#4522=EDGE_CURVE('',#3611,#3613,#364,.T.);
#4523=EDGE_CURVE('',#3614,#3615,#2168,.T.);
#4524=EDGE_CURVE('',#3614,#3612,#365,.T.);
#4525=EDGE_CURVE('',#3613,#3615,#366,.T.);
#4526=EDGE_CURVE('',#3616,#3617,#2169,.T.);
#4527=EDGE_CURVE('',#3616,#3614,#367,.T.);
#4528=EDGE_CURVE('',#3615,#3617,#368,.T.);
#4529=EDGE_CURVE('',#3618,#3619,#2170,.T.);
#4530=EDGE_CURVE('',#3618,#3616,#369,.T.);
#4531=EDGE_CURVE('',#3617,#3619,#370,.T.);
#4532=EDGE_CURVE('',#3620,#3621,#2171,.T.);
#4533=EDGE_CURVE('',#3620,#3618,#371,.T.);
#4534=EDGE_CURVE('',#3619,#3621,#372,.T.);
#4535=EDGE_CURVE('',#3622,#3623,#2172,.T.);
#4536=EDGE_CURVE('',#3622,#3620,#373,.T.);
#4537=EDGE_CURVE('',#3621,#3623,#374,.T.);
#4538=EDGE_CURVE('',#3624,#3625,#2173,.T.);
#4539=EDGE_CURVE('',#3624,#3622,#375,.T.);
#4540=EDGE_CURVE('',#3623,#3625,#376,.T.);
#4541=EDGE_CURVE('',#3626,#3627,#2174,.T.);
#4542=EDGE_CURVE('',#3626,#3624,#377,.T.);
#4543=EDGE_CURVE('',#3625,#3627,#378,.T.);
#4544=EDGE_CURVE('',#3628,#3629,#2175,.T.);
#4545=EDGE_CURVE('',#3628,#3626,#379,.T.);
#4546=EDGE_CURVE('',#3627,#3629,#380,.T.);
#4547=EDGE_CURVE('',#3630,#3631,#2176,.T.);
#4548=EDGE_CURVE('',#3630,#3628,#381,.T.);
#4549=EDGE_CURVE('',#3629,#3631,#382,.T.);
#4550=EDGE_CURVE('',#3632,#3633,#2177,.T.);
#4551=EDGE_CURVE('',#3632,#3630,#383,.T.);
#4552=EDGE_CURVE('',#3631,#3633,#384,.T.);
#4553=EDGE_CURVE('',#3634,#3635,#2178,.T.);
#4554=EDGE_CURVE('',#3634,#3632,#385,.T.);
#4555=EDGE_CURVE('',#3633,#3635,#386,.T.);
#4556=EDGE_CURVE('',#3636,#3637,#2179,.T.);
#4557=EDGE_CURVE('',#3636,#3634,#387,.T.);
#4558=EDGE_CURVE('',#3635,#3637,#388,.T.);
#4559=EDGE_CURVE('',#3638,#3639,#2180,.T.);
#4560=EDGE_CURVE('',#3638,#3636,#389,.T.);
#4561=EDGE_CURVE('',#3637,#3639,#390,.T.);
#4562=EDGE_CURVE('',#3640,#3641,#2181,.T.);
#4563=EDGE_CURVE('',#3640,#3638,#391,.T.);
#4564=EDGE_CURVE('',#3639,#3641,#392,.T.);
#4565=EDGE_CURVE('',#3642,#3643,#2182,.T.);
#4566=EDGE_CURVE('',#3642,#3640,#393,.T.);
#4567=EDGE_CURVE('',#3641,#3643,#394,.T.);
#4568=EDGE_CURVE('',#3644,#3645,#2183,.T.);
#4569=EDGE_CURVE('',#3644,#3642,#395,.T.);
#4570=EDGE_CURVE('',#3643,#3645,#396,.T.);
#4571=EDGE_CURVE('',#3646,#3647,#2184,.T.);
#4572=EDGE_CURVE('',#3646,#3644,#397,.T.);
#4573=EDGE_CURVE('',#3645,#3647,#398,.T.);
#4574=EDGE_CURVE('',#3648,#3649,#2185,.T.);
#4575=EDGE_CURVE('',#3648,#3646,#399,.T.);
#4576=EDGE_CURVE('',#3647,#3649,#400,.T.);
#4577=EDGE_CURVE('',#3650,#3651,#2186,.T.);
#4578=EDGE_CURVE('',#3650,#3648,#401,.T.);
#4579=EDGE_CURVE('',#3649,#3651,#402,.T.);
#4580=EDGE_CURVE('',#3652,#3653,#2187,.T.);
#4581=EDGE_CURVE('',#3652,#3650,#403,.T.);
#4582=EDGE_CURVE('',#3651,#3653,#404,.T.);
#4583=EDGE_CURVE('',#3654,#3655,#2188,.T.);
#4584=EDGE_CURVE('',#3654,#3656,#405,.T.);
#4585=EDGE_CURVE('',#3657,#3656,#3323,.T.);
#4586=EDGE_CURVE('',#3655,#3657,#406,.T.);
#4587=EDGE_CURVE('',#3658,#3659,#2189,.T.);
#4588=EDGE_CURVE('',#3658,#3654,#407,.T.);
#4589=EDGE_CURVE('',#3659,#3655,#408,.T.);
#4590=EDGE_CURVE('',#3660,#3661,#2190,.T.);
#4591=EDGE_CURVE('',#3660,#3658,#409,.T.);
#4592=EDGE_CURVE('',#3661,#3659,#410,.T.);
#4593=EDGE_CURVE('',#3662,#3663,#2191,.T.);
#4594=EDGE_CURVE('',#3662,#3660,#411,.T.);
#4595=EDGE_CURVE('',#3663,#3661,#412,.T.);
#4596=EDGE_CURVE('',#3664,#3665,#2192,.T.);
#4597=EDGE_CURVE('',#3664,#3662,#413,.T.);
#4598=EDGE_CURVE('',#3665,#3663,#414,.T.);
#4599=EDGE_CURVE('',#3666,#3667,#2193,.T.);
#4600=EDGE_CURVE('',#3666,#3664,#415,.T.);
#4601=EDGE_CURVE('',#3667,#3665,#416,.T.);
#4602=EDGE_CURVE('',#3668,#3669,#2194,.T.);
#4603=EDGE_CURVE('',#3668,#3666,#417,.T.);
#4604=EDGE_CURVE('',#3669,#3667,#418,.T.);
#4605=EDGE_CURVE('',#3670,#3671,#2195,.T.);
#4606=EDGE_CURVE('',#3670,#3668,#419,.T.);
#4607=EDGE_CURVE('',#3671,#3669,#420,.T.);
#4608=EDGE_CURVE('',#3672,#3673,#2196,.T.);
#4609=EDGE_CURVE('',#3672,#3670,#421,.T.);
#4610=EDGE_CURVE('',#3673,#3671,#422,.T.);
#4611=EDGE_CURVE('',#3674,#3675,#2197,.T.);
#4612=EDGE_CURVE('',#3674,#3672,#423,.T.);
#4613=EDGE_CURVE('',#3675,#3673,#424,.T.);
#4614=EDGE_CURVE('',#3676,#3677,#2198,.T.);
#4615=EDGE_CURVE('',#3676,#3674,#425,.T.);
#4616=EDGE_CURVE('',#3677,#3675,#426,.T.);
#4617=EDGE_CURVE('',#3678,#3679,#2199,.T.);
#4618=EDGE_CURVE('',#3678,#3676,#427,.T.);
#4619=EDGE_CURVE('',#3679,#3677,#428,.T.);
#4620=EDGE_CURVE('',#3680,#3681,#2200,.T.);
#4621=EDGE_CURVE('',#3680,#3678,#429,.T.);
#4622=EDGE_CURVE('',#3681,#3679,#430,.T.);
#4623=EDGE_CURVE('',#3682,#3683,#2201,.T.);
#4624=EDGE_CURVE('',#3682,#3680,#431,.T.);
#4625=EDGE_CURVE('',#3683,#3681,#432,.T.);
#4626=EDGE_CURVE('',#3684,#3685,#2202,.T.);
#4627=EDGE_CURVE('',#3684,#3682,#433,.T.);
#4628=EDGE_CURVE('',#3685,#3683,#434,.T.);
#4629=EDGE_CURVE('',#3686,#3687,#2203,.T.);
#4630=EDGE_CURVE('',#3686,#3684,#435,.T.);
#4631=EDGE_CURVE('',#3687,#3685,#436,.T.);
#4632=EDGE_CURVE('',#3688,#3689,#2204,.T.);
#4633=EDGE_CURVE('',#3688,#3686,#437,.T.);
#4634=EDGE_CURVE('',#3689,#3687,#438,.T.);
#4635=EDGE_CURVE('',#3690,#3691,#2205,.T.);
#4636=EDGE_CURVE('',#3690,#3688,#439,.T.);
#4637=EDGE_CURVE('',#3691,#3689,#440,.T.);
#4638=EDGE_CURVE('',#3692,#3693,#2206,.T.);
#4639=EDGE_CURVE('',#3692,#3690,#441,.T.);
#4640=EDGE_CURVE('',#3693,#3691,#442,.T.);
#4641=EDGE_CURVE('',#3694,#3695,#2207,.T.);
#4642=EDGE_CURVE('',#3694,#3692,#443,.T.);
#4643=EDGE_CURVE('',#3695,#3693,#444,.T.);
#4644=EDGE_CURVE('',#3696,#3697,#2208,.T.);
#4645=EDGE_CURVE('',#3696,#3694,#445,.T.);
#4646=EDGE_CURVE('',#3697,#3695,#446,.T.);
#4647=EDGE_CURVE('',#3698,#3699,#2209,.T.);
#4648=EDGE_CURVE('',#3698,#3696,#447,.T.);
#4649=EDGE_CURVE('',#3699,#3697,#448,.T.);
#4650=EDGE_CURVE('',#3700,#3701,#2210,.T.);
#4651=EDGE_CURVE('',#3700,#3698,#449,.T.);
#4652=EDGE_CURVE('',#3701,#3699,#450,.T.);
#4653=EDGE_CURVE('',#3702,#3703,#2211,.T.);
#4654=EDGE_CURVE('',#3702,#3700,#451,.T.);
#4655=EDGE_CURVE('',#3703,#3701,#452,.T.);
#4656=EDGE_CURVE('',#3704,#3705,#2212,.T.);
#4657=EDGE_CURVE('',#3704,#3702,#453,.T.);
#4658=EDGE_CURVE('',#3705,#3703,#454,.T.);
#4659=EDGE_CURVE('',#3706,#3707,#2213,.T.);
#4660=EDGE_CURVE('',#3706,#3704,#455,.T.);
#4661=EDGE_CURVE('',#3707,#3705,#456,.T.);
#4662=EDGE_CURVE('',#3708,#3709,#2214,.T.);
#4663=EDGE_CURVE('',#3708,#3706,#457,.T.);
#4664=EDGE_CURVE('',#3709,#3707,#458,.T.);
#4665=EDGE_CURVE('',#3710,#3711,#2215,.T.);
#4666=EDGE_CURVE('',#3710,#3708,#459,.T.);
#4667=EDGE_CURVE('',#3711,#3709,#460,.T.);
#4668=EDGE_CURVE('',#3712,#3713,#2216,.T.);
#4669=EDGE_CURVE('',#3712,#3710,#461,.T.);
#4670=EDGE_CURVE('',#3713,#3711,#462,.T.);
#4671=EDGE_CURVE('',#3714,#3715,#2217,.T.);
#4672=EDGE_CURVE('',#3714,#3712,#463,.T.);
#4673=EDGE_CURVE('',#3715,#3713,#464,.T.);
#4674=EDGE_CURVE('',#3716,#3717,#2218,.T.);
#4675=EDGE_CURVE('',#3716,#3714,#465,.T.);
#4676=EDGE_CURVE('',#3717,#3715,#466,.T.);
#4677=EDGE_CURVE('',#3718,#3719,#2219,.T.);
#4678=EDGE_CURVE('',#3718,#3716,#467,.T.);
#4679=EDGE_CURVE('',#3719,#3717,#468,.T.);
#4680=EDGE_CURVE('',#3720,#3721,#2220,.T.);
#4681=EDGE_CURVE('',#3720,#3718,#469,.T.);
#4682=EDGE_CURVE('',#3721,#3719,#470,.T.);
#4683=EDGE_CURVE('',#3722,#3723,#2221,.T.);
#4684=EDGE_CURVE('',#3722,#3720,#471,.T.);
#4685=EDGE_CURVE('',#3723,#3721,#472,.T.);
#4686=EDGE_CURVE('',#3724,#3725,#2222,.T.);
#4687=EDGE_CURVE('',#3724,#3722,#473,.T.);
#4688=EDGE_CURVE('',#3725,#3723,#474,.T.);
#4689=EDGE_CURVE('',#3726,#3727,#2223,.T.);
#4690=EDGE_CURVE('',#3726,#3724,#475,.T.);
#4691=EDGE_CURVE('',#3727,#3725,#476,.T.);
#4692=EDGE_CURVE('',#3728,#3729,#2224,.T.);
#4693=EDGE_CURVE('',#3728,#3726,#477,.T.);
#4694=EDGE_CURVE('',#3729,#3727,#478,.T.);
#4695=EDGE_CURVE('',#3730,#3731,#2225,.T.);
#4696=EDGE_CURVE('',#3730,#3728,#479,.T.);
#4697=EDGE_CURVE('',#3731,#3729,#480,.T.);
#4698=EDGE_CURVE('',#3732,#3733,#2226,.T.);
#4699=EDGE_CURVE('',#3732,#3730,#481,.T.);
#4700=EDGE_CURVE('',#3733,#3731,#482,.T.);
#4701=EDGE_CURVE('',#3734,#3735,#2227,.T.);
#4702=EDGE_CURVE('',#3734,#3732,#483,.T.);
#4703=EDGE_CURVE('',#3735,#3733,#484,.T.);
#4704=EDGE_CURVE('',#3736,#3737,#2228,.T.);
#4705=EDGE_CURVE('',#3736,#3734,#485,.T.);
#4706=EDGE_CURVE('',#3737,#3735,#486,.T.);
#4707=EDGE_CURVE('',#3738,#3739,#2229,.T.);
#4708=EDGE_CURVE('',#3738,#3736,#487,.T.);
#4709=EDGE_CURVE('',#3739,#3737,#488,.T.);
#4710=EDGE_CURVE('',#3740,#3741,#2230,.T.);
#4711=EDGE_CURVE('',#3740,#3738,#489,.T.);
#4712=EDGE_CURVE('',#3741,#3739,#490,.T.);
#4713=EDGE_CURVE('',#3742,#3743,#2231,.T.);
#4714=EDGE_CURVE('',#3742,#3740,#491,.T.);
#4715=EDGE_CURVE('',#3743,#3741,#492,.T.);
#4716=EDGE_CURVE('',#3744,#3745,#2232,.T.);
#4717=EDGE_CURVE('',#3744,#3742,#493,.T.);
#4718=EDGE_CURVE('',#3745,#3743,#494,.T.);
#4719=EDGE_CURVE('',#3746,#3747,#2233,.T.);
#4720=EDGE_CURVE('',#3746,#3744,#495,.T.);
#4721=EDGE_CURVE('',#3747,#3745,#496,.T.);
#4722=EDGE_CURVE('',#3748,#3749,#2234,.T.);
#4723=EDGE_CURVE('',#3748,#3746,#497,.T.);
#4724=EDGE_CURVE('',#3749,#3747,#498,.T.);
#4725=EDGE_CURVE('',#3750,#3751,#2235,.T.);
#4726=EDGE_CURVE('',#3750,#3748,#499,.T.);
#4727=EDGE_CURVE('',#3751,#3749,#500,.T.);
#4728=EDGE_CURVE('',#3752,#3753,#2236,.T.);
#4729=EDGE_CURVE('',#3752,#3750,#501,.T.);
#4730=EDGE_CURVE('',#3753,#3751,#502,.T.);
#4731=EDGE_CURVE('',#3754,#3755,#2237,.T.);
#4732=EDGE_CURVE('',#3754,#3752,#503,.T.);
#4733=EDGE_CURVE('',#3755,#3753,#504,.T.);
#4734=EDGE_CURVE('',#3756,#3757,#2238,.T.);
#4735=EDGE_CURVE('',#3756,#3754,#505,.T.);
#4736=EDGE_CURVE('',#3757,#3755,#506,.T.);
#4737=EDGE_CURVE('',#3758,#3759,#2239,.T.);
#4738=EDGE_CURVE('',#3758,#3756,#507,.T.);
#4739=EDGE_CURVE('',#3759,#3757,#508,.T.);
#4740=EDGE_CURVE('',#3760,#3761,#2240,.T.);
#4741=EDGE_CURVE('',#3760,#3758,#509,.T.);
#4742=EDGE_CURVE('',#3761,#3759,#510,.T.);
#4743=EDGE_CURVE('',#3762,#3763,#2241,.T.);
#4744=EDGE_CURVE('',#3762,#3760,#511,.T.);
#4745=EDGE_CURVE('',#3763,#3761,#512,.T.);
#4746=EDGE_CURVE('',#3764,#3765,#2242,.T.);
#4747=EDGE_CURVE('',#3764,#3762,#513,.T.);
#4748=EDGE_CURVE('',#3765,#3763,#514,.T.);
#4749=EDGE_CURVE('',#3766,#3767,#2243,.T.);
#4750=EDGE_CURVE('',#3766,#3764,#515,.T.);
#4751=EDGE_CURVE('',#3767,#3765,#516,.T.);
#4752=EDGE_CURVE('',#3768,#3769,#2244,.T.);
#4753=EDGE_CURVE('',#3768,#3766,#517,.T.);
#4754=EDGE_CURVE('',#3769,#3767,#518,.T.);
#4755=EDGE_CURVE('',#3770,#3771,#2245,.T.);
#4756=EDGE_CURVE('',#3770,#3768,#519,.T.);
#4757=EDGE_CURVE('',#3771,#3769,#520,.T.);
#4758=EDGE_CURVE('',#3772,#3773,#2246,.T.);
#4759=EDGE_CURVE('',#3772,#3770,#521,.T.);
#4760=EDGE_CURVE('',#3773,#3771,#522,.T.);
#4761=EDGE_CURVE('',#3774,#3775,#2247,.T.);
#4762=EDGE_CURVE('',#3774,#3772,#523,.T.);
#4763=EDGE_CURVE('',#3775,#3773,#524,.T.);
#4764=EDGE_CURVE('',#3776,#3777,#2248,.T.);
#4765=EDGE_CURVE('',#3776,#3774,#525,.T.);
#4766=EDGE_CURVE('',#3777,#3775,#526,.T.);
#4767=EDGE_CURVE('',#3778,#3779,#2249,.T.);
#4768=EDGE_CURVE('',#3778,#3776,#527,.T.);
#4769=EDGE_CURVE('',#3779,#3777,#528,.T.);
#4770=EDGE_CURVE('',#3780,#3781,#2250,.T.);
#4771=EDGE_CURVE('',#3780,#3778,#529,.T.);
#4772=EDGE_CURVE('',#3781,#3779,#530,.T.);
#4773=EDGE_CURVE('',#3782,#3783,#2251,.T.);
#4774=EDGE_CURVE('',#3782,#3780,#531,.T.);
#4775=EDGE_CURVE('',#3783,#3781,#532,.T.);
#4776=EDGE_CURVE('',#3784,#3785,#2252,.T.);
#4777=EDGE_CURVE('',#3784,#3782,#533,.T.);
#4778=EDGE_CURVE('',#3785,#3783,#534,.T.);
#4779=EDGE_CURVE('',#3786,#3787,#2253,.T.);
#4780=EDGE_CURVE('',#3786,#3784,#535,.T.);
#4781=EDGE_CURVE('',#3787,#3785,#536,.T.);
#4782=EDGE_CURVE('',#3788,#3789,#2254,.T.);
#4783=EDGE_CURVE('',#3788,#3786,#537,.T.);
#4784=EDGE_CURVE('',#3789,#3787,#538,.T.);
#4785=EDGE_CURVE('',#3790,#3791,#2255,.T.);
#4786=EDGE_CURVE('',#3790,#3788,#539,.T.);
#4787=EDGE_CURVE('',#3791,#3789,#540,.T.);
#4788=EDGE_CURVE('',#3792,#3793,#2256,.T.);
#4789=EDGE_CURVE('',#3792,#3790,#541,.T.);
#4790=EDGE_CURVE('',#3793,#3791,#542,.T.);
#4791=EDGE_CURVE('',#3794,#3795,#2257,.T.);
#4792=EDGE_CURVE('',#3794,#3792,#543,.T.);
#4793=EDGE_CURVE('',#3795,#3793,#544,.T.);
#4794=EDGE_CURVE('',#3796,#3797,#2258,.T.);
#4795=EDGE_CURVE('',#3796,#3794,#545,.T.);
#4796=EDGE_CURVE('',#3797,#3795,#546,.T.);
#4797=EDGE_CURVE('',#3798,#3799,#2259,.T.);
#4798=EDGE_CURVE('',#3798,#3796,#547,.T.);
#4799=EDGE_CURVE('',#3799,#3797,#548,.T.);
#4800=EDGE_CURVE('',#3800,#3801,#2260,.T.);
#4801=EDGE_CURVE('',#3800,#3798,#549,.T.);
#4802=EDGE_CURVE('',#3801,#3799,#550,.T.);
#4803=EDGE_CURVE('',#3802,#3803,#2261,.T.);
#4804=EDGE_CURVE('',#3802,#3800,#551,.T.);
#4805=EDGE_CURVE('',#3803,#3801,#552,.T.);
#4806=EDGE_CURVE('',#3804,#3805,#2262,.T.);
#4807=EDGE_CURVE('',#3804,#3802,#553,.T.);
#4808=EDGE_CURVE('',#3805,#3803,#554,.T.);
#4809=EDGE_CURVE('',#3806,#3807,#2263,.T.);
#4810=EDGE_CURVE('',#3806,#3804,#555,.T.);
#4811=EDGE_CURVE('',#3807,#3805,#556,.T.);
#4812=EDGE_CURVE('',#3808,#3809,#2264,.T.);
#4813=EDGE_CURVE('',#3808,#3806,#557,.T.);
#4814=EDGE_CURVE('',#3809,#3807,#558,.T.);
#4815=EDGE_CURVE('',#3810,#3811,#2265,.T.);
#4816=EDGE_CURVE('',#3810,#3808,#559,.T.);
#4817=EDGE_CURVE('',#3811,#3809,#560,.T.);
#4818=EDGE_CURVE('',#3812,#3813,#2266,.T.);
#4819=EDGE_CURVE('',#3812,#3810,#561,.T.);
#4820=EDGE_CURVE('',#3813,#3811,#562,.T.);
#4821=EDGE_CURVE('',#3814,#3815,#2267,.T.);
#4822=EDGE_CURVE('',#3814,#3812,#563,.T.);
#4823=EDGE_CURVE('',#3815,#3813,#564,.T.);
#4824=EDGE_CURVE('',#3816,#3817,#2268,.T.);
#4825=EDGE_CURVE('',#3816,#3814,#565,.T.);
#4826=EDGE_CURVE('',#3817,#3815,#566,.T.);
#4827=EDGE_CURVE('',#3818,#3819,#2269,.T.);
#4828=EDGE_CURVE('',#3818,#3816,#567,.T.);
#4829=EDGE_CURVE('',#3819,#3817,#568,.T.);
#4830=EDGE_CURVE('',#3820,#3821,#2270,.T.);
#4831=EDGE_CURVE('',#3820,#3818,#569,.T.);
#4832=EDGE_CURVE('',#3821,#3819,#570,.T.);
#4833=EDGE_CURVE('',#3822,#3823,#2271,.T.);
#4834=EDGE_CURVE('',#3822,#3820,#571,.T.);
#4835=EDGE_CURVE('',#3823,#3821,#572,.T.);
#4836=EDGE_CURVE('',#3824,#3825,#2272,.T.);
#4837=EDGE_CURVE('',#3824,#3822,#573,.T.);
#4838=EDGE_CURVE('',#3825,#3823,#574,.T.);
#4839=EDGE_CURVE('',#3826,#3827,#2273,.T.);
#4840=EDGE_CURVE('',#3826,#3824,#575,.T.);
#4841=EDGE_CURVE('',#3827,#3825,#576,.T.);
#4842=EDGE_CURVE('',#3828,#3829,#2274,.T.);
#4843=EDGE_CURVE('',#3828,#3826,#577,.T.);
#4844=EDGE_CURVE('',#3829,#3827,#578,.T.);
#4845=EDGE_CURVE('',#3830,#3831,#2275,.T.);
#4846=EDGE_CURVE('',#3830,#3828,#579,.T.);
#4847=EDGE_CURVE('',#3831,#3829,#580,.T.);
#4848=EDGE_CURVE('',#3832,#3833,#2276,.T.);
#4849=EDGE_CURVE('',#3832,#3830,#581,.T.);
#4850=EDGE_CURVE('',#3833,#3831,#582,.T.);
#4851=EDGE_CURVE('',#3834,#3835,#2277,.T.);
#4852=EDGE_CURVE('',#3834,#3832,#583,.T.);
#4853=EDGE_CURVE('',#3835,#3833,#584,.T.);
#4854=EDGE_CURVE('',#3836,#3837,#2278,.T.);
#4855=EDGE_CURVE('',#3836,#3834,#585,.T.);
#4856=EDGE_CURVE('',#3837,#3835,#586,.T.);
#4857=EDGE_CURVE('',#3838,#3839,#2279,.T.);
#4858=EDGE_CURVE('',#3838,#3836,#587,.T.);
#4859=EDGE_CURVE('',#3839,#3837,#588,.T.);
#4860=EDGE_CURVE('',#3840,#3841,#2280,.T.);
#4861=EDGE_CURVE('',#3840,#3838,#589,.T.);
#4862=EDGE_CURVE('',#3841,#3839,#590,.T.);
#4863=EDGE_CURVE('',#3842,#3843,#2281,.T.);
#4864=EDGE_CURVE('',#3842,#3840,#591,.T.);
#4865=EDGE_CURVE('',#3843,#3841,#592,.T.);
#4866=EDGE_CURVE('',#3844,#3844,#3324,.T.);
#4867=EDGE_CURVE('',#3844,#3845,#2282,.T.);
#4868=EDGE_CURVE('',#3845,#3845,#3325,.T.);
#4869=EDGE_CURVE('',#3846,#3846,#3326,.T.);
#4870=EDGE_CURVE('',#3846,#3847,#2283,.T.);
#4871=EDGE_CURVE('',#3847,#3847,#3327,.T.);
#4872=EDGE_CURVE('',#3848,#3848,#3328,.T.);
#4873=EDGE_CURVE('',#3848,#3849,#2284,.T.);
#4874=EDGE_CURVE('',#3849,#3849,#3329,.T.);
#4875=EDGE_CURVE('',#3850,#3850,#3330,.T.);
#4876=EDGE_CURVE('',#3850,#3851,#2285,.T.);
#4877=EDGE_CURVE('',#3851,#3851,#3331,.T.);
#4878=EDGE_CURVE('',#3852,#3852,#3332,.T.);
#4879=EDGE_CURVE('',#3852,#3853,#2286,.T.);
#4880=EDGE_CURVE('',#3853,#3853,#3333,.T.);
#4881=EDGE_CURVE('',#3854,#3854,#3334,.T.);
#4882=EDGE_CURVE('',#3854,#3855,#2287,.T.);
#4883=EDGE_CURVE('',#3855,#3855,#3335,.T.);
#4884=EDGE_CURVE('',#3856,#3856,#3336,.T.);
#4885=EDGE_CURVE('',#3857,#3467,#593,.T.);
#4886=EDGE_CURVE('',#3466,#3858,#594,.T.);
#4887=EDGE_CURVE('',#3858,#3857,#3337,.T.);
#4888=EDGE_CURVE('',#3856,#3859,#2288,.T.);
#4889=EDGE_CURVE('',#3859,#3859,#3338,.T.);
#4890=EDGE_CURVE('',#3860,#3657,#595,.T.);
#4891=EDGE_CURVE('',#3653,#3860,#596,.T.);
#4892=EDGE_CURVE('',#3857,#3843,#597,.T.);
#4893=EDGE_CURVE('',#3858,#3842,#598,.T.);
#4894=EDGE_CURVE('',#3656,#3861,#599,.T.);
#4895=EDGE_CURVE('',#3861,#3652,#600,.T.);
#4896=EDGE_CURVE('',#3861,#3860,#3339,.F.);
#4897=EDGE_CURVE('',#3862,#3862,#3340,.T.);
#4898=EDGE_CURVE('',#3862,#3863,#2289,.T.);
#4899=EDGE_CURVE('',#3863,#3863,#3341,.T.);
#4900=EDGE_CURVE('',#3864,#3864,#3342,.T.);
#4901=EDGE_CURVE('',#3864,#3865,#2290,.T.);
#4902=EDGE_CURVE('',#3865,#3865,#3343,.T.);
#4903=EDGE_CURVE('',#3866,#3867,#3344,.T.);
#4904=EDGE_CURVE('',#3868,#3866,#2291,.T.);
#4905=EDGE_CURVE('',#3869,#3868,#3345,.T.);
#4906=EDGE_CURVE('',#3867,#3869,#2292,.T.);
#4907=EDGE_CURVE('',#3868,#3870,#2293,.T.);
#4908=EDGE_CURVE('',#3870,#3871,#3346,.T.);
#4909=EDGE_CURVE('',#3871,#3872,#2294,.T.);
#4910=EDGE_CURVE('',#3872,#3873,#2295,.T.);
#4911=EDGE_CURVE('',#3873,#3874,#2296,.T.);
#4912=EDGE_CURVE('',#3874,#3875,#3347,.T.);
#4913=EDGE_CURVE('',#3875,#3869,#2297,.T.);
#4914=EDGE_CURVE('',#3876,#3866,#2298,.T.);
#4915=EDGE_CURVE('',#3870,#3876,#2299,.T.);
#4916=EDGE_CURVE('',#3877,#3877,#3348,.T.);
#4917=EDGE_CURVE('',#3877,#3878,#2300,.T.);
#4918=EDGE_CURVE('',#3878,#3878,#3349,.T.);
#4919=EDGE_CURVE('',#3879,#3880,#2301,.T.);
#4920=EDGE_CURVE('',#3881,#3879,#3350,.T.);
#4921=EDGE_CURVE('',#3882,#3881,#2302,.T.);
#4922=EDGE_CURVE('',#3882,#3880,#3351,.T.);
#4923=EDGE_CURVE('',#3880,#3883,#2303,.T.);
#4924=EDGE_CURVE('',#3884,#3883,#2304,.T.);
#4925=EDGE_CURVE('',#3884,#3879,#2305,.T.);
#4926=EDGE_CURVE('',#3882,#3885,#2306,.T.);
#4927=EDGE_CURVE('',#3886,#3885,#2307,.T.);
#4928=EDGE_CURVE('',#3887,#3886,#2308,.T.);
#4929=EDGE_CURVE('',#3888,#3887,#2309,.T.);
#4930=EDGE_CURVE('',#3888,#3883,#2310,.T.);
#4931=EDGE_CURVE('',#3881,#3889,#2311,.T.);
#4932=EDGE_CURVE('',#3885,#3889,#2312,.T.);
#4933=EDGE_CURVE('',#3889,#3890,#2313,.T.);
#4934=EDGE_CURVE('',#3890,#3886,#2314,.T.);
#4935=EDGE_CURVE('',#3873,#3884,#2315,.T.);
#4936=EDGE_CURVE('',#3872,#3890,#2316,.T.);
#4937=EDGE_CURVE('',#3891,#3888,#2317,.T.);
#4938=EDGE_CURVE('',#3874,#3891,#2318,.T.);
#4939=EDGE_CURVE('',#3892,#3871,#2319,.T.);
#4940=EDGE_CURVE('',#3887,#3892,#2320,.T.);
#4941=EDGE_CURVE('',#3867,#3893,#2321,.T.);
#4942=EDGE_CURVE('',#3891,#3893,#3352,.T.);
#4943=EDGE_CURVE('',#3876,#3892,#3353,.T.);
#4944=EDGE_CURVE('',#3893,#3875,#2322,.T.);
#4945=EDGE_CURVE('',#3894,#3894,#3354,.T.);
#4946=EDGE_CURVE('',#3894,#3895,#2323,.T.);
#4947=EDGE_CURVE('',#3895,#3895,#3355,.T.);
#4948=EDGE_CURVE('',#3896,#3897,#2324,.T.);
#4949=EDGE_CURVE('',#3896,#3898,#2325,.T.);
#4950=EDGE_CURVE('',#3899,#3898,#2326,.T.);
#4951=EDGE_CURVE('',#3897,#3899,#2327,.T.);
#4952=EDGE_CURVE('',#3897,#3900,#2328,.T.);
#4953=EDGE_CURVE('',#3901,#3899,#2329,.T.);
#4954=EDGE_CURVE('',#3900,#3901,#2330,.T.);
#4955=EDGE_CURVE('',#3900,#3902,#2331,.T.);
#4956=EDGE_CURVE('',#3903,#3901,#2332,.T.);
#4957=EDGE_CURVE('',#3902,#3903,#2333,.T.);
#4958=EDGE_CURVE('',#3902,#3896,#2334,.T.);
#4959=EDGE_CURVE('',#3898,#3903,#2335,.T.);
#4960=EDGE_CURVE('',#3904,#3904,#3356,.T.);
#4961=EDGE_CURVE('',#3904,#3905,#2336,.T.);
#4962=EDGE_CURVE('',#3905,#3905,#3357,.T.);
#4963=EDGE_CURVE('',#3906,#3907,#2337,.T.);
#4964=EDGE_CURVE('',#3906,#3908,#2338,.T.);
#4965=EDGE_CURVE('',#3909,#3908,#2339,.T.);
#4966=EDGE_CURVE('',#3907,#3909,#2340,.T.);
#4967=EDGE_CURVE('',#3907,#3910,#2341,.T.);
#4968=EDGE_CURVE('',#3911,#3909,#2342,.T.);
#4969=EDGE_CURVE('',#3910,#3911,#2343,.T.);
#4970=EDGE_CURVE('',#3910,#3912,#2344,.T.);
#4971=EDGE_CURVE('',#3913,#3911,#2345,.T.);
#4972=EDGE_CURVE('',#3912,#3913,#2346,.T.);
#4973=EDGE_CURVE('',#3912,#3906,#2347,.T.);
#4974=EDGE_CURVE('',#3908,#3913,#2348,.T.);
#4975=EDGE_CURVE('',#3914,#3915,#2349,.T.);
#4976=EDGE_CURVE('',#3916,#3914,#3358,.T.);
#4977=EDGE_CURVE('',#3917,#3916,#2350,.T.);
#4978=EDGE_CURVE('',#3915,#3917,#3359,.T.);
#4979=EDGE_CURVE('',#3914,#3918,#2351,.T.);
#4980=EDGE_CURVE('',#3918,#3919,#3360,.T.);
#4981=EDGE_CURVE('',#3919,#3916,#2352,.T.);
#4982=EDGE_CURVE('',#3920,#3915,#2353,.T.);
#4983=EDGE_CURVE('',#3918,#3920,#2354,.T.);
#4984=EDGE_CURVE('',#3921,#3919,#2355,.T.);
#4985=EDGE_CURVE('',#3917,#3921,#2356,.T.);
#4986=EDGE_CURVE('',#3920,#3921,#3361,.T.);
#4987=EDGE_CURVE('',#3922,#3922,#3362,.T.);
#4988=EDGE_CURVE('',#3922,#3923,#2357,.T.);
#4989=EDGE_CURVE('',#3923,#3923,#3363,.T.);
#4990=EDGE_CURVE('',#3924,#3925,#2358,.T.);
#4991=EDGE_CURVE('',#3924,#3926,#2359,.T.);
#4992=EDGE_CURVE('',#3927,#3926,#2360,.T.);
#4993=EDGE_CURVE('',#3925,#3927,#2361,.T.);
#4994=EDGE_CURVE('',#3925,#3928,#2362,.T.);
#4995=EDGE_CURVE('',#3929,#3927,#2363,.T.);
#4996=EDGE_CURVE('',#3928,#3929,#2364,.T.);
#4997=EDGE_CURVE('',#3928,#3930,#2365,.T.);
#4998=EDGE_CURVE('',#3931,#3929,#2366,.T.);
#4999=EDGE_CURVE('',#3930,#3931,#2367,.T.);
#5000=EDGE_CURVE('',#3930,#3924,#2368,.T.);
#5001=EDGE_CURVE('',#3926,#3931,#2369,.T.);
#5002=EDGE_CURVE('',#3932,#3932,#3364,.T.);
#5003=EDGE_CURVE('',#3932,#3933,#2370,.T.);
#5004=EDGE_CURVE('',#3933,#3933,#3365,.T.);
#5005=EDGE_CURVE('',#3934,#3935,#2371,.T.);
#5006=EDGE_CURVE('',#3934,#3936,#2372,.T.);
#5007=EDGE_CURVE('',#3937,#3936,#2373,.T.);
#5008=EDGE_CURVE('',#3935,#3937,#2374,.T.);
#5009=EDGE_CURVE('',#3935,#3938,#2375,.T.);
#5010=EDGE_CURVE('',#3939,#3937,#2376,.T.);
#5011=EDGE_CURVE('',#3938,#3939,#2377,.T.);
#5012=EDGE_CURVE('',#3938,#3940,#2378,.T.);
#5013=EDGE_CURVE('',#3941,#3939,#2379,.T.);
#5014=EDGE_CURVE('',#3940,#3941,#2380,.T.);
#5015=EDGE_CURVE('',#3940,#3934,#2381,.T.);
#5016=EDGE_CURVE('',#3936,#3941,#2382,.T.);
#5017=EDGE_CURVE('',#3942,#3943,#2383,.T.);
#5018=EDGE_CURVE('',#3944,#3942,#2384,.T.);
#5019=EDGE_CURVE('',#3945,#3944,#2385,.T.);
#5020=EDGE_CURVE('',#3943,#3945,#2386,.T.);
#5021=EDGE_CURVE('',#3946,#3947,#2387,.T.);
#5022=EDGE_CURVE('',#3948,#3946,#2388,.T.);
#5023=EDGE_CURVE('',#3949,#3948,#2389,.T.);
#5024=EDGE_CURVE('',#3947,#3949,#2390,.T.);
#5025=EDGE_CURVE('',#3943,#3946,#3366,.T.);
#5026=EDGE_CURVE('',#3948,#3945,#3367,.T.);
#5027=EDGE_CURVE('',#3949,#3944,#3368,.T.);
#5028=EDGE_CURVE('',#3942,#3947,#3369,.T.);
#5029=EDGE_CURVE('',#3950,#3951,#2391,.T.);
#5030=EDGE_CURVE('',#3952,#3950,#2392,.T.);
#5031=EDGE_CURVE('',#3953,#3952,#2393,.T.);
#5032=EDGE_CURVE('',#3951,#3953,#2394,.T.);
#5033=EDGE_CURVE('',#3954,#3955,#2395,.T.);
#5034=EDGE_CURVE('',#3956,#3954,#2396,.T.);
#5035=EDGE_CURVE('',#3957,#3956,#2397,.T.);
#5036=EDGE_CURVE('',#3955,#3957,#2398,.T.);
#5037=EDGE_CURVE('',#3951,#3954,#3370,.T.);
#5038=EDGE_CURVE('',#3956,#3953,#3371,.T.);
#5039=EDGE_CURVE('',#3957,#3952,#3372,.T.);
#5040=EDGE_CURVE('',#3950,#3955,#3373,.T.);
#5041=EDGE_CURVE('',#3958,#3959,#2399,.T.);
#5042=EDGE_CURVE('',#3958,#3960,#3374,.T.);
#5043=EDGE_CURVE('',#3961,#3960,#2400,.T.);
#5044=EDGE_CURVE('',#3962,#3961,#3375,.T.);
#5045=EDGE_CURVE('',#3963,#3962,#2401,.T.);
#5046=EDGE_CURVE('',#3964,#3963,#3376,.T.);
#5047=EDGE_CURVE('',#3965,#3964,#2402,.T.);
#5048=EDGE_CURVE('',#3959,#3965,#3377,.T.);
#5049=EDGE_CURVE('',#3966,#3958,#2403,.T.);
#5050=EDGE_CURVE('',#3967,#3966,#2404,.T.);
#5051=EDGE_CURVE('',#3960,#3967,#2405,.T.);
#5052=EDGE_CURVE('',#3963,#3968,#2406,.T.);
#5053=EDGE_CURVE('',#3969,#3968,#3378,.T.);
#5054=EDGE_CURVE('',#3969,#3964,#2407,.T.);
#5055=EDGE_CURVE('',#3970,#3962,#2408,.T.);
#5056=EDGE_CURVE('',#3968,#3970,#2409,.T.);
#5057=EDGE_CURVE('',#3967,#3971,#2410,.T.);
#5058=EDGE_CURVE('',#3971,#3972,#2411,.T.);
#5059=EDGE_CURVE('',#3973,#3972,#2412,.T.);
#5060=EDGE_CURVE('',#3961,#3973,#2413,.T.);
#5061=EDGE_CURVE('',#3974,#3974,#3379,.T.);
#5062=EDGE_CURVE('',#3974,#3975,#2414,.T.);
#5063=EDGE_CURVE('',#3975,#3975,#3380,.T.);
#5064=EDGE_CURVE('',#3976,#3977,#2415,.T.);
#5065=EDGE_CURVE('',#3978,#3976,#3381,.T.);
#5066=EDGE_CURVE('',#3979,#3978,#2416,.T.);
#5067=EDGE_CURVE('',#3979,#3977,#3382,.T.);
#5068=EDGE_CURVE('',#3977,#3972,#2417,.T.);
#5069=EDGE_CURVE('',#3971,#3976,#2418,.T.);
#5070=EDGE_CURVE('',#3979,#3980,#2419,.T.);
#5071=EDGE_CURVE('',#3981,#3980,#2420,.T.);
#5072=EDGE_CURVE('',#3982,#3981,#2421,.T.);
#5073=EDGE_CURVE('',#3973,#3982,#2422,.T.);
#5074=EDGE_CURVE('',#3978,#3983,#2423,.T.);
#5075=EDGE_CURVE('',#3980,#3983,#2424,.T.);
#5076=EDGE_CURVE('',#3983,#3984,#2425,.T.);
#5077=EDGE_CURVE('',#3984,#3981,#2426,.T.);
#5078=EDGE_CURVE('',#3966,#3984,#2427,.T.);
#5079=EDGE_CURVE('',#3982,#3959,#2428,.T.);
#5080=EDGE_CURVE('',#3985,#3969,#2429,.T.);
#5081=EDGE_CURVE('',#3965,#3985,#2430,.T.);
#5082=EDGE_CURVE('',#3985,#3970,#3383,.T.);
#5083=EDGE_CURVE('',#3986,#3986,#3384,.T.);
#5084=EDGE_CURVE('',#3986,#3987,#2431,.T.);
#5085=EDGE_CURVE('',#3987,#3987,#3385,.T.);
#5086=EDGE_CURVE('',#3988,#3989,#2432,.T.);
#5087=EDGE_CURVE('',#3988,#3990,#2433,.T.);
#5088=EDGE_CURVE('',#3991,#3990,#2434,.T.);
#5089=EDGE_CURVE('',#3989,#3991,#2435,.T.);
#5090=EDGE_CURVE('',#3989,#3992,#2436,.T.);
#5091=EDGE_CURVE('',#3993,#3991,#2437,.T.);
#5092=EDGE_CURVE('',#3992,#3993,#2438,.T.);
#5093=EDGE_CURVE('',#3992,#3994,#2439,.T.);
#5094=EDGE_CURVE('',#3995,#3993,#2440,.T.);
#5095=EDGE_CURVE('',#3994,#3995,#2441,.T.);
#5096=EDGE_CURVE('',#3994,#3988,#2442,.T.);
#5097=EDGE_CURVE('',#3990,#3995,#2443,.T.);
#5098=EDGE_CURVE('',#3996,#3996,#3386,.T.);
#5099=EDGE_CURVE('',#3996,#3997,#2444,.T.);
#5100=EDGE_CURVE('',#3997,#3997,#3387,.T.);
#5101=EDGE_CURVE('',#3998,#3999,#2445,.T.);
#5102=EDGE_CURVE('',#3998,#4000,#2446,.T.);
#5103=EDGE_CURVE('',#4001,#4000,#2447,.T.);
#5104=EDGE_CURVE('',#3999,#4001,#2448,.T.);
#5105=EDGE_CURVE('',#3999,#4002,#2449,.T.);
#5106=EDGE_CURVE('',#4003,#4001,#2450,.T.);
#5107=EDGE_CURVE('',#4002,#4003,#2451,.T.);
#5108=EDGE_CURVE('',#4002,#4004,#2452,.T.);
#5109=EDGE_CURVE('',#4005,#4003,#2453,.T.);
#5110=EDGE_CURVE('',#4004,#4005,#2454,.T.);
#5111=EDGE_CURVE('',#4004,#3998,#2455,.T.);
#5112=EDGE_CURVE('',#4000,#4005,#2456,.T.);
#5113=EDGE_CURVE('',#4006,#4007,#2457,.T.);
#5114=EDGE_CURVE('',#4008,#4006,#3388,.T.);
#5115=EDGE_CURVE('',#4009,#4008,#2458,.T.);
#5116=EDGE_CURVE('',#4007,#4009,#3389,.T.);
#5117=EDGE_CURVE('',#4006,#4010,#2459,.T.);
#5118=EDGE_CURVE('',#4010,#4011,#3390,.T.);
#5119=EDGE_CURVE('',#4011,#4008,#2460,.T.);
#5120=EDGE_CURVE('',#4012,#4007,#2461,.T.);
#5121=EDGE_CURVE('',#4010,#4012,#2462,.T.);
#5122=EDGE_CURVE('',#4013,#4011,#2463,.T.);
#5123=EDGE_CURVE('',#4009,#4013,#2464,.T.);
#5124=EDGE_CURVE('',#4012,#4013,#3391,.T.);
#5125=EDGE_CURVE('',#4014,#4014,#3392,.T.);
#5126=EDGE_CURVE('',#4014,#4015,#2465,.T.);
#5127=EDGE_CURVE('',#4015,#4015,#3393,.T.);
#5128=EDGE_CURVE('',#4016,#4017,#2466,.T.);
#5129=EDGE_CURVE('',#4016,#4018,#2467,.T.);
#5130=EDGE_CURVE('',#4019,#4018,#2468,.T.);
#5131=EDGE_CURVE('',#4017,#4019,#2469,.T.);
#5132=EDGE_CURVE('',#4017,#4020,#2470,.T.);
#5133=EDGE_CURVE('',#4021,#4019,#2471,.T.);
#5134=EDGE_CURVE('',#4020,#4021,#2472,.T.);
#5135=EDGE_CURVE('',#4020,#4022,#2473,.T.);
#5136=EDGE_CURVE('',#4023,#4021,#2474,.T.);
#5137=EDGE_CURVE('',#4022,#4023,#2475,.T.);
#5138=EDGE_CURVE('',#4022,#4016,#2476,.T.);
#5139=EDGE_CURVE('',#4018,#4023,#2477,.T.);
#5140=EDGE_CURVE('',#4024,#4024,#3394,.T.);
#5141=EDGE_CURVE('',#4024,#4025,#2478,.T.);
#5142=EDGE_CURVE('',#4025,#4025,#3395,.T.);
#5143=EDGE_CURVE('',#4026,#4027,#2479,.T.);
#5144=EDGE_CURVE('',#4026,#4028,#2480,.T.);
#5145=EDGE_CURVE('',#4029,#4028,#2481,.T.);
#5146=EDGE_CURVE('',#4027,#4029,#2482,.T.);
#5147=EDGE_CURVE('',#4027,#4030,#2483,.T.);
#5148=EDGE_CURVE('',#4031,#4029,#2484,.T.);
#5149=EDGE_CURVE('',#4030,#4031,#2485,.T.);
#5150=EDGE_CURVE('',#4030,#4032,#2486,.T.);
#5151=EDGE_CURVE('',#4033,#4031,#2487,.T.);
#5152=EDGE_CURVE('',#4032,#4033,#2488,.T.);
#5153=EDGE_CURVE('',#4032,#4026,#2489,.T.);
#5154=EDGE_CURVE('',#4028,#4033,#2490,.T.);
#5155=EDGE_CURVE('',#4034,#4035,#2491,.T.);
#5156=EDGE_CURVE('',#4036,#4034,#2492,.T.);
#5157=EDGE_CURVE('',#4037,#4036,#2493,.T.);
#5158=EDGE_CURVE('',#4035,#4037,#2494,.T.);
#5159=EDGE_CURVE('',#4038,#4039,#2495,.T.);
#5160=EDGE_CURVE('',#4040,#4038,#2496,.T.);
#5161=EDGE_CURVE('',#4041,#4040,#2497,.T.);
#5162=EDGE_CURVE('',#4039,#4041,#2498,.T.);
#5163=EDGE_CURVE('',#4035,#4038,#3396,.T.);
#5164=EDGE_CURVE('',#4040,#4037,#3397,.T.);
#5165=EDGE_CURVE('',#4041,#4036,#3398,.T.);
#5166=EDGE_CURVE('',#4034,#4039,#3399,.T.);
#5167=EDGE_CURVE('',#4042,#4043,#2499,.T.);
#5168=EDGE_CURVE('',#4044,#4042,#2500,.T.);
#5169=EDGE_CURVE('',#4045,#4044,#2501,.T.);
#5170=EDGE_CURVE('',#4043,#4045,#2502,.T.);
#5171=EDGE_CURVE('',#4046,#4047,#2503,.T.);
#5172=EDGE_CURVE('',#4048,#4046,#2504,.T.);
#5173=EDGE_CURVE('',#4049,#4048,#2505,.T.);
#5174=EDGE_CURVE('',#4047,#4049,#2506,.T.);
#5175=EDGE_CURVE('',#4043,#4046,#3400,.T.);
#5176=EDGE_CURVE('',#4048,#4045,#3401,.T.);
#5177=EDGE_CURVE('',#4049,#4044,#3402,.T.);
#5178=EDGE_CURVE('',#4042,#4047,#3403,.T.);
#5179=EDGE_CURVE('',#4050,#4051,#2507,.T.);
#5180=EDGE_CURVE('',#4051,#4052,#2508,.T.);
#5181=EDGE_CURVE('',#4053,#4052,#2509,.T.);
#5182=EDGE_CURVE('',#4050,#4053,#2510,.T.);
#5183=EDGE_CURVE('',#4054,#4050,#2511,.T.);
#5184=EDGE_CURVE('',#4055,#4053,#2512,.T.);
#5185=EDGE_CURVE('',#4054,#4055,#2513,.T.);
#5186=EDGE_CURVE('',#4056,#4054,#2514,.T.);
#5187=EDGE_CURVE('',#4057,#4055,#2515,.T.);
#5188=EDGE_CURVE('',#4056,#4057,#2516,.T.);
#5189=EDGE_CURVE('',#4051,#4056,#2517,.T.);
#5190=EDGE_CURVE('',#4052,#4057,#2518,.T.);
#5191=EDGE_CURVE('',#4058,#4059,#2519,.T.);
#5192=EDGE_CURVE('',#4059,#4060,#2520,.T.);
#5193=EDGE_CURVE('',#4061,#4060,#2521,.T.);
#5194=EDGE_CURVE('',#4058,#4061,#2522,.T.);
#5195=EDGE_CURVE('',#4062,#4058,#2523,.T.);
#5196=EDGE_CURVE('',#4063,#4061,#2524,.T.);
#5197=EDGE_CURVE('',#4062,#4063,#2525,.T.);
#5198=EDGE_CURVE('',#4064,#4062,#2526,.T.);
#5199=EDGE_CURVE('',#4065,#4063,#2527,.T.);
#5200=EDGE_CURVE('',#4064,#4065,#2528,.T.);
#5201=EDGE_CURVE('',#4059,#4064,#2529,.T.);
#5202=EDGE_CURVE('',#4060,#4065,#2530,.T.);
#5203=EDGE_CURVE('',#4066,#4067,#2531,.T.);
#5204=EDGE_CURVE('',#4067,#4068,#2532,.T.);
#5205=EDGE_CURVE('',#4068,#4069,#2533,.T.);
#5206=EDGE_CURVE('',#4066,#4069,#2534,.T.);
#5207=EDGE_CURVE('',#4067,#4070,#2535,.T.);
#5208=EDGE_CURVE('',#4070,#4071,#2536,.T.);
#5209=EDGE_CURVE('',#4071,#4068,#2537,.T.);
#5210=EDGE_CURVE('',#4070,#4072,#2538,.T.);
#5211=EDGE_CURVE('',#4072,#4073,#2539,.T.);
#5212=EDGE_CURVE('',#4073,#4071,#2540,.T.);
#5213=EDGE_CURVE('',#4072,#4074,#2541,.T.);
#5214=EDGE_CURVE('',#4074,#4075,#2542,.T.);
#5215=EDGE_CURVE('',#4075,#4073,#2543,.T.);
#5216=EDGE_CURVE('',#4074,#4076,#2544,.T.);
#5217=EDGE_CURVE('',#4076,#4077,#2545,.T.);
#5218=EDGE_CURVE('',#4077,#4075,#2546,.T.);
#5219=EDGE_CURVE('',#4076,#4066,#2547,.T.);
#5220=EDGE_CURVE('',#4069,#4077,#2548,.T.);
#5221=EDGE_CURVE('',#4078,#4078,#3404,.T.);
#5222=EDGE_CURVE('',#4079,#4079,#3405,.T.);
#5223=EDGE_CURVE('',#4080,#4080,#3406,.T.);
#5224=EDGE_CURVE('',#4080,#4079,#2549,.T.);
#5225=EDGE_CURVE('',#4081,#4081,#3407,.T.);
#5226=EDGE_CURVE('',#4081,#4080,#2550,.T.);
#5227=EDGE_CURVE('',#4082,#4082,#3408,.T.);
#5228=EDGE_CURVE('',#4082,#4081,#2551,.T.);
#5229=EDGE_CURVE('',#4083,#4083,#3409,.T.);
#5230=EDGE_CURVE('',#4084,#4084,#3410,.F.);
#5231=EDGE_CURVE('',#4084,#4083,#2552,.T.);
#5232=EDGE_CURVE('',#4078,#4084,#2553,.T.);
#5233=EDGE_CURVE('',#4085,#4086,#2554,.T.);
#5234=EDGE_CURVE('',#4086,#4087,#2555,.T.);
#5235=EDGE_CURVE('',#4087,#4088,#2556,.T.);
#5236=EDGE_CURVE('',#4085,#4088,#2557,.T.);
#5237=EDGE_CURVE('',#4086,#4089,#2558,.T.);
#5238=EDGE_CURVE('',#4089,#4090,#2559,.T.);
#5239=EDGE_CURVE('',#4090,#4087,#2560,.T.);
#5240=EDGE_CURVE('',#4089,#4091,#2561,.T.);
#5241=EDGE_CURVE('',#4091,#4092,#2562,.T.);
#5242=EDGE_CURVE('',#4092,#4090,#2563,.T.);
#5243=EDGE_CURVE('',#4091,#4093,#2564,.T.);
#5244=EDGE_CURVE('',#4093,#4094,#2565,.T.);
#5245=EDGE_CURVE('',#4094,#4092,#2566,.T.);
#5246=EDGE_CURVE('',#4093,#4095,#2567,.T.);
#5247=EDGE_CURVE('',#4095,#4096,#2568,.T.);
#5248=EDGE_CURVE('',#4096,#4094,#2569,.T.);
#5249=EDGE_CURVE('',#4095,#4085,#2570,.T.);
#5250=EDGE_CURVE('',#4088,#4096,#2571,.T.);
#5251=EDGE_CURVE('',#4097,#4097,#3411,.T.);
#5252=EDGE_CURVE('',#4098,#4098,#3412,.T.);
#5253=EDGE_CURVE('',#4097,#4099,#2572,.T.);
#5254=EDGE_CURVE('',#4099,#4099,#3413,.T.);
#5255=EDGE_CURVE('',#4100,#4100,#3414,.T.);
#5256=EDGE_CURVE('',#4101,#4101,#3415,.T.);
#5257=EDGE_CURVE('',#4101,#4100,#2573,.T.);
#5258=EDGE_CURVE('',#4102,#4102,#3416,.T.);
#5259=EDGE_CURVE('',#4102,#4101,#2574,.T.);
#5260=EDGE_CURVE('',#4103,#4103,#3417,.T.);
#5261=EDGE_CURVE('',#4103,#4102,#2575,.T.);
#5262=EDGE_CURVE('',#4104,#4104,#3418,.T.);
#5263=EDGE_CURVE('',#4105,#4105,#3419,.F.);
#5264=EDGE_CURVE('',#4105,#4104,#2576,.T.);
#5265=EDGE_CURVE('',#4098,#4105,#2577,.T.);
#5266=EDGE_CURVE('',#4106,#4106,#3420,.T.);
#5267=EDGE_CURVE('',#4106,#4107,#2578,.T.);
#5268=EDGE_CURVE('',#4107,#4107,#3421,.T.);
#5269=EDGE_CURVE('',#4108,#4108,#3422,.T.);
#5270=EDGE_CURVE('',#4108,#4109,#2579,.T.);
#5271=EDGE_CURVE('',#4109,#4109,#3423,.T.);
#5272=EDGE_CURVE('',#4110,#4111,#183,.T.);
#5273=EDGE_CURVE('',#4112,#4110,#184,.T.);
#5274=EDGE_CURVE('',#4112,#4113,#2580,.T.);
#5275=EDGE_CURVE('',#4113,#4113,#3424,.T.);
#5276=EDGE_CURVE('',#4114,#4112,#185,.T.);
#5277=EDGE_CURVE('',#4115,#4114,#186,.T.);
#5278=EDGE_CURVE('',#4116,#4115,#187,.T.);
#5279=EDGE_CURVE('',#4111,#4116,#188,.T.);
#5280=EDGE_CURVE('',#4117,#4117,#3425,.T.);
#5281=EDGE_CURVE('',#4117,#4118,#2581,.T.);
#5282=EDGE_CURVE('',#4119,#4118,#189,.T.);
#5283=EDGE_CURVE('',#4120,#4119,#190,.T.);
#5284=EDGE_CURVE('',#4121,#4120,#191,.T.);
#5285=EDGE_CURVE('',#4122,#4121,#192,.T.);
#5286=EDGE_CURVE('',#4123,#4122,#193,.T.);
#5287=EDGE_CURVE('',#4118,#4123,#194,.T.);
#5288=EDGE_CURVE('',#4114,#4123,#2582,.T.);
#5289=EDGE_CURVE('',#4115,#4122,#2583,.T.);
#5290=EDGE_CURVE('',#4112,#4118,#2584,.T.);
#5291=EDGE_CURVE('',#4110,#4119,#2585,.T.);
#5292=EDGE_CURVE('',#4124,#4124,#3426,.F.);
#5293=EDGE_CURVE('',#4124,#4125,#2586,.T.);
#5294=EDGE_CURVE('',#4125,#4125,#3427,.F.);
#5295=EDGE_CURVE('',#4111,#4120,#2587,.T.);
#5296=EDGE_CURVE('',#4116,#4121,#2588,.T.);
#5297=EDGE_CURVE('',#4126,#4127,#2589,.T.);
#5298=EDGE_CURVE('',#4127,#4128,#601,.T.);
#5299=EDGE_CURVE('',#4129,#4128,#3428,.T.);
#5300=EDGE_CURVE('',#4129,#4126,#602,.T.);
#5301=EDGE_CURVE('',#4130,#4131,#2590,.T.);
#5302=EDGE_CURVE('',#4131,#4127,#603,.T.);
#5303=EDGE_CURVE('',#4126,#4130,#604,.T.);
#5304=EDGE_CURVE('',#4132,#4133,#2591,.T.);
#5305=EDGE_CURVE('',#4133,#4131,#605,.T.);
#5306=EDGE_CURVE('',#4130,#4132,#606,.T.);
#5307=EDGE_CURVE('',#4134,#4135,#2592,.T.);
#5308=EDGE_CURVE('',#4134,#4136,#607,.T.);
#5309=EDGE_CURVE('',#4137,#4136,#3429,.F.);
#5310=EDGE_CURVE('',#4137,#4135,#608,.T.);
#5311=EDGE_CURVE('',#4138,#4139,#2593,.T.);
#5312=EDGE_CURVE('',#4139,#4140,#609,.T.);
#5313=EDGE_CURVE('',#4141,#4140,#3430,.T.);
#5314=EDGE_CURVE('',#4138,#4141,#610,.T.);
#5315=EDGE_CURVE('',#4142,#4143,#2594,.T.);
#5316=EDGE_CURVE('',#4143,#4139,#611,.T.);
#5317=EDGE_CURVE('',#4142,#4138,#612,.T.);
#5318=EDGE_CURVE('',#4144,#4145,#2595,.T.);
#5319=EDGE_CURVE('',#4145,#4143,#613,.T.);
#5320=EDGE_CURVE('',#4144,#4142,#614,.T.);
#5321=EDGE_CURVE('',#4146,#4147,#2596,.T.);
#5322=EDGE_CURVE('',#4148,#4146,#615,.T.);
#5323=EDGE_CURVE('',#4149,#4148,#3431,.T.);
#5324=EDGE_CURVE('',#4149,#4147,#616,.T.);
#5325=EDGE_CURVE('',#4147,#4145,#617,.T.);
#5326=EDGE_CURVE('',#4146,#4144,#618,.T.);
#5327=EDGE_CURVE('',#4140,#4129,#619,.T.);
#5328=EDGE_CURVE('',#4136,#4149,#620,.T.);
#5329=EDGE_CURVE('',#4132,#4134,#621,.T.);
#5330=EDGE_CURVE('',#4128,#4141,#622,.T.);
#5331=EDGE_CURVE('',#4135,#4133,#623,.T.);
#5332=EDGE_CURVE('',#4148,#4137,#624,.T.);
#5333=EDGE_CURVE('',#4150,#4151,#2597,.T.);
#5334=EDGE_CURVE('',#4151,#4152,#2598,.T.);
#5335=EDGE_CURVE('',#4152,#4153,#2599,.T.);
#5336=EDGE_CURVE('',#4153,#4154,#2600,.T.);
#5337=EDGE_CURVE('',#4154,#4155,#2601,.T.);
#5338=EDGE_CURVE('',#4155,#4150,#2602,.T.);
#5339=EDGE_CURVE('',#4156,#4157,#2603,.T.);
#5340=EDGE_CURVE('',#4157,#4150,#2604,.T.);
#5341=EDGE_CURVE('',#4156,#4155,#2605,.T.);
#5342=EDGE_CURVE('',#4158,#4156,#2606,.T.);
#5343=EDGE_CURVE('',#4158,#4154,#2607,.T.);
#5344=EDGE_CURVE('',#4159,#4158,#2608,.T.);
#5345=EDGE_CURVE('',#4159,#4153,#2609,.T.);
#5346=EDGE_CURVE('',#4160,#4159,#2610,.T.);
#5347=EDGE_CURVE('',#4160,#4152,#2611,.T.);
#5348=EDGE_CURVE('',#4161,#4160,#2612,.T.);
#5349=EDGE_CURVE('',#4161,#4151,#2613,.T.);
#5350=EDGE_CURVE('',#4157,#4161,#2614,.T.);
#5351=EDGE_CURVE('',#4162,#4163,#2615,.T.);
#5352=EDGE_CURVE('',#4163,#4164,#625,.T.);
#5353=EDGE_CURVE('',#4165,#4164,#3432,.T.);
#5354=EDGE_CURVE('',#4165,#4162,#626,.T.);
#5355=EDGE_CURVE('',#4166,#4167,#2616,.T.);
#5356=EDGE_CURVE('',#4167,#4163,#627,.T.);
#5357=EDGE_CURVE('',#4162,#4166,#628,.T.);
#5358=EDGE_CURVE('',#4168,#4169,#2617,.T.);
#5359=EDGE_CURVE('',#4169,#4167,#629,.T.);
#5360=EDGE_CURVE('',#4166,#4168,#630,.T.);
#5361=EDGE_CURVE('',#4170,#4171,#2618,.T.);
#5362=EDGE_CURVE('',#4170,#4172,#631,.T.);
#5363=EDGE_CURVE('',#4173,#4172,#3433,.F.);
#5364=EDGE_CURVE('',#4173,#4171,#632,.T.);
#5365=EDGE_CURVE('',#4174,#4175,#2619,.T.);
#5366=EDGE_CURVE('',#4175,#4176,#633,.T.);
#5367=EDGE_CURVE('',#4177,#4176,#3434,.T.);
#5368=EDGE_CURVE('',#4174,#4177,#634,.T.);
#5369=EDGE_CURVE('',#4178,#4179,#2620,.T.);
#5370=EDGE_CURVE('',#4179,#4175,#635,.T.);
#5371=EDGE_CURVE('',#4178,#4174,#636,.T.);
#5372=EDGE_CURVE('',#4180,#4181,#2621,.T.);
#5373=EDGE_CURVE('',#4181,#4179,#637,.T.);
#5374=EDGE_CURVE('',#4180,#4178,#638,.T.);
#5375=EDGE_CURVE('',#4182,#4183,#2622,.T.);
#5376=EDGE_CURVE('',#4184,#4182,#639,.T.);
#5377=EDGE_CURVE('',#4185,#4184,#3435,.T.);
#5378=EDGE_CURVE('',#4185,#4183,#640,.T.);
#5379=EDGE_CURVE('',#4183,#4181,#641,.T.);
#5380=EDGE_CURVE('',#4182,#4180,#642,.T.);
#5381=EDGE_CURVE('',#4176,#4165,#643,.T.);
#5382=EDGE_CURVE('',#4172,#4185,#644,.T.);
#5383=EDGE_CURVE('',#4168,#4170,#645,.T.);
#5384=EDGE_CURVE('',#4164,#4177,#646,.T.);
#5385=EDGE_CURVE('',#4171,#4169,#647,.T.);
#5386=EDGE_CURVE('',#4184,#4173,#648,.T.);
#5387=EDGE_CURVE('',#4186,#4187,#2623,.T.);
#5388=EDGE_CURVE('',#4187,#4188,#2624,.T.);
#5389=EDGE_CURVE('',#4188,#4189,#2625,.T.);
#5390=EDGE_CURVE('',#4189,#4190,#2626,.T.);
#5391=EDGE_CURVE('',#4190,#4191,#2627,.T.);
#5392=EDGE_CURVE('',#4191,#4186,#2628,.T.);
#5393=EDGE_CURVE('',#4192,#4193,#2629,.T.);
#5394=EDGE_CURVE('',#4193,#4186,#2630,.T.);
#5395=EDGE_CURVE('',#4192,#4191,#2631,.T.);
#5396=EDGE_CURVE('',#4194,#4192,#2632,.T.);
#5397=EDGE_CURVE('',#4194,#4190,#2633,.T.);
#5398=EDGE_CURVE('',#4195,#4194,#2634,.T.);
#5399=EDGE_CURVE('',#4195,#4189,#2635,.T.);
#5400=EDGE_CURVE('',#4196,#4195,#2636,.T.);
#5401=EDGE_CURVE('',#4196,#4188,#2637,.T.);
#5402=EDGE_CURVE('',#4197,#4196,#2638,.T.);
#5403=EDGE_CURVE('',#4197,#4187,#2639,.T.);
#5404=EDGE_CURVE('',#4193,#4197,#2640,.T.);
#5405=EDGE_CURVE('',#4198,#4199,#2641,.T.);
#5406=EDGE_CURVE('',#4199,#4200,#649,.T.);
#5407=EDGE_CURVE('',#4201,#4200,#3436,.T.);
#5408=EDGE_CURVE('',#4201,#4198,#650,.T.);
#5409=EDGE_CURVE('',#4202,#4203,#2642,.T.);
#5410=EDGE_CURVE('',#4203,#4199,#651,.T.);
#5411=EDGE_CURVE('',#4198,#4202,#652,.T.);
#5412=EDGE_CURVE('',#4204,#4205,#2643,.T.);
#5413=EDGE_CURVE('',#4205,#4203,#653,.T.);
#5414=EDGE_CURVE('',#4202,#4204,#654,.T.);
#5415=EDGE_CURVE('',#4206,#4207,#2644,.T.);
#5416=EDGE_CURVE('',#4206,#4208,#655,.T.);
#5417=EDGE_CURVE('',#4209,#4208,#3437,.F.);
#5418=EDGE_CURVE('',#4209,#4207,#656,.T.);
#5419=EDGE_CURVE('',#4210,#4211,#2645,.T.);
#5420=EDGE_CURVE('',#4211,#4212,#657,.T.);
#5421=EDGE_CURVE('',#4213,#4212,#3438,.T.);
#5422=EDGE_CURVE('',#4210,#4213,#658,.T.);
#5423=EDGE_CURVE('',#4214,#4215,#2646,.T.);
#5424=EDGE_CURVE('',#4215,#4211,#659,.T.);
#5425=EDGE_CURVE('',#4214,#4210,#660,.T.);
#5426=EDGE_CURVE('',#4216,#4217,#2647,.T.);
#5427=EDGE_CURVE('',#4217,#4215,#661,.T.);
#5428=EDGE_CURVE('',#4216,#4214,#662,.T.);
#5429=EDGE_CURVE('',#4218,#4219,#2648,.T.);
#5430=EDGE_CURVE('',#4220,#4218,#663,.T.);
#5431=EDGE_CURVE('',#4221,#4220,#3439,.T.);
#5432=EDGE_CURVE('',#4221,#4219,#664,.T.);
#5433=EDGE_CURVE('',#4219,#4217,#665,.T.);
#5434=EDGE_CURVE('',#4218,#4216,#666,.T.);
#5435=EDGE_CURVE('',#4212,#4201,#667,.T.);
#5436=EDGE_CURVE('',#4208,#4221,#668,.T.);
#5437=EDGE_CURVE('',#4204,#4206,#669,.T.);
#5438=EDGE_CURVE('',#4200,#4213,#670,.T.);
#5439=EDGE_CURVE('',#4207,#4205,#671,.T.);
#5440=EDGE_CURVE('',#4220,#4209,#672,.T.);
#5441=EDGE_CURVE('',#4222,#4223,#2649,.T.);
#5442=EDGE_CURVE('',#4223,#4224,#2650,.T.);
#5443=EDGE_CURVE('',#4224,#4225,#2651,.T.);
#5444=EDGE_CURVE('',#4225,#4226,#2652,.T.);
#5445=EDGE_CURVE('',#4226,#4227,#2653,.T.);
#5446=EDGE_CURVE('',#4227,#4222,#2654,.T.);
#5447=EDGE_CURVE('',#4228,#4229,#2655,.T.);
#5448=EDGE_CURVE('',#4229,#4222,#2656,.T.);
#5449=EDGE_CURVE('',#4228,#4227,#2657,.T.);
#5450=EDGE_CURVE('',#4230,#4228,#2658,.T.);
#5451=EDGE_CURVE('',#4230,#4226,#2659,.T.);
#5452=EDGE_CURVE('',#4231,#4230,#2660,.T.);
#5453=EDGE_CURVE('',#4231,#4225,#2661,.T.);
#5454=EDGE_CURVE('',#4232,#4231,#2662,.T.);
#5455=EDGE_CURVE('',#4232,#4224,#2663,.T.);
#5456=EDGE_CURVE('',#4233,#4232,#2664,.T.);
#5457=EDGE_CURVE('',#4233,#4223,#2665,.T.);
#5458=EDGE_CURVE('',#4229,#4233,#2666,.T.);
#5459=EDGE_CURVE('',#4234,#4235,#2667,.T.);
#5460=EDGE_CURVE('',#4235,#4236,#673,.T.);
#5461=EDGE_CURVE('',#4237,#4236,#3440,.T.);
#5462=EDGE_CURVE('',#4237,#4234,#674,.T.);
#5463=EDGE_CURVE('',#4238,#4239,#2668,.T.);
#5464=EDGE_CURVE('',#4239,#4235,#675,.T.);
#5465=EDGE_CURVE('',#4234,#4238,#676,.T.);
#5466=EDGE_CURVE('',#4240,#4241,#2669,.T.);
#5467=EDGE_CURVE('',#4241,#4239,#677,.T.);
#5468=EDGE_CURVE('',#4238,#4240,#678,.T.);
#5469=EDGE_CURVE('',#4242,#4243,#2670,.T.);
#5470=EDGE_CURVE('',#4242,#4244,#679,.T.);
#5471=EDGE_CURVE('',#4245,#4244,#3441,.F.);
#5472=EDGE_CURVE('',#4245,#4243,#680,.T.);
#5473=EDGE_CURVE('',#4246,#4247,#2671,.T.);
#5474=EDGE_CURVE('',#4247,#4248,#681,.T.);
#5475=EDGE_CURVE('',#4249,#4248,#3442,.T.);
#5476=EDGE_CURVE('',#4246,#4249,#682,.T.);
#5477=EDGE_CURVE('',#4250,#4251,#2672,.T.);
#5478=EDGE_CURVE('',#4251,#4247,#683,.T.);
#5479=EDGE_CURVE('',#4250,#4246,#684,.T.);
#5480=EDGE_CURVE('',#4252,#4253,#2673,.T.);
#5481=EDGE_CURVE('',#4253,#4251,#685,.T.);
#5482=EDGE_CURVE('',#4252,#4250,#686,.T.);
#5483=EDGE_CURVE('',#4254,#4255,#2674,.T.);
#5484=EDGE_CURVE('',#4256,#4254,#687,.T.);
#5485=EDGE_CURVE('',#4257,#4256,#3443,.T.);
#5486=EDGE_CURVE('',#4257,#4255,#688,.T.);
#5487=EDGE_CURVE('',#4255,#4253,#689,.T.);
#5488=EDGE_CURVE('',#4254,#4252,#690,.T.);
#5489=EDGE_CURVE('',#4248,#4237,#691,.T.);
#5490=EDGE_CURVE('',#4244,#4257,#692,.T.);
#5491=EDGE_CURVE('',#4240,#4242,#693,.T.);
#5492=EDGE_CURVE('',#4236,#4249,#694,.T.);
#5493=EDGE_CURVE('',#4243,#4241,#695,.T.);
#5494=EDGE_CURVE('',#4256,#4245,#696,.T.);
#5495=EDGE_CURVE('',#4258,#4259,#2675,.T.);
#5496=EDGE_CURVE('',#4259,#4260,#2676,.T.);
#5497=EDGE_CURVE('',#4260,#4261,#2677,.T.);
#5498=EDGE_CURVE('',#4261,#4262,#2678,.T.);
#5499=EDGE_CURVE('',#4262,#4263,#2679,.T.);
#5500=EDGE_CURVE('',#4263,#4258,#2680,.T.);
#5501=EDGE_CURVE('',#4264,#4265,#2681,.T.);
#5502=EDGE_CURVE('',#4265,#4258,#2682,.T.);
#5503=EDGE_CURVE('',#4264,#4263,#2683,.T.);
#5504=EDGE_CURVE('',#4266,#4264,#2684,.T.);
#5505=EDGE_CURVE('',#4266,#4262,#2685,.T.);
#5506=EDGE_CURVE('',#4267,#4266,#2686,.T.);
#5507=EDGE_CURVE('',#4267,#4261,#2687,.T.);
#5508=EDGE_CURVE('',#4268,#4267,#2688,.T.);
#5509=EDGE_CURVE('',#4268,#4260,#2689,.T.);
#5510=EDGE_CURVE('',#4269,#4268,#2690,.T.);
#5511=EDGE_CURVE('',#4269,#4259,#2691,.T.);
#5512=EDGE_CURVE('',#4265,#4269,#2692,.T.);
#5513=ORIENTED_EDGE('',*,*,#4270,.F.);
#5514=ORIENTED_EDGE('',*,*,#4271,.T.);
#5515=ORIENTED_EDGE('',*,*,#4272,.F.);
#5516=ORIENTED_EDGE('',*,*,#4271,.F.);
#5517=ORIENTED_EDGE('',*,*,#4270,.T.);
#5518=ORIENTED_EDGE('',*,*,#4273,.F.);
#5519=ORIENTED_EDGE('',*,*,#4274,.T.);
#5520=ORIENTED_EDGE('',*,*,#4275,.F.);
#5521=ORIENTED_EDGE('',*,*,#4274,.F.);
#5522=ORIENTED_EDGE('',*,*,#4273,.T.);
#5523=ORIENTED_EDGE('',*,*,#4276,.F.);
#5524=ORIENTED_EDGE('',*,*,#4277,.T.);
#5525=ORIENTED_EDGE('',*,*,#4278,.F.);
#5526=ORIENTED_EDGE('',*,*,#4277,.F.);
#5527=ORIENTED_EDGE('',*,*,#4279,.F.);
#5528=ORIENTED_EDGE('',*,*,#4280,.T.);
#5529=ORIENTED_EDGE('',*,*,#4281,.F.);
#5530=ORIENTED_EDGE('',*,*,#4280,.F.);
#5531=ORIENTED_EDGE('',*,*,#4282,.F.);
#5532=ORIENTED_EDGE('',*,*,#4283,.T.);
#5533=ORIENTED_EDGE('',*,*,#4284,.F.);
#5534=ORIENTED_EDGE('',*,*,#4283,.F.);
#5535=ORIENTED_EDGE('',*,*,#4285,.F.);
#5536=ORIENTED_EDGE('',*,*,#4286,.T.);
#5537=ORIENTED_EDGE('',*,*,#4287,.F.);
#5538=ORIENTED_EDGE('',*,*,#4286,.F.);
#5539=ORIENTED_EDGE('',*,*,#4288,.T.);
#5540=ORIENTED_EDGE('',*,*,#4289,.T.);
#5541=ORIENTED_EDGE('',*,*,#4290,.F.);
#5542=ORIENTED_EDGE('',*,*,#4291,.F.);
#5543=ORIENTED_EDGE('',*,*,#4292,.T.);
#5544=ORIENTED_EDGE('',*,*,#4291,.T.);
#5545=ORIENTED_EDGE('',*,*,#4293,.F.);
#5546=ORIENTED_EDGE('',*,*,#4294,.F.);
#5547=ORIENTED_EDGE('',*,*,#4295,.T.);
#5548=ORIENTED_EDGE('',*,*,#4294,.T.);
#5549=ORIENTED_EDGE('',*,*,#4296,.F.);
#5550=ORIENTED_EDGE('',*,*,#4297,.F.);
#5551=ORIENTED_EDGE('',*,*,#4298,.T.);
#5552=ORIENTED_EDGE('',*,*,#4297,.T.);
#5553=ORIENTED_EDGE('',*,*,#4299,.F.);
#5554=ORIENTED_EDGE('',*,*,#4289,.F.);
#5555=ORIENTED_EDGE('',*,*,#4299,.T.);
#5556=ORIENTED_EDGE('',*,*,#4296,.T.);
#5557=ORIENTED_EDGE('',*,*,#4293,.T.);
#5558=ORIENTED_EDGE('',*,*,#4290,.T.);
#5559=ORIENTED_EDGE('',*,*,#4272,.T.);
#5560=ORIENTED_EDGE('',*,*,#4275,.T.);
#5561=ORIENTED_EDGE('',*,*,#4278,.T.);
#5562=ORIENTED_EDGE('',*,*,#4281,.T.);
#5563=ORIENTED_EDGE('',*,*,#4284,.T.);
#5564=ORIENTED_EDGE('',*,*,#4287,.T.);
#5565=ORIENTED_EDGE('',*,*,#4298,.F.);
#5566=ORIENTED_EDGE('',*,*,#4288,.F.);
#5567=ORIENTED_EDGE('',*,*,#4292,.F.);
#5568=ORIENTED_EDGE('',*,*,#4295,.F.);
#5569=ORIENTED_EDGE('',*,*,#4276,.T.);
#5570=ORIENTED_EDGE('',*,*,#4279,.T.);
#5571=ORIENTED_EDGE('',*,*,#4282,.T.);
#5572=ORIENTED_EDGE('',*,*,#4285,.T.);
#5573=ORIENTED_EDGE('',*,*,#4300,.F.);
#5574=ORIENTED_EDGE('',*,*,#4301,.T.);
#5575=ORIENTED_EDGE('',*,*,#4302,.T.);
#5576=ORIENTED_EDGE('',*,*,#4303,.T.);
#5577=ORIENTED_EDGE('',*,*,#4304,.F.);
#5578=ORIENTED_EDGE('',*,*,#4305,.T.);
#5579=ORIENTED_EDGE('',*,*,#4300,.T.);
#5580=ORIENTED_EDGE('',*,*,#4306,.T.);
#5581=ORIENTED_EDGE('',*,*,#4307,.F.);
#5582=ORIENTED_EDGE('',*,*,#4308,.T.);
#5583=ORIENTED_EDGE('',*,*,#4304,.T.);
#5584=ORIENTED_EDGE('',*,*,#4309,.T.);
#5585=ORIENTED_EDGE('',*,*,#4310,.F.);
#5586=ORIENTED_EDGE('',*,*,#4311,.T.);
#5587=ORIENTED_EDGE('',*,*,#4307,.T.);
#5588=ORIENTED_EDGE('',*,*,#4312,.T.);
#5589=ORIENTED_EDGE('',*,*,#4313,.F.);
#5590=ORIENTED_EDGE('',*,*,#4314,.T.);
#5591=ORIENTED_EDGE('',*,*,#4310,.T.);
#5592=ORIENTED_EDGE('',*,*,#4315,.T.);
#5593=ORIENTED_EDGE('',*,*,#4316,.F.);
#5594=ORIENTED_EDGE('',*,*,#4317,.T.);
#5595=ORIENTED_EDGE('',*,*,#4313,.T.);
#5596=ORIENTED_EDGE('',*,*,#4318,.T.);
#5597=ORIENTED_EDGE('',*,*,#4319,.F.);
#5598=ORIENTED_EDGE('',*,*,#4320,.T.);
#5599=ORIENTED_EDGE('',*,*,#4316,.T.);
#5600=ORIENTED_EDGE('',*,*,#4321,.T.);
#5601=ORIENTED_EDGE('',*,*,#4322,.F.);
#5602=ORIENTED_EDGE('',*,*,#4323,.T.);
#5603=ORIENTED_EDGE('',*,*,#4319,.T.);
#5604=ORIENTED_EDGE('',*,*,#4324,.T.);
#5605=ORIENTED_EDGE('',*,*,#4325,.F.);
#5606=ORIENTED_EDGE('',*,*,#4326,.T.);
#5607=ORIENTED_EDGE('',*,*,#4322,.T.);
#5608=ORIENTED_EDGE('',*,*,#4327,.T.);
#5609=ORIENTED_EDGE('',*,*,#4328,.F.);
#5610=ORIENTED_EDGE('',*,*,#4329,.T.);
#5611=ORIENTED_EDGE('',*,*,#4325,.T.);
#5612=ORIENTED_EDGE('',*,*,#4330,.T.);
#5613=ORIENTED_EDGE('',*,*,#4331,.F.);
#5614=ORIENTED_EDGE('',*,*,#4332,.T.);
#5615=ORIENTED_EDGE('',*,*,#4328,.T.);
#5616=ORIENTED_EDGE('',*,*,#4333,.T.);
#5617=ORIENTED_EDGE('',*,*,#4334,.F.);
#5618=ORIENTED_EDGE('',*,*,#4335,.T.);
#5619=ORIENTED_EDGE('',*,*,#4331,.T.);
#5620=ORIENTED_EDGE('',*,*,#4336,.T.);
#5621=ORIENTED_EDGE('',*,*,#4337,.F.);
#5622=ORIENTED_EDGE('',*,*,#4338,.T.);
#5623=ORIENTED_EDGE('',*,*,#4334,.T.);
#5624=ORIENTED_EDGE('',*,*,#4339,.T.);
#5625=ORIENTED_EDGE('',*,*,#4340,.F.);
#5626=ORIENTED_EDGE('',*,*,#4341,.T.);
#5627=ORIENTED_EDGE('',*,*,#4337,.T.);
#5628=ORIENTED_EDGE('',*,*,#4342,.T.);
#5629=ORIENTED_EDGE('',*,*,#4343,.F.);
#5630=ORIENTED_EDGE('',*,*,#4344,.T.);
#5631=ORIENTED_EDGE('',*,*,#4340,.T.);
#5632=ORIENTED_EDGE('',*,*,#4345,.T.);
#5633=ORIENTED_EDGE('',*,*,#4346,.F.);
#5634=ORIENTED_EDGE('',*,*,#4347,.T.);
#5635=ORIENTED_EDGE('',*,*,#4343,.T.);
#5636=ORIENTED_EDGE('',*,*,#4348,.T.);
#5637=ORIENTED_EDGE('',*,*,#4349,.F.);
#5638=ORIENTED_EDGE('',*,*,#4350,.T.);
#5639=ORIENTED_EDGE('',*,*,#4346,.T.);
#5640=ORIENTED_EDGE('',*,*,#4351,.T.);
#5641=ORIENTED_EDGE('',*,*,#4352,.F.);
#5642=ORIENTED_EDGE('',*,*,#4353,.T.);
#5643=ORIENTED_EDGE('',*,*,#4349,.T.);
#5644=ORIENTED_EDGE('',*,*,#4354,.T.);
#5645=ORIENTED_EDGE('',*,*,#4355,.F.);
#5646=ORIENTED_EDGE('',*,*,#4356,.T.);
#5647=ORIENTED_EDGE('',*,*,#4352,.T.);
#5648=ORIENTED_EDGE('',*,*,#4357,.T.);
#5649=ORIENTED_EDGE('',*,*,#4358,.F.);
#5650=ORIENTED_EDGE('',*,*,#4359,.T.);
#5651=ORIENTED_EDGE('',*,*,#4355,.T.);
#5652=ORIENTED_EDGE('',*,*,#4360,.T.);
#5653=ORIENTED_EDGE('',*,*,#4361,.F.);
#5654=ORIENTED_EDGE('',*,*,#4362,.T.);
#5655=ORIENTED_EDGE('',*,*,#4358,.T.);
#5656=ORIENTED_EDGE('',*,*,#4363,.T.);
#5657=ORIENTED_EDGE('',*,*,#4364,.F.);
#5658=ORIENTED_EDGE('',*,*,#4365,.T.);
#5659=ORIENTED_EDGE('',*,*,#4361,.T.);
#5660=ORIENTED_EDGE('',*,*,#4366,.T.);
#5661=ORIENTED_EDGE('',*,*,#4367,.F.);
#5662=ORIENTED_EDGE('',*,*,#4368,.T.);
#5663=ORIENTED_EDGE('',*,*,#4364,.T.);
#5664=ORIENTED_EDGE('',*,*,#4369,.T.);
#5665=ORIENTED_EDGE('',*,*,#4370,.F.);
#5666=ORIENTED_EDGE('',*,*,#4371,.T.);
#5667=ORIENTED_EDGE('',*,*,#4367,.T.);
#5668=ORIENTED_EDGE('',*,*,#4372,.T.);
#5669=ORIENTED_EDGE('',*,*,#4373,.F.);
#5670=ORIENTED_EDGE('',*,*,#4374,.T.);
#5671=ORIENTED_EDGE('',*,*,#4370,.T.);
#5672=ORIENTED_EDGE('',*,*,#4375,.T.);
#5673=ORIENTED_EDGE('',*,*,#4376,.F.);
#5674=ORIENTED_EDGE('',*,*,#4377,.T.);
#5675=ORIENTED_EDGE('',*,*,#4373,.T.);
#5676=ORIENTED_EDGE('',*,*,#4378,.T.);
#5677=ORIENTED_EDGE('',*,*,#4379,.F.);
#5678=ORIENTED_EDGE('',*,*,#4380,.T.);
#5679=ORIENTED_EDGE('',*,*,#4376,.T.);
#5680=ORIENTED_EDGE('',*,*,#4381,.T.);
#5681=ORIENTED_EDGE('',*,*,#4382,.F.);
#5682=ORIENTED_EDGE('',*,*,#4383,.T.);
#5683=ORIENTED_EDGE('',*,*,#4379,.T.);
#5684=ORIENTED_EDGE('',*,*,#4384,.T.);
#5685=ORIENTED_EDGE('',*,*,#4385,.F.);
#5686=ORIENTED_EDGE('',*,*,#4386,.T.);
#5687=ORIENTED_EDGE('',*,*,#4382,.T.);
#5688=ORIENTED_EDGE('',*,*,#4387,.T.);
#5689=ORIENTED_EDGE('',*,*,#4388,.F.);
#5690=ORIENTED_EDGE('',*,*,#4389,.T.);
#5691=ORIENTED_EDGE('',*,*,#4385,.T.);
#5692=ORIENTED_EDGE('',*,*,#4390,.T.);
#5693=ORIENTED_EDGE('',*,*,#4391,.F.);
#5694=ORIENTED_EDGE('',*,*,#4392,.T.);
#5695=ORIENTED_EDGE('',*,*,#4388,.T.);
#5696=ORIENTED_EDGE('',*,*,#4393,.T.);
#5697=ORIENTED_EDGE('',*,*,#4394,.F.);
#5698=ORIENTED_EDGE('',*,*,#4395,.T.);
#5699=ORIENTED_EDGE('',*,*,#4391,.T.);
#5700=ORIENTED_EDGE('',*,*,#4396,.T.);
#5701=ORIENTED_EDGE('',*,*,#4397,.F.);
#5702=ORIENTED_EDGE('',*,*,#4398,.T.);
#5703=ORIENTED_EDGE('',*,*,#4394,.T.);
#5704=ORIENTED_EDGE('',*,*,#4399,.T.);
#5705=ORIENTED_EDGE('',*,*,#4400,.F.);
#5706=ORIENTED_EDGE('',*,*,#4401,.T.);
#5707=ORIENTED_EDGE('',*,*,#4397,.T.);
#5708=ORIENTED_EDGE('',*,*,#4402,.T.);
#5709=ORIENTED_EDGE('',*,*,#4403,.F.);
#5710=ORIENTED_EDGE('',*,*,#4404,.T.);
#5711=ORIENTED_EDGE('',*,*,#4400,.T.);
#5712=ORIENTED_EDGE('',*,*,#4405,.T.);
#5713=ORIENTED_EDGE('',*,*,#4406,.F.);
#5714=ORIENTED_EDGE('',*,*,#4407,.T.);
#5715=ORIENTED_EDGE('',*,*,#4403,.T.);
#5716=ORIENTED_EDGE('',*,*,#4408,.T.);
#5717=ORIENTED_EDGE('',*,*,#4409,.F.);
#5718=ORIENTED_EDGE('',*,*,#4410,.T.);
#5719=ORIENTED_EDGE('',*,*,#4406,.T.);
#5720=ORIENTED_EDGE('',*,*,#4411,.T.);
#5721=ORIENTED_EDGE('',*,*,#4412,.F.);
#5722=ORIENTED_EDGE('',*,*,#4413,.T.);
#5723=ORIENTED_EDGE('',*,*,#4409,.T.);
#5724=ORIENTED_EDGE('',*,*,#4414,.T.);
#5725=ORIENTED_EDGE('',*,*,#4415,.F.);
#5726=ORIENTED_EDGE('',*,*,#4416,.T.);
#5727=ORIENTED_EDGE('',*,*,#4412,.T.);
#5728=ORIENTED_EDGE('',*,*,#4417,.T.);
#5729=ORIENTED_EDGE('',*,*,#4418,.F.);
#5730=ORIENTED_EDGE('',*,*,#4419,.T.);
#5731=ORIENTED_EDGE('',*,*,#4415,.T.);
#5732=ORIENTED_EDGE('',*,*,#4420,.T.);
#5733=ORIENTED_EDGE('',*,*,#4421,.F.);
#5734=ORIENTED_EDGE('',*,*,#4422,.T.);
#5735=ORIENTED_EDGE('',*,*,#4418,.T.);
#5736=ORIENTED_EDGE('',*,*,#4423,.T.);
#5737=ORIENTED_EDGE('',*,*,#4424,.F.);
#5738=ORIENTED_EDGE('',*,*,#4425,.T.);
#5739=ORIENTED_EDGE('',*,*,#4421,.T.);
#5740=ORIENTED_EDGE('',*,*,#4426,.T.);
#5741=ORIENTED_EDGE('',*,*,#4427,.F.);
#5742=ORIENTED_EDGE('',*,*,#4428,.T.);
#5743=ORIENTED_EDGE('',*,*,#4424,.T.);
#5744=ORIENTED_EDGE('',*,*,#4429,.T.);
#5745=ORIENTED_EDGE('',*,*,#4430,.F.);
#5746=ORIENTED_EDGE('',*,*,#4431,.T.);
#5747=ORIENTED_EDGE('',*,*,#4427,.T.);
#5748=ORIENTED_EDGE('',*,*,#4432,.T.);
#5749=ORIENTED_EDGE('',*,*,#4433,.F.);
#5750=ORIENTED_EDGE('',*,*,#4434,.T.);
#5751=ORIENTED_EDGE('',*,*,#4430,.T.);
#5752=ORIENTED_EDGE('',*,*,#4435,.T.);
#5753=ORIENTED_EDGE('',*,*,#4436,.F.);
#5754=ORIENTED_EDGE('',*,*,#4437,.T.);
#5755=ORIENTED_EDGE('',*,*,#4433,.T.);
#5756=ORIENTED_EDGE('',*,*,#4438,.T.);
#5757=ORIENTED_EDGE('',*,*,#4439,.F.);
#5758=ORIENTED_EDGE('',*,*,#4440,.T.);
#5759=ORIENTED_EDGE('',*,*,#4436,.T.);
#5760=ORIENTED_EDGE('',*,*,#4441,.T.);
#5761=ORIENTED_EDGE('',*,*,#4442,.F.);
#5762=ORIENTED_EDGE('',*,*,#4443,.T.);
#5763=ORIENTED_EDGE('',*,*,#4439,.T.);
#5764=ORIENTED_EDGE('',*,*,#4444,.T.);
#5765=ORIENTED_EDGE('',*,*,#4445,.F.);
#5766=ORIENTED_EDGE('',*,*,#4446,.T.);
#5767=ORIENTED_EDGE('',*,*,#4442,.T.);
#5768=ORIENTED_EDGE('',*,*,#4447,.T.);
#5769=ORIENTED_EDGE('',*,*,#4448,.F.);
#5770=ORIENTED_EDGE('',*,*,#4449,.T.);
#5771=ORIENTED_EDGE('',*,*,#4445,.T.);
#5772=ORIENTED_EDGE('',*,*,#4450,.T.);
#5773=ORIENTED_EDGE('',*,*,#4451,.F.);
#5774=ORIENTED_EDGE('',*,*,#4452,.T.);
#5775=ORIENTED_EDGE('',*,*,#4448,.T.);
#5776=ORIENTED_EDGE('',*,*,#4453,.T.);
#5777=ORIENTED_EDGE('',*,*,#4454,.F.);
#5778=ORIENTED_EDGE('',*,*,#4455,.T.);
#5779=ORIENTED_EDGE('',*,*,#4451,.T.);
#5780=ORIENTED_EDGE('',*,*,#4456,.T.);
#5781=ORIENTED_EDGE('',*,*,#4457,.F.);
#5782=ORIENTED_EDGE('',*,*,#4458,.T.);
#5783=ORIENTED_EDGE('',*,*,#4454,.T.);
#5784=ORIENTED_EDGE('',*,*,#4459,.T.);
#5785=ORIENTED_EDGE('',*,*,#4460,.F.);
#5786=ORIENTED_EDGE('',*,*,#4461,.T.);
#5787=ORIENTED_EDGE('',*,*,#4457,.T.);
#5788=ORIENTED_EDGE('',*,*,#4462,.T.);
#5789=ORIENTED_EDGE('',*,*,#4463,.F.);
#5790=ORIENTED_EDGE('',*,*,#4464,.T.);
#5791=ORIENTED_EDGE('',*,*,#4460,.T.);
#5792=ORIENTED_EDGE('',*,*,#4465,.T.);
#5793=ORIENTED_EDGE('',*,*,#4466,.F.);
#5794=ORIENTED_EDGE('',*,*,#4467,.T.);
#5795=ORIENTED_EDGE('',*,*,#4463,.T.);
#5796=ORIENTED_EDGE('',*,*,#4468,.T.);
#5797=ORIENTED_EDGE('',*,*,#4469,.F.);
#5798=ORIENTED_EDGE('',*,*,#4470,.T.);
#5799=ORIENTED_EDGE('',*,*,#4466,.T.);
#5800=ORIENTED_EDGE('',*,*,#4471,.T.);
#5801=ORIENTED_EDGE('',*,*,#4472,.F.);
#5802=ORIENTED_EDGE('',*,*,#4473,.T.);
#5803=ORIENTED_EDGE('',*,*,#4469,.T.);
#5804=ORIENTED_EDGE('',*,*,#4474,.T.);
#5805=ORIENTED_EDGE('',*,*,#4475,.F.);
#5806=ORIENTED_EDGE('',*,*,#4476,.T.);
#5807=ORIENTED_EDGE('',*,*,#4472,.T.);
#5808=ORIENTED_EDGE('',*,*,#4477,.T.);
#5809=ORIENTED_EDGE('',*,*,#4478,.F.);
#5810=ORIENTED_EDGE('',*,*,#4479,.T.);
#5811=ORIENTED_EDGE('',*,*,#4475,.T.);
#5812=ORIENTED_EDGE('',*,*,#4480,.T.);
#5813=ORIENTED_EDGE('',*,*,#4481,.F.);
#5814=ORIENTED_EDGE('',*,*,#4482,.T.);
#5815=ORIENTED_EDGE('',*,*,#4478,.T.);
#5816=ORIENTED_EDGE('',*,*,#4483,.T.);
#5817=ORIENTED_EDGE('',*,*,#4484,.F.);
#5818=ORIENTED_EDGE('',*,*,#4485,.T.);
#5819=ORIENTED_EDGE('',*,*,#4481,.T.);
#5820=ORIENTED_EDGE('',*,*,#4486,.T.);
#5821=ORIENTED_EDGE('',*,*,#4487,.F.);
#5822=ORIENTED_EDGE('',*,*,#4488,.T.);
#5823=ORIENTED_EDGE('',*,*,#4484,.T.);
#5824=ORIENTED_EDGE('',*,*,#4489,.T.);
#5825=ORIENTED_EDGE('',*,*,#4490,.F.);
#5826=ORIENTED_EDGE('',*,*,#4491,.T.);
#5827=ORIENTED_EDGE('',*,*,#4487,.T.);
#5828=ORIENTED_EDGE('',*,*,#4492,.T.);
#5829=ORIENTED_EDGE('',*,*,#4493,.F.);
#5830=ORIENTED_EDGE('',*,*,#4494,.T.);
#5831=ORIENTED_EDGE('',*,*,#4490,.T.);
#5832=ORIENTED_EDGE('',*,*,#4495,.T.);
#5833=ORIENTED_EDGE('',*,*,#4496,.F.);
#5834=ORIENTED_EDGE('',*,*,#4497,.T.);
#5835=ORIENTED_EDGE('',*,*,#4493,.T.);
#5836=ORIENTED_EDGE('',*,*,#4498,.T.);
#5837=ORIENTED_EDGE('',*,*,#4499,.F.);
#5838=ORIENTED_EDGE('',*,*,#4500,.T.);
#5839=ORIENTED_EDGE('',*,*,#4496,.T.);
#5840=ORIENTED_EDGE('',*,*,#4501,.T.);
#5841=ORIENTED_EDGE('',*,*,#4502,.F.);
#5842=ORIENTED_EDGE('',*,*,#4503,.T.);
#5843=ORIENTED_EDGE('',*,*,#4499,.T.);
#5844=ORIENTED_EDGE('',*,*,#4504,.T.);
#5845=ORIENTED_EDGE('',*,*,#4505,.F.);
#5846=ORIENTED_EDGE('',*,*,#4506,.T.);
#5847=ORIENTED_EDGE('',*,*,#4502,.T.);
#5848=ORIENTED_EDGE('',*,*,#4507,.T.);
#5849=ORIENTED_EDGE('',*,*,#4508,.F.);
#5850=ORIENTED_EDGE('',*,*,#4509,.T.);
#5851=ORIENTED_EDGE('',*,*,#4505,.T.);
#5852=ORIENTED_EDGE('',*,*,#4510,.T.);
#5853=ORIENTED_EDGE('',*,*,#4511,.F.);
#5854=ORIENTED_EDGE('',*,*,#4512,.T.);
#5855=ORIENTED_EDGE('',*,*,#4508,.T.);
#5856=ORIENTED_EDGE('',*,*,#4513,.T.);
#5857=ORIENTED_EDGE('',*,*,#4514,.F.);
#5858=ORIENTED_EDGE('',*,*,#4515,.T.);
#5859=ORIENTED_EDGE('',*,*,#4511,.T.);
#5860=ORIENTED_EDGE('',*,*,#4516,.T.);
#5861=ORIENTED_EDGE('',*,*,#4517,.F.);
#5862=ORIENTED_EDGE('',*,*,#4518,.T.);
#5863=ORIENTED_EDGE('',*,*,#4514,.T.);
#5864=ORIENTED_EDGE('',*,*,#4519,.T.);
#5865=ORIENTED_EDGE('',*,*,#4520,.F.);
#5866=ORIENTED_EDGE('',*,*,#4521,.T.);
#5867=ORIENTED_EDGE('',*,*,#4517,.T.);
#5868=ORIENTED_EDGE('',*,*,#4522,.T.);
#5869=ORIENTED_EDGE('',*,*,#4523,.F.);
#5870=ORIENTED_EDGE('',*,*,#4524,.T.);
#5871=ORIENTED_EDGE('',*,*,#4520,.T.);
#5872=ORIENTED_EDGE('',*,*,#4525,.T.);
#5873=ORIENTED_EDGE('',*,*,#4526,.F.);
#5874=ORIENTED_EDGE('',*,*,#4527,.T.);
#5875=ORIENTED_EDGE('',*,*,#4523,.T.);
#5876=ORIENTED_EDGE('',*,*,#4528,.T.);
#5877=ORIENTED_EDGE('',*,*,#4529,.F.);
#5878=ORIENTED_EDGE('',*,*,#4530,.T.);
#5879=ORIENTED_EDGE('',*,*,#4526,.T.);
#5880=ORIENTED_EDGE('',*,*,#4531,.T.);
#5881=ORIENTED_EDGE('',*,*,#4532,.F.);
#5882=ORIENTED_EDGE('',*,*,#4533,.T.);
#5883=ORIENTED_EDGE('',*,*,#4529,.T.);
#5884=ORIENTED_EDGE('',*,*,#4534,.T.);
#5885=ORIENTED_EDGE('',*,*,#4535,.F.);
#5886=ORIENTED_EDGE('',*,*,#4536,.T.);
#5887=ORIENTED_EDGE('',*,*,#4532,.T.);
#5888=ORIENTED_EDGE('',*,*,#4537,.T.);
#5889=ORIENTED_EDGE('',*,*,#4538,.F.);
#5890=ORIENTED_EDGE('',*,*,#4539,.T.);
#5891=ORIENTED_EDGE('',*,*,#4535,.T.);
#5892=ORIENTED_EDGE('',*,*,#4540,.T.);
#5893=ORIENTED_EDGE('',*,*,#4541,.F.);
#5894=ORIENTED_EDGE('',*,*,#4542,.T.);
#5895=ORIENTED_EDGE('',*,*,#4538,.T.);
#5896=ORIENTED_EDGE('',*,*,#4543,.T.);
#5897=ORIENTED_EDGE('',*,*,#4544,.F.);
#5898=ORIENTED_EDGE('',*,*,#4545,.T.);
#5899=ORIENTED_EDGE('',*,*,#4541,.T.);
#5900=ORIENTED_EDGE('',*,*,#4546,.T.);
#5901=ORIENTED_EDGE('',*,*,#4547,.F.);
#5902=ORIENTED_EDGE('',*,*,#4548,.T.);
#5903=ORIENTED_EDGE('',*,*,#4544,.T.);
#5904=ORIENTED_EDGE('',*,*,#4549,.T.);
#5905=ORIENTED_EDGE('',*,*,#4550,.F.);
#5906=ORIENTED_EDGE('',*,*,#4551,.T.);
#5907=ORIENTED_EDGE('',*,*,#4547,.T.);
#5908=ORIENTED_EDGE('',*,*,#4552,.T.);
#5909=ORIENTED_EDGE('',*,*,#4553,.F.);
#5910=ORIENTED_EDGE('',*,*,#4554,.T.);
#5911=ORIENTED_EDGE('',*,*,#4550,.T.);
#5912=ORIENTED_EDGE('',*,*,#4555,.T.);
#5913=ORIENTED_EDGE('',*,*,#4556,.F.);
#5914=ORIENTED_EDGE('',*,*,#4557,.T.);
#5915=ORIENTED_EDGE('',*,*,#4553,.T.);
#5916=ORIENTED_EDGE('',*,*,#4558,.T.);
#5917=ORIENTED_EDGE('',*,*,#4559,.F.);
#5918=ORIENTED_EDGE('',*,*,#4560,.T.);
#5919=ORIENTED_EDGE('',*,*,#4556,.T.);
#5920=ORIENTED_EDGE('',*,*,#4561,.T.);
#5921=ORIENTED_EDGE('',*,*,#4562,.F.);
#5922=ORIENTED_EDGE('',*,*,#4563,.T.);
#5923=ORIENTED_EDGE('',*,*,#4559,.T.);
#5924=ORIENTED_EDGE('',*,*,#4564,.T.);
#5925=ORIENTED_EDGE('',*,*,#4565,.F.);
#5926=ORIENTED_EDGE('',*,*,#4566,.T.);
#5927=ORIENTED_EDGE('',*,*,#4562,.T.);
#5928=ORIENTED_EDGE('',*,*,#4567,.T.);
#5929=ORIENTED_EDGE('',*,*,#4568,.F.);
#5930=ORIENTED_EDGE('',*,*,#4569,.T.);
#5931=ORIENTED_EDGE('',*,*,#4565,.T.);
#5932=ORIENTED_EDGE('',*,*,#4570,.T.);
#5933=ORIENTED_EDGE('',*,*,#4571,.F.);
#5934=ORIENTED_EDGE('',*,*,#4572,.T.);
#5935=ORIENTED_EDGE('',*,*,#4568,.T.);
#5936=ORIENTED_EDGE('',*,*,#4573,.T.);
#5937=ORIENTED_EDGE('',*,*,#4574,.F.);
#5938=ORIENTED_EDGE('',*,*,#4575,.T.);
#5939=ORIENTED_EDGE('',*,*,#4571,.T.);
#5940=ORIENTED_EDGE('',*,*,#4576,.T.);
#5941=ORIENTED_EDGE('',*,*,#4577,.F.);
#5942=ORIENTED_EDGE('',*,*,#4578,.T.);
#5943=ORIENTED_EDGE('',*,*,#4574,.T.);
#5944=ORIENTED_EDGE('',*,*,#4579,.T.);
#5945=ORIENTED_EDGE('',*,*,#4580,.F.);
#5946=ORIENTED_EDGE('',*,*,#4581,.T.);
#5947=ORIENTED_EDGE('',*,*,#4577,.T.);
#5948=ORIENTED_EDGE('',*,*,#4582,.T.);
#5949=ORIENTED_EDGE('',*,*,#4583,.F.);
#5950=ORIENTED_EDGE('',*,*,#4584,.T.);
#5951=ORIENTED_EDGE('',*,*,#4585,.F.);
#5952=ORIENTED_EDGE('',*,*,#4586,.F.);
#5953=ORIENTED_EDGE('',*,*,#4587,.F.);
#5954=ORIENTED_EDGE('',*,*,#4588,.T.);
#5955=ORIENTED_EDGE('',*,*,#4583,.T.);
#5956=ORIENTED_EDGE('',*,*,#4589,.F.);
#5957=ORIENTED_EDGE('',*,*,#4590,.F.);
#5958=ORIENTED_EDGE('',*,*,#4591,.T.);
#5959=ORIENTED_EDGE('',*,*,#4587,.T.);
#5960=ORIENTED_EDGE('',*,*,#4592,.F.);
#5961=ORIENTED_EDGE('',*,*,#4593,.F.);
#5962=ORIENTED_EDGE('',*,*,#4594,.T.);
#5963=ORIENTED_EDGE('',*,*,#4590,.T.);
#5964=ORIENTED_EDGE('',*,*,#4595,.F.);
#5965=ORIENTED_EDGE('',*,*,#4596,.F.);
#5966=ORIENTED_EDGE('',*,*,#4597,.T.);
#5967=ORIENTED_EDGE('',*,*,#4593,.T.);
#5968=ORIENTED_EDGE('',*,*,#4598,.F.);
#5969=ORIENTED_EDGE('',*,*,#4599,.F.);
#5970=ORIENTED_EDGE('',*,*,#4600,.T.);
#5971=ORIENTED_EDGE('',*,*,#4596,.T.);
#5972=ORIENTED_EDGE('',*,*,#4601,.F.);
#5973=ORIENTED_EDGE('',*,*,#4602,.F.);
#5974=ORIENTED_EDGE('',*,*,#4603,.T.);
#5975=ORIENTED_EDGE('',*,*,#4599,.T.);
#5976=ORIENTED_EDGE('',*,*,#4604,.F.);
#5977=ORIENTED_EDGE('',*,*,#4605,.F.);
#5978=ORIENTED_EDGE('',*,*,#4606,.T.);
#5979=ORIENTED_EDGE('',*,*,#4602,.T.);
#5980=ORIENTED_EDGE('',*,*,#4607,.F.);
#5981=ORIENTED_EDGE('',*,*,#4608,.F.);
#5982=ORIENTED_EDGE('',*,*,#4609,.T.);
#5983=ORIENTED_EDGE('',*,*,#4605,.T.);
#5984=ORIENTED_EDGE('',*,*,#4610,.F.);
#5985=ORIENTED_EDGE('',*,*,#4611,.F.);
#5986=ORIENTED_EDGE('',*,*,#4612,.T.);
#5987=ORIENTED_EDGE('',*,*,#4608,.T.);
#5988=ORIENTED_EDGE('',*,*,#4613,.F.);
#5989=ORIENTED_EDGE('',*,*,#4614,.F.);
#5990=ORIENTED_EDGE('',*,*,#4615,.T.);
#5991=ORIENTED_EDGE('',*,*,#4611,.T.);
#5992=ORIENTED_EDGE('',*,*,#4616,.F.);
#5993=ORIENTED_EDGE('',*,*,#4617,.F.);
#5994=ORIENTED_EDGE('',*,*,#4618,.T.);
#5995=ORIENTED_EDGE('',*,*,#4614,.T.);
#5996=ORIENTED_EDGE('',*,*,#4619,.F.);
#5997=ORIENTED_EDGE('',*,*,#4620,.F.);
#5998=ORIENTED_EDGE('',*,*,#4621,.T.);
#5999=ORIENTED_EDGE('',*,*,#4617,.T.);
#6000=ORIENTED_EDGE('',*,*,#4622,.F.);
#6001=ORIENTED_EDGE('',*,*,#4623,.F.);
#6002=ORIENTED_EDGE('',*,*,#4624,.T.);
#6003=ORIENTED_EDGE('',*,*,#4620,.T.);
#6004=ORIENTED_EDGE('',*,*,#4625,.F.);
#6005=ORIENTED_EDGE('',*,*,#4626,.F.);
#6006=ORIENTED_EDGE('',*,*,#4627,.T.);
#6007=ORIENTED_EDGE('',*,*,#4623,.T.);
#6008=ORIENTED_EDGE('',*,*,#4628,.F.);
#6009=ORIENTED_EDGE('',*,*,#4629,.F.);
#6010=ORIENTED_EDGE('',*,*,#4630,.T.);
#6011=ORIENTED_EDGE('',*,*,#4626,.T.);
#6012=ORIENTED_EDGE('',*,*,#4631,.F.);
#6013=ORIENTED_EDGE('',*,*,#4632,.F.);
#6014=ORIENTED_EDGE('',*,*,#4633,.T.);
#6015=ORIENTED_EDGE('',*,*,#4629,.T.);
#6016=ORIENTED_EDGE('',*,*,#4634,.F.);
#6017=ORIENTED_EDGE('',*,*,#4635,.F.);
#6018=ORIENTED_EDGE('',*,*,#4636,.T.);
#6019=ORIENTED_EDGE('',*,*,#4632,.T.);
#6020=ORIENTED_EDGE('',*,*,#4637,.F.);
#6021=ORIENTED_EDGE('',*,*,#4638,.F.);
#6022=ORIENTED_EDGE('',*,*,#4639,.T.);
#6023=ORIENTED_EDGE('',*,*,#4635,.T.);
#6024=ORIENTED_EDGE('',*,*,#4640,.F.);
#6025=ORIENTED_EDGE('',*,*,#4641,.F.);
#6026=ORIENTED_EDGE('',*,*,#4642,.T.);
#6027=ORIENTED_EDGE('',*,*,#4638,.T.);
#6028=ORIENTED_EDGE('',*,*,#4643,.F.);
#6029=ORIENTED_EDGE('',*,*,#4644,.F.);
#6030=ORIENTED_EDGE('',*,*,#4645,.T.);
#6031=ORIENTED_EDGE('',*,*,#4641,.T.);
#6032=ORIENTED_EDGE('',*,*,#4646,.F.);
#6033=ORIENTED_EDGE('',*,*,#4647,.F.);
#6034=ORIENTED_EDGE('',*,*,#4648,.T.);
#6035=ORIENTED_EDGE('',*,*,#4644,.T.);
#6036=ORIENTED_EDGE('',*,*,#4649,.F.);
#6037=ORIENTED_EDGE('',*,*,#4650,.F.);
#6038=ORIENTED_EDGE('',*,*,#4651,.T.);
#6039=ORIENTED_EDGE('',*,*,#4647,.T.);
#6040=ORIENTED_EDGE('',*,*,#4652,.F.);
#6041=ORIENTED_EDGE('',*,*,#4653,.F.);
#6042=ORIENTED_EDGE('',*,*,#4654,.T.);
#6043=ORIENTED_EDGE('',*,*,#4650,.T.);
#6044=ORIENTED_EDGE('',*,*,#4655,.F.);
#6045=ORIENTED_EDGE('',*,*,#4656,.F.);
#6046=ORIENTED_EDGE('',*,*,#4657,.T.);
#6047=ORIENTED_EDGE('',*,*,#4653,.T.);
#6048=ORIENTED_EDGE('',*,*,#4658,.F.);
#6049=ORIENTED_EDGE('',*,*,#4659,.F.);
#6050=ORIENTED_EDGE('',*,*,#4660,.T.);
#6051=ORIENTED_EDGE('',*,*,#4656,.T.);
#6052=ORIENTED_EDGE('',*,*,#4661,.F.);
#6053=ORIENTED_EDGE('',*,*,#4662,.F.);
#6054=ORIENTED_EDGE('',*,*,#4663,.T.);
#6055=ORIENTED_EDGE('',*,*,#4659,.T.);
#6056=ORIENTED_EDGE('',*,*,#4664,.F.);
#6057=ORIENTED_EDGE('',*,*,#4665,.F.);
#6058=ORIENTED_EDGE('',*,*,#4666,.T.);
#6059=ORIENTED_EDGE('',*,*,#4662,.T.);
#6060=ORIENTED_EDGE('',*,*,#4667,.F.);
#6061=ORIENTED_EDGE('',*,*,#4668,.F.);
#6062=ORIENTED_EDGE('',*,*,#4669,.T.);
#6063=ORIENTED_EDGE('',*,*,#4665,.T.);
#6064=ORIENTED_EDGE('',*,*,#4670,.F.);
#6065=ORIENTED_EDGE('',*,*,#4671,.F.);
#6066=ORIENTED_EDGE('',*,*,#4672,.T.);
#6067=ORIENTED_EDGE('',*,*,#4668,.T.);
#6068=ORIENTED_EDGE('',*,*,#4673,.F.);
#6069=ORIENTED_EDGE('',*,*,#4674,.F.);
#6070=ORIENTED_EDGE('',*,*,#4675,.T.);
#6071=ORIENTED_EDGE('',*,*,#4671,.T.);
#6072=ORIENTED_EDGE('',*,*,#4676,.F.);
#6073=ORIENTED_EDGE('',*,*,#4677,.F.);
#6074=ORIENTED_EDGE('',*,*,#4678,.T.);
#6075=ORIENTED_EDGE('',*,*,#4674,.T.);
#6076=ORIENTED_EDGE('',*,*,#4679,.F.);
#6077=ORIENTED_EDGE('',*,*,#4680,.F.);
#6078=ORIENTED_EDGE('',*,*,#4681,.T.);
#6079=ORIENTED_EDGE('',*,*,#4677,.T.);
#6080=ORIENTED_EDGE('',*,*,#4682,.F.);
#6081=ORIENTED_EDGE('',*,*,#4683,.F.);
#6082=ORIENTED_EDGE('',*,*,#4684,.T.);
#6083=ORIENTED_EDGE('',*,*,#4680,.T.);
#6084=ORIENTED_EDGE('',*,*,#4685,.F.);
#6085=ORIENTED_EDGE('',*,*,#4686,.F.);
#6086=ORIENTED_EDGE('',*,*,#4687,.T.);
#6087=ORIENTED_EDGE('',*,*,#4683,.T.);
#6088=ORIENTED_EDGE('',*,*,#4688,.F.);
#6089=ORIENTED_EDGE('',*,*,#4689,.F.);
#6090=ORIENTED_EDGE('',*,*,#4690,.T.);
#6091=ORIENTED_EDGE('',*,*,#4686,.T.);
#6092=ORIENTED_EDGE('',*,*,#4691,.F.);
#6093=ORIENTED_EDGE('',*,*,#4692,.F.);
#6094=ORIENTED_EDGE('',*,*,#4693,.T.);
#6095=ORIENTED_EDGE('',*,*,#4689,.T.);
#6096=ORIENTED_EDGE('',*,*,#4694,.F.);
#6097=ORIENTED_EDGE('',*,*,#4695,.F.);
#6098=ORIENTED_EDGE('',*,*,#4696,.T.);
#6099=ORIENTED_EDGE('',*,*,#4692,.T.);
#6100=ORIENTED_EDGE('',*,*,#4697,.F.);
#6101=ORIENTED_EDGE('',*,*,#4698,.F.);
#6102=ORIENTED_EDGE('',*,*,#4699,.T.);
#6103=ORIENTED_EDGE('',*,*,#4695,.T.);
#6104=ORIENTED_EDGE('',*,*,#4700,.F.);
#6105=ORIENTED_EDGE('',*,*,#4701,.F.);
#6106=ORIENTED_EDGE('',*,*,#4702,.T.);
#6107=ORIENTED_EDGE('',*,*,#4698,.T.);
#6108=ORIENTED_EDGE('',*,*,#4703,.F.);
#6109=ORIENTED_EDGE('',*,*,#4704,.F.);
#6110=ORIENTED_EDGE('',*,*,#4705,.T.);
#6111=ORIENTED_EDGE('',*,*,#4701,.T.);
#6112=ORIENTED_EDGE('',*,*,#4706,.F.);
#6113=ORIENTED_EDGE('',*,*,#4707,.F.);
#6114=ORIENTED_EDGE('',*,*,#4708,.T.);
#6115=ORIENTED_EDGE('',*,*,#4704,.T.);
#6116=ORIENTED_EDGE('',*,*,#4709,.F.);
#6117=ORIENTED_EDGE('',*,*,#4710,.F.);
#6118=ORIENTED_EDGE('',*,*,#4711,.T.);
#6119=ORIENTED_EDGE('',*,*,#4707,.T.);
#6120=ORIENTED_EDGE('',*,*,#4712,.F.);
#6121=ORIENTED_EDGE('',*,*,#4713,.F.);
#6122=ORIENTED_EDGE('',*,*,#4714,.T.);
#6123=ORIENTED_EDGE('',*,*,#4710,.T.);
#6124=ORIENTED_EDGE('',*,*,#4715,.F.);
#6125=ORIENTED_EDGE('',*,*,#4716,.F.);
#6126=ORIENTED_EDGE('',*,*,#4717,.T.);
#6127=ORIENTED_EDGE('',*,*,#4713,.T.);
#6128=ORIENTED_EDGE('',*,*,#4718,.F.);
#6129=ORIENTED_EDGE('',*,*,#4719,.F.);
#6130=ORIENTED_EDGE('',*,*,#4720,.T.);
#6131=ORIENTED_EDGE('',*,*,#4716,.T.);
#6132=ORIENTED_EDGE('',*,*,#4721,.F.);
#6133=ORIENTED_EDGE('',*,*,#4722,.F.);
#6134=ORIENTED_EDGE('',*,*,#4723,.T.);
#6135=ORIENTED_EDGE('',*,*,#4719,.T.);
#6136=ORIENTED_EDGE('',*,*,#4724,.F.);
#6137=ORIENTED_EDGE('',*,*,#4725,.F.);
#6138=ORIENTED_EDGE('',*,*,#4726,.T.);
#6139=ORIENTED_EDGE('',*,*,#4722,.T.);
#6140=ORIENTED_EDGE('',*,*,#4727,.F.);
#6141=ORIENTED_EDGE('',*,*,#4728,.F.);
#6142=ORIENTED_EDGE('',*,*,#4729,.T.);
#6143=ORIENTED_EDGE('',*,*,#4725,.T.);
#6144=ORIENTED_EDGE('',*,*,#4730,.F.);
#6145=ORIENTED_EDGE('',*,*,#4731,.F.);
#6146=ORIENTED_EDGE('',*,*,#4732,.T.);
#6147=ORIENTED_EDGE('',*,*,#4728,.T.);
#6148=ORIENTED_EDGE('',*,*,#4733,.F.);
#6149=ORIENTED_EDGE('',*,*,#4734,.F.);
#6150=ORIENTED_EDGE('',*,*,#4735,.T.);
#6151=ORIENTED_EDGE('',*,*,#4731,.T.);
#6152=ORIENTED_EDGE('',*,*,#4736,.F.);
#6153=ORIENTED_EDGE('',*,*,#4737,.F.);
#6154=ORIENTED_EDGE('',*,*,#4738,.T.);
#6155=ORIENTED_EDGE('',*,*,#4734,.T.);
#6156=ORIENTED_EDGE('',*,*,#4739,.F.);
#6157=ORIENTED_EDGE('',*,*,#4740,.F.);
#6158=ORIENTED_EDGE('',*,*,#4741,.T.);
#6159=ORIENTED_EDGE('',*,*,#4737,.T.);
#6160=ORIENTED_EDGE('',*,*,#4742,.F.);
#6161=ORIENTED_EDGE('',*,*,#4743,.F.);
#6162=ORIENTED_EDGE('',*,*,#4744,.T.);
#6163=ORIENTED_EDGE('',*,*,#4740,.T.);
#6164=ORIENTED_EDGE('',*,*,#4745,.F.);
#6165=ORIENTED_EDGE('',*,*,#4746,.F.);
#6166=ORIENTED_EDGE('',*,*,#4747,.T.);
#6167=ORIENTED_EDGE('',*,*,#4743,.T.);
#6168=ORIENTED_EDGE('',*,*,#4748,.F.);
#6169=ORIENTED_EDGE('',*,*,#4749,.F.);
#6170=ORIENTED_EDGE('',*,*,#4750,.T.);
#6171=ORIENTED_EDGE('',*,*,#4746,.T.);
#6172=ORIENTED_EDGE('',*,*,#4751,.F.);
#6173=ORIENTED_EDGE('',*,*,#4752,.F.);
#6174=ORIENTED_EDGE('',*,*,#4753,.T.);
#6175=ORIENTED_EDGE('',*,*,#4749,.T.);
#6176=ORIENTED_EDGE('',*,*,#4754,.F.);
#6177=ORIENTED_EDGE('',*,*,#4755,.F.);
#6178=ORIENTED_EDGE('',*,*,#4756,.T.);
#6179=ORIENTED_EDGE('',*,*,#4752,.T.);
#6180=ORIENTED_EDGE('',*,*,#4757,.F.);
#6181=ORIENTED_EDGE('',*,*,#4758,.F.);
#6182=ORIENTED_EDGE('',*,*,#4759,.T.);
#6183=ORIENTED_EDGE('',*,*,#4755,.T.);
#6184=ORIENTED_EDGE('',*,*,#4760,.F.);
#6185=ORIENTED_EDGE('',*,*,#4761,.F.);
#6186=ORIENTED_EDGE('',*,*,#4762,.T.);
#6187=ORIENTED_EDGE('',*,*,#4758,.T.);
#6188=ORIENTED_EDGE('',*,*,#4763,.F.);
#6189=ORIENTED_EDGE('',*,*,#4764,.F.);
#6190=ORIENTED_EDGE('',*,*,#4765,.T.);
#6191=ORIENTED_EDGE('',*,*,#4761,.T.);
#6192=ORIENTED_EDGE('',*,*,#4766,.F.);
#6193=ORIENTED_EDGE('',*,*,#4767,.F.);
#6194=ORIENTED_EDGE('',*,*,#4768,.T.);
#6195=ORIENTED_EDGE('',*,*,#4764,.T.);
#6196=ORIENTED_EDGE('',*,*,#4769,.F.);
#6197=ORIENTED_EDGE('',*,*,#4770,.F.);
#6198=ORIENTED_EDGE('',*,*,#4771,.T.);
#6199=ORIENTED_EDGE('',*,*,#4767,.T.);
#6200=ORIENTED_EDGE('',*,*,#4772,.F.);
#6201=ORIENTED_EDGE('',*,*,#4773,.F.);
#6202=ORIENTED_EDGE('',*,*,#4774,.T.);
#6203=ORIENTED_EDGE('',*,*,#4770,.T.);
#6204=ORIENTED_EDGE('',*,*,#4775,.F.);
#6205=ORIENTED_EDGE('',*,*,#4776,.F.);
#6206=ORIENTED_EDGE('',*,*,#4777,.T.);
#6207=ORIENTED_EDGE('',*,*,#4773,.T.);
#6208=ORIENTED_EDGE('',*,*,#4778,.F.);
#6209=ORIENTED_EDGE('',*,*,#4779,.F.);
#6210=ORIENTED_EDGE('',*,*,#4780,.T.);
#6211=ORIENTED_EDGE('',*,*,#4776,.T.);
#6212=ORIENTED_EDGE('',*,*,#4781,.F.);
#6213=ORIENTED_EDGE('',*,*,#4782,.F.);
#6214=ORIENTED_EDGE('',*,*,#4783,.T.);
#6215=ORIENTED_EDGE('',*,*,#4779,.T.);
#6216=ORIENTED_EDGE('',*,*,#4784,.F.);
#6217=ORIENTED_EDGE('',*,*,#4785,.F.);
#6218=ORIENTED_EDGE('',*,*,#4786,.T.);
#6219=ORIENTED_EDGE('',*,*,#4782,.T.);
#6220=ORIENTED_EDGE('',*,*,#4787,.F.);
#6221=ORIENTED_EDGE('',*,*,#4788,.F.);
#6222=ORIENTED_EDGE('',*,*,#4789,.T.);
#6223=ORIENTED_EDGE('',*,*,#4785,.T.);
#6224=ORIENTED_EDGE('',*,*,#4790,.F.);
#6225=ORIENTED_EDGE('',*,*,#4791,.F.);
#6226=ORIENTED_EDGE('',*,*,#4792,.T.);
#6227=ORIENTED_EDGE('',*,*,#4788,.T.);
#6228=ORIENTED_EDGE('',*,*,#4793,.F.);
#6229=ORIENTED_EDGE('',*,*,#4794,.F.);
#6230=ORIENTED_EDGE('',*,*,#4795,.T.);
#6231=ORIENTED_EDGE('',*,*,#4791,.T.);
#6232=ORIENTED_EDGE('',*,*,#4796,.F.);
#6233=ORIENTED_EDGE('',*,*,#4797,.F.);
#6234=ORIENTED_EDGE('',*,*,#4798,.T.);
#6235=ORIENTED_EDGE('',*,*,#4794,.T.);
#6236=ORIENTED_EDGE('',*,*,#4799,.F.);
#6237=ORIENTED_EDGE('',*,*,#4800,.F.);
#6238=ORIENTED_EDGE('',*,*,#4801,.T.);
#6239=ORIENTED_EDGE('',*,*,#4797,.T.);
#6240=ORIENTED_EDGE('',*,*,#4802,.F.);
#6241=ORIENTED_EDGE('',*,*,#4803,.F.);
#6242=ORIENTED_EDGE('',*,*,#4804,.T.);
#6243=ORIENTED_EDGE('',*,*,#4800,.T.);
#6244=ORIENTED_EDGE('',*,*,#4805,.F.);
#6245=ORIENTED_EDGE('',*,*,#4806,.F.);
#6246=ORIENTED_EDGE('',*,*,#4807,.T.);
#6247=ORIENTED_EDGE('',*,*,#4803,.T.);
#6248=ORIENTED_EDGE('',*,*,#4808,.F.);
#6249=ORIENTED_EDGE('',*,*,#4809,.F.);
#6250=ORIENTED_EDGE('',*,*,#4810,.T.);
#6251=ORIENTED_EDGE('',*,*,#4806,.T.);
#6252=ORIENTED_EDGE('',*,*,#4811,.F.);
#6253=ORIENTED_EDGE('',*,*,#4812,.F.);
#6254=ORIENTED_EDGE('',*,*,#4813,.T.);
#6255=ORIENTED_EDGE('',*,*,#4809,.T.);
#6256=ORIENTED_EDGE('',*,*,#4814,.F.);
#6257=ORIENTED_EDGE('',*,*,#4815,.F.);
#6258=ORIENTED_EDGE('',*,*,#4816,.T.);
#6259=ORIENTED_EDGE('',*,*,#4812,.T.);
#6260=ORIENTED_EDGE('',*,*,#4817,.F.);
#6261=ORIENTED_EDGE('',*,*,#4818,.F.);
#6262=ORIENTED_EDGE('',*,*,#4819,.T.);
#6263=ORIENTED_EDGE('',*,*,#4815,.T.);
#6264=ORIENTED_EDGE('',*,*,#4820,.F.);
#6265=ORIENTED_EDGE('',*,*,#4821,.F.);
#6266=ORIENTED_EDGE('',*,*,#4822,.T.);
#6267=ORIENTED_EDGE('',*,*,#4818,.T.);
#6268=ORIENTED_EDGE('',*,*,#4823,.F.);
#6269=ORIENTED_EDGE('',*,*,#4824,.F.);
#6270=ORIENTED_EDGE('',*,*,#4825,.T.);
#6271=ORIENTED_EDGE('',*,*,#4821,.T.);
#6272=ORIENTED_EDGE('',*,*,#4826,.F.);
#6273=ORIENTED_EDGE('',*,*,#4827,.F.);
#6274=ORIENTED_EDGE('',*,*,#4828,.T.);
#6275=ORIENTED_EDGE('',*,*,#4824,.T.);
#6276=ORIENTED_EDGE('',*,*,#4829,.F.);
#6277=ORIENTED_EDGE('',*,*,#4830,.F.);
#6278=ORIENTED_EDGE('',*,*,#4831,.T.);
#6279=ORIENTED_EDGE('',*,*,#4827,.T.);
#6280=ORIENTED_EDGE('',*,*,#4832,.F.);
#6281=ORIENTED_EDGE('',*,*,#4833,.F.);
#6282=ORIENTED_EDGE('',*,*,#4834,.T.);
#6283=ORIENTED_EDGE('',*,*,#4830,.T.);
#6284=ORIENTED_EDGE('',*,*,#4835,.F.);
#6285=ORIENTED_EDGE('',*,*,#4836,.F.);
#6286=ORIENTED_EDGE('',*,*,#4837,.T.);
#6287=ORIENTED_EDGE('',*,*,#4833,.T.);
#6288=ORIENTED_EDGE('',*,*,#4838,.F.);
#6289=ORIENTED_EDGE('',*,*,#4839,.F.);
#6290=ORIENTED_EDGE('',*,*,#4840,.T.);
#6291=ORIENTED_EDGE('',*,*,#4836,.T.);
#6292=ORIENTED_EDGE('',*,*,#4841,.F.);
#6293=ORIENTED_EDGE('',*,*,#4842,.F.);
#6294=ORIENTED_EDGE('',*,*,#4843,.T.);
#6295=ORIENTED_EDGE('',*,*,#4839,.T.);
#6296=ORIENTED_EDGE('',*,*,#4844,.F.);
#6297=ORIENTED_EDGE('',*,*,#4845,.F.);
#6298=ORIENTED_EDGE('',*,*,#4846,.T.);
#6299=ORIENTED_EDGE('',*,*,#4842,.T.);
#6300=ORIENTED_EDGE('',*,*,#4847,.F.);
#6301=ORIENTED_EDGE('',*,*,#4848,.F.);
#6302=ORIENTED_EDGE('',*,*,#4849,.T.);
#6303=ORIENTED_EDGE('',*,*,#4845,.T.);
#6304=ORIENTED_EDGE('',*,*,#4850,.F.);
#6305=ORIENTED_EDGE('',*,*,#4851,.F.);
#6306=ORIENTED_EDGE('',*,*,#4852,.T.);
#6307=ORIENTED_EDGE('',*,*,#4848,.T.);
#6308=ORIENTED_EDGE('',*,*,#4853,.F.);
#6309=ORIENTED_EDGE('',*,*,#4854,.F.);
#6310=ORIENTED_EDGE('',*,*,#4855,.T.);
#6311=ORIENTED_EDGE('',*,*,#4851,.T.);
#6312=ORIENTED_EDGE('',*,*,#4856,.F.);
#6313=ORIENTED_EDGE('',*,*,#4857,.F.);
#6314=ORIENTED_EDGE('',*,*,#4858,.T.);
#6315=ORIENTED_EDGE('',*,*,#4854,.T.);
#6316=ORIENTED_EDGE('',*,*,#4859,.F.);
#6317=ORIENTED_EDGE('',*,*,#4860,.F.);
#6318=ORIENTED_EDGE('',*,*,#4861,.T.);
#6319=ORIENTED_EDGE('',*,*,#4857,.T.);
#6320=ORIENTED_EDGE('',*,*,#4862,.F.);
#6321=ORIENTED_EDGE('',*,*,#4863,.F.);
#6322=ORIENTED_EDGE('',*,*,#4864,.T.);
#6323=ORIENTED_EDGE('',*,*,#4860,.T.);
#6324=ORIENTED_EDGE('',*,*,#4865,.F.);
#6325=ORIENTED_EDGE('',*,*,#4866,.F.);
#6326=ORIENTED_EDGE('',*,*,#4867,.T.);
#6327=ORIENTED_EDGE('',*,*,#4868,.F.);
#6328=ORIENTED_EDGE('',*,*,#4867,.F.);
#6329=ORIENTED_EDGE('',*,*,#4869,.F.);
#6330=ORIENTED_EDGE('',*,*,#4870,.T.);
#6331=ORIENTED_EDGE('',*,*,#4871,.F.);
#6332=ORIENTED_EDGE('',*,*,#4870,.F.);
#6333=ORIENTED_EDGE('',*,*,#4872,.F.);
#6334=ORIENTED_EDGE('',*,*,#4873,.T.);
#6335=ORIENTED_EDGE('',*,*,#4874,.F.);
#6336=ORIENTED_EDGE('',*,*,#4873,.F.);
#6337=ORIENTED_EDGE('',*,*,#4875,.F.);
#6338=ORIENTED_EDGE('',*,*,#4876,.T.);
#6339=ORIENTED_EDGE('',*,*,#4877,.F.);
#6340=ORIENTED_EDGE('',*,*,#4876,.F.);
#6341=ORIENTED_EDGE('',*,*,#4878,.F.);
#6342=ORIENTED_EDGE('',*,*,#4879,.T.);
#6343=ORIENTED_EDGE('',*,*,#4880,.F.);
#6344=ORIENTED_EDGE('',*,*,#4879,.F.);
#6345=ORIENTED_EDGE('',*,*,#4881,.F.);
#6346=ORIENTED_EDGE('',*,*,#4882,.T.);
#6347=ORIENTED_EDGE('',*,*,#4883,.F.);
#6348=ORIENTED_EDGE('',*,*,#4882,.F.);
#6349=ORIENTED_EDGE('',*,*,#4884,.T.);
#6350=ORIENTED_EDGE('',*,*,#4868,.T.);
#6351=ORIENTED_EDGE('',*,*,#4871,.T.);
#6352=ORIENTED_EDGE('',*,*,#4885,.T.);
#6353=ORIENTED_EDGE('',*,*,#4302,.F.);
#6354=ORIENTED_EDGE('',*,*,#4886,.T.);
#6355=ORIENTED_EDGE('',*,*,#4887,.T.);
#6356=ORIENTED_EDGE('',*,*,#4883,.T.);
#6357=ORIENTED_EDGE('',*,*,#4880,.T.);
#6358=ORIENTED_EDGE('',*,*,#4877,.T.);
#6359=ORIENTED_EDGE('',*,*,#4874,.T.);
#6360=ORIENTED_EDGE('',*,*,#4884,.F.);
#6361=ORIENTED_EDGE('',*,*,#4888,.T.);
#6362=ORIENTED_EDGE('',*,*,#4889,.T.);
#6363=ORIENTED_EDGE('',*,*,#4888,.F.);
#6364=ORIENTED_EDGE('',*,*,#4889,.F.);
#6365=ORIENTED_EDGE('',*,*,#4866,.T.);
#6366=ORIENTED_EDGE('',*,*,#4869,.T.);
#6367=ORIENTED_EDGE('',*,*,#4872,.T.);
#6368=ORIENTED_EDGE('',*,*,#4875,.T.);
#6369=ORIENTED_EDGE('',*,*,#4878,.T.);
#6370=ORIENTED_EDGE('',*,*,#4881,.T.);
#6371=ORIENTED_EDGE('',*,*,#4890,.F.);
#6372=ORIENTED_EDGE('',*,*,#4891,.F.);
#6373=ORIENTED_EDGE('',*,*,#4582,.F.);
#6374=ORIENTED_EDGE('',*,*,#4579,.F.);
#6375=ORIENTED_EDGE('',*,*,#4576,.F.);
#6376=ORIENTED_EDGE('',*,*,#4573,.F.);
#6377=ORIENTED_EDGE('',*,*,#4570,.F.);
#6378=ORIENTED_EDGE('',*,*,#4567,.F.);
#6379=ORIENTED_EDGE('',*,*,#4564,.F.);
#6380=ORIENTED_EDGE('',*,*,#4561,.F.);
#6381=ORIENTED_EDGE('',*,*,#4558,.F.);
#6382=ORIENTED_EDGE('',*,*,#4555,.F.);
#6383=ORIENTED_EDGE('',*,*,#4552,.F.);
#6384=ORIENTED_EDGE('',*,*,#4549,.F.);
#6385=ORIENTED_EDGE('',*,*,#4546,.F.);
#6386=ORIENTED_EDGE('',*,*,#4543,.F.);
#6387=ORIENTED_EDGE('',*,*,#4540,.F.);
#6388=ORIENTED_EDGE('',*,*,#4537,.F.);
#6389=ORIENTED_EDGE('',*,*,#4534,.F.);
#6390=ORIENTED_EDGE('',*,*,#4531,.F.);
#6391=ORIENTED_EDGE('',*,*,#4528,.F.);
#6392=ORIENTED_EDGE('',*,*,#4525,.F.);
#6393=ORIENTED_EDGE('',*,*,#4522,.F.);
#6394=ORIENTED_EDGE('',*,*,#4519,.F.);
#6395=ORIENTED_EDGE('',*,*,#4516,.F.);
#6396=ORIENTED_EDGE('',*,*,#4513,.F.);
#6397=ORIENTED_EDGE('',*,*,#4510,.F.);
#6398=ORIENTED_EDGE('',*,*,#4507,.F.);
#6399=ORIENTED_EDGE('',*,*,#4504,.F.);
#6400=ORIENTED_EDGE('',*,*,#4501,.F.);
#6401=ORIENTED_EDGE('',*,*,#4498,.F.);
#6402=ORIENTED_EDGE('',*,*,#4495,.F.);
#6403=ORIENTED_EDGE('',*,*,#4492,.F.);
#6404=ORIENTED_EDGE('',*,*,#4489,.F.);
#6405=ORIENTED_EDGE('',*,*,#4486,.F.);
#6406=ORIENTED_EDGE('',*,*,#4483,.F.);
#6407=ORIENTED_EDGE('',*,*,#4480,.F.);
#6408=ORIENTED_EDGE('',*,*,#4477,.F.);
#6409=ORIENTED_EDGE('',*,*,#4474,.F.);
#6410=ORIENTED_EDGE('',*,*,#4471,.F.);
#6411=ORIENTED_EDGE('',*,*,#4468,.F.);
#6412=ORIENTED_EDGE('',*,*,#4465,.F.);
#6413=ORIENTED_EDGE('',*,*,#4462,.F.);
#6414=ORIENTED_EDGE('',*,*,#4459,.F.);
#6415=ORIENTED_EDGE('',*,*,#4456,.F.);
#6416=ORIENTED_EDGE('',*,*,#4453,.F.);
#6417=ORIENTED_EDGE('',*,*,#4450,.F.);
#6418=ORIENTED_EDGE('',*,*,#4447,.F.);
#6419=ORIENTED_EDGE('',*,*,#4444,.F.);
#6420=ORIENTED_EDGE('',*,*,#4441,.F.);
#6421=ORIENTED_EDGE('',*,*,#4438,.F.);
#6422=ORIENTED_EDGE('',*,*,#4435,.F.);
#6423=ORIENTED_EDGE('',*,*,#4432,.F.);
#6424=ORIENTED_EDGE('',*,*,#4429,.F.);
#6425=ORIENTED_EDGE('',*,*,#4426,.F.);
#6426=ORIENTED_EDGE('',*,*,#4423,.F.);
#6427=ORIENTED_EDGE('',*,*,#4420,.F.);
#6428=ORIENTED_EDGE('',*,*,#4417,.F.);
#6429=ORIENTED_EDGE('',*,*,#4414,.F.);
#6430=ORIENTED_EDGE('',*,*,#4411,.F.);
#6431=ORIENTED_EDGE('',*,*,#4408,.F.);
#6432=ORIENTED_EDGE('',*,*,#4405,.F.);
#6433=ORIENTED_EDGE('',*,*,#4402,.F.);
#6434=ORIENTED_EDGE('',*,*,#4399,.F.);
#6435=ORIENTED_EDGE('',*,*,#4396,.F.);
#6436=ORIENTED_EDGE('',*,*,#4393,.F.);
#6437=ORIENTED_EDGE('',*,*,#4390,.F.);
#6438=ORIENTED_EDGE('',*,*,#4387,.F.);
#6439=ORIENTED_EDGE('',*,*,#4384,.F.);
#6440=ORIENTED_EDGE('',*,*,#4381,.F.);
#6441=ORIENTED_EDGE('',*,*,#4378,.F.);
#6442=ORIENTED_EDGE('',*,*,#4375,.F.);
#6443=ORIENTED_EDGE('',*,*,#4372,.F.);
#6444=ORIENTED_EDGE('',*,*,#4369,.F.);
#6445=ORIENTED_EDGE('',*,*,#4366,.F.);
#6446=ORIENTED_EDGE('',*,*,#4363,.F.);
#6447=ORIENTED_EDGE('',*,*,#4360,.F.);
#6448=ORIENTED_EDGE('',*,*,#4357,.F.);
#6449=ORIENTED_EDGE('',*,*,#4354,.F.);
#6450=ORIENTED_EDGE('',*,*,#4351,.F.);
#6451=ORIENTED_EDGE('',*,*,#4348,.F.);
#6452=ORIENTED_EDGE('',*,*,#4345,.F.);
#6453=ORIENTED_EDGE('',*,*,#4342,.F.);
#6454=ORIENTED_EDGE('',*,*,#4339,.F.);
#6455=ORIENTED_EDGE('',*,*,#4336,.F.);
#6456=ORIENTED_EDGE('',*,*,#4333,.F.);
#6457=ORIENTED_EDGE('',*,*,#4330,.F.);
#6458=ORIENTED_EDGE('',*,*,#4327,.F.);
#6459=ORIENTED_EDGE('',*,*,#4324,.F.);
#6460=ORIENTED_EDGE('',*,*,#4321,.F.);
#6461=ORIENTED_EDGE('',*,*,#4318,.F.);
#6462=ORIENTED_EDGE('',*,*,#4315,.F.);
#6463=ORIENTED_EDGE('',*,*,#4312,.F.);
#6464=ORIENTED_EDGE('',*,*,#4309,.F.);
#6465=ORIENTED_EDGE('',*,*,#4306,.F.);
#6466=ORIENTED_EDGE('',*,*,#4303,.F.);
#6467=ORIENTED_EDGE('',*,*,#4885,.F.);
#6468=ORIENTED_EDGE('',*,*,#4892,.T.);
#6469=ORIENTED_EDGE('',*,*,#4865,.T.);
#6470=ORIENTED_EDGE('',*,*,#4862,.T.);
#6471=ORIENTED_EDGE('',*,*,#4859,.T.);
#6472=ORIENTED_EDGE('',*,*,#4856,.T.);
#6473=ORIENTED_EDGE('',*,*,#4853,.T.);
#6474=ORIENTED_EDGE('',*,*,#4850,.T.);
#6475=ORIENTED_EDGE('',*,*,#4847,.T.);
#6476=ORIENTED_EDGE('',*,*,#4844,.T.);
#6477=ORIENTED_EDGE('',*,*,#4841,.T.);
#6478=ORIENTED_EDGE('',*,*,#4838,.T.);
#6479=ORIENTED_EDGE('',*,*,#4835,.T.);
#6480=ORIENTED_EDGE('',*,*,#4832,.T.);
#6481=ORIENTED_EDGE('',*,*,#4829,.T.);
#6482=ORIENTED_EDGE('',*,*,#4826,.T.);
#6483=ORIENTED_EDGE('',*,*,#4823,.T.);
#6484=ORIENTED_EDGE('',*,*,#4820,.T.);
#6485=ORIENTED_EDGE('',*,*,#4817,.T.);
#6486=ORIENTED_EDGE('',*,*,#4814,.T.);
#6487=ORIENTED_EDGE('',*,*,#4811,.T.);
#6488=ORIENTED_EDGE('',*,*,#4808,.T.);
#6489=ORIENTED_EDGE('',*,*,#4805,.T.);
#6490=ORIENTED_EDGE('',*,*,#4802,.T.);
#6491=ORIENTED_EDGE('',*,*,#4799,.T.);
#6492=ORIENTED_EDGE('',*,*,#4796,.T.);
#6493=ORIENTED_EDGE('',*,*,#4793,.T.);
#6494=ORIENTED_EDGE('',*,*,#4790,.T.);
#6495=ORIENTED_EDGE('',*,*,#4787,.T.);
#6496=ORIENTED_EDGE('',*,*,#4784,.T.);
#6497=ORIENTED_EDGE('',*,*,#4781,.T.);
#6498=ORIENTED_EDGE('',*,*,#4778,.T.);
#6499=ORIENTED_EDGE('',*,*,#4775,.T.);
#6500=ORIENTED_EDGE('',*,*,#4772,.T.);
#6501=ORIENTED_EDGE('',*,*,#4769,.T.);
#6502=ORIENTED_EDGE('',*,*,#4766,.T.);
#6503=ORIENTED_EDGE('',*,*,#4763,.T.);
#6504=ORIENTED_EDGE('',*,*,#4760,.T.);
#6505=ORIENTED_EDGE('',*,*,#4757,.T.);
#6506=ORIENTED_EDGE('',*,*,#4754,.T.);
#6507=ORIENTED_EDGE('',*,*,#4751,.T.);
#6508=ORIENTED_EDGE('',*,*,#4748,.T.);
#6509=ORIENTED_EDGE('',*,*,#4745,.T.);
#6510=ORIENTED_EDGE('',*,*,#4742,.T.);
#6511=ORIENTED_EDGE('',*,*,#4739,.T.);
#6512=ORIENTED_EDGE('',*,*,#4736,.T.);
#6513=ORIENTED_EDGE('',*,*,#4733,.T.);
#6514=ORIENTED_EDGE('',*,*,#4730,.T.);
#6515=ORIENTED_EDGE('',*,*,#4727,.T.);
#6516=ORIENTED_EDGE('',*,*,#4724,.T.);
#6517=ORIENTED_EDGE('',*,*,#4721,.T.);
#6518=ORIENTED_EDGE('',*,*,#4718,.T.);
#6519=ORIENTED_EDGE('',*,*,#4715,.T.);
#6520=ORIENTED_EDGE('',*,*,#4712,.T.);
#6521=ORIENTED_EDGE('',*,*,#4709,.T.);
#6522=ORIENTED_EDGE('',*,*,#4706,.T.);
#6523=ORIENTED_EDGE('',*,*,#4703,.T.);
#6524=ORIENTED_EDGE('',*,*,#4700,.T.);
#6525=ORIENTED_EDGE('',*,*,#4697,.T.);
#6526=ORIENTED_EDGE('',*,*,#4694,.T.);
#6527=ORIENTED_EDGE('',*,*,#4691,.T.);
#6528=ORIENTED_EDGE('',*,*,#4688,.T.);
#6529=ORIENTED_EDGE('',*,*,#4685,.T.);
#6530=ORIENTED_EDGE('',*,*,#4682,.T.);
#6531=ORIENTED_EDGE('',*,*,#4679,.T.);
#6532=ORIENTED_EDGE('',*,*,#4676,.T.);
#6533=ORIENTED_EDGE('',*,*,#4673,.T.);
#6534=ORIENTED_EDGE('',*,*,#4670,.T.);
#6535=ORIENTED_EDGE('',*,*,#4667,.T.);
#6536=ORIENTED_EDGE('',*,*,#4664,.T.);
#6537=ORIENTED_EDGE('',*,*,#4661,.T.);
#6538=ORIENTED_EDGE('',*,*,#4658,.T.);
#6539=ORIENTED_EDGE('',*,*,#4655,.T.);
#6540=ORIENTED_EDGE('',*,*,#4652,.T.);
#6541=ORIENTED_EDGE('',*,*,#4649,.T.);
#6542=ORIENTED_EDGE('',*,*,#4646,.T.);
#6543=ORIENTED_EDGE('',*,*,#4643,.T.);
#6544=ORIENTED_EDGE('',*,*,#4640,.T.);
#6545=ORIENTED_EDGE('',*,*,#4637,.T.);
#6546=ORIENTED_EDGE('',*,*,#4634,.T.);
#6547=ORIENTED_EDGE('',*,*,#4631,.T.);
#6548=ORIENTED_EDGE('',*,*,#4628,.T.);
#6549=ORIENTED_EDGE('',*,*,#4625,.T.);
#6550=ORIENTED_EDGE('',*,*,#4622,.T.);
#6551=ORIENTED_EDGE('',*,*,#4619,.T.);
#6552=ORIENTED_EDGE('',*,*,#4616,.T.);
#6553=ORIENTED_EDGE('',*,*,#4613,.T.);
#6554=ORIENTED_EDGE('',*,*,#4610,.T.);
#6555=ORIENTED_EDGE('',*,*,#4607,.T.);
#6556=ORIENTED_EDGE('',*,*,#4604,.T.);
#6557=ORIENTED_EDGE('',*,*,#4601,.T.);
#6558=ORIENTED_EDGE('',*,*,#4598,.T.);
#6559=ORIENTED_EDGE('',*,*,#4595,.T.);
#6560=ORIENTED_EDGE('',*,*,#4592,.T.);
#6561=ORIENTED_EDGE('',*,*,#4589,.T.);
#6562=ORIENTED_EDGE('',*,*,#4586,.T.);
#6563=ORIENTED_EDGE('',*,*,#4863,.T.);
#6564=ORIENTED_EDGE('',*,*,#4892,.F.);
#6565=ORIENTED_EDGE('',*,*,#4887,.F.);
#6566=ORIENTED_EDGE('',*,*,#4893,.T.);
#6567=ORIENTED_EDGE('',*,*,#4894,.F.);
#6568=ORIENTED_EDGE('',*,*,#4584,.F.);
#6569=ORIENTED_EDGE('',*,*,#4588,.F.);
#6570=ORIENTED_EDGE('',*,*,#4591,.F.);
#6571=ORIENTED_EDGE('',*,*,#4594,.F.);
#6572=ORIENTED_EDGE('',*,*,#4597,.F.);
#6573=ORIENTED_EDGE('',*,*,#4600,.F.);
#6574=ORIENTED_EDGE('',*,*,#4603,.F.);
#6575=ORIENTED_EDGE('',*,*,#4606,.F.);
#6576=ORIENTED_EDGE('',*,*,#4609,.F.);
#6577=ORIENTED_EDGE('',*,*,#4612,.F.);
#6578=ORIENTED_EDGE('',*,*,#4615,.F.);
#6579=ORIENTED_EDGE('',*,*,#4618,.F.);
#6580=ORIENTED_EDGE('',*,*,#4621,.F.);
#6581=ORIENTED_EDGE('',*,*,#4624,.F.);
#6582=ORIENTED_EDGE('',*,*,#4627,.F.);
#6583=ORIENTED_EDGE('',*,*,#4630,.F.);
#6584=ORIENTED_EDGE('',*,*,#4633,.F.);
#6585=ORIENTED_EDGE('',*,*,#4636,.F.);
#6586=ORIENTED_EDGE('',*,*,#4639,.F.);
#6587=ORIENTED_EDGE('',*,*,#4642,.F.);
#6588=ORIENTED_EDGE('',*,*,#4645,.F.);
#6589=ORIENTED_EDGE('',*,*,#4648,.F.);
#6590=ORIENTED_EDGE('',*,*,#4651,.F.);
#6591=ORIENTED_EDGE('',*,*,#4654,.F.);
#6592=ORIENTED_EDGE('',*,*,#4657,.F.);
#6593=ORIENTED_EDGE('',*,*,#4660,.F.);
#6594=ORIENTED_EDGE('',*,*,#4663,.F.);
#6595=ORIENTED_EDGE('',*,*,#4666,.F.);
#6596=ORIENTED_EDGE('',*,*,#4669,.F.);
#6597=ORIENTED_EDGE('',*,*,#4672,.F.);
#6598=ORIENTED_EDGE('',*,*,#4675,.F.);
#6599=ORIENTED_EDGE('',*,*,#4678,.F.);
#6600=ORIENTED_EDGE('',*,*,#4681,.F.);
#6601=ORIENTED_EDGE('',*,*,#4684,.F.);
#6602=ORIENTED_EDGE('',*,*,#4687,.F.);
#6603=ORIENTED_EDGE('',*,*,#4690,.F.);
#6604=ORIENTED_EDGE('',*,*,#4693,.F.);
#6605=ORIENTED_EDGE('',*,*,#4696,.F.);
#6606=ORIENTED_EDGE('',*,*,#4699,.F.);
#6607=ORIENTED_EDGE('',*,*,#4702,.F.);
#6608=ORIENTED_EDGE('',*,*,#4705,.F.);
#6609=ORIENTED_EDGE('',*,*,#4708,.F.);
#6610=ORIENTED_EDGE('',*,*,#4711,.F.);
#6611=ORIENTED_EDGE('',*,*,#4714,.F.);
#6612=ORIENTED_EDGE('',*,*,#4717,.F.);
#6613=ORIENTED_EDGE('',*,*,#4720,.F.);
#6614=ORIENTED_EDGE('',*,*,#4723,.F.);
#6615=ORIENTED_EDGE('',*,*,#4726,.F.);
#6616=ORIENTED_EDGE('',*,*,#4729,.F.);
#6617=ORIENTED_EDGE('',*,*,#4732,.F.);
#6618=ORIENTED_EDGE('',*,*,#4735,.F.);
#6619=ORIENTED_EDGE('',*,*,#4738,.F.);
#6620=ORIENTED_EDGE('',*,*,#4741,.F.);
#6621=ORIENTED_EDGE('',*,*,#4744,.F.);
#6622=ORIENTED_EDGE('',*,*,#4747,.F.);
#6623=ORIENTED_EDGE('',*,*,#4750,.F.);
#6624=ORIENTED_EDGE('',*,*,#4753,.F.);
#6625=ORIENTED_EDGE('',*,*,#4756,.F.);
#6626=ORIENTED_EDGE('',*,*,#4759,.F.);
#6627=ORIENTED_EDGE('',*,*,#4762,.F.);
#6628=ORIENTED_EDGE('',*,*,#4765,.F.);
#6629=ORIENTED_EDGE('',*,*,#4768,.F.);
#6630=ORIENTED_EDGE('',*,*,#4771,.F.);
#6631=ORIENTED_EDGE('',*,*,#4774,.F.);
#6632=ORIENTED_EDGE('',*,*,#4777,.F.);
#6633=ORIENTED_EDGE('',*,*,#4780,.F.);
#6634=ORIENTED_EDGE('',*,*,#4783,.F.);
#6635=ORIENTED_EDGE('',*,*,#4786,.F.);
#6636=ORIENTED_EDGE('',*,*,#4789,.F.);
#6637=ORIENTED_EDGE('',*,*,#4792,.F.);
#6638=ORIENTED_EDGE('',*,*,#4795,.F.);
#6639=ORIENTED_EDGE('',*,*,#4798,.F.);
#6640=ORIENTED_EDGE('',*,*,#4801,.F.);
#6641=ORIENTED_EDGE('',*,*,#4804,.F.);
#6642=ORIENTED_EDGE('',*,*,#4807,.F.);
#6643=ORIENTED_EDGE('',*,*,#4810,.F.);
#6644=ORIENTED_EDGE('',*,*,#4813,.F.);
#6645=ORIENTED_EDGE('',*,*,#4816,.F.);
#6646=ORIENTED_EDGE('',*,*,#4819,.F.);
#6647=ORIENTED_EDGE('',*,*,#4822,.F.);
#6648=ORIENTED_EDGE('',*,*,#4825,.F.);
#6649=ORIENTED_EDGE('',*,*,#4828,.F.);
#6650=ORIENTED_EDGE('',*,*,#4831,.F.);
#6651=ORIENTED_EDGE('',*,*,#4834,.F.);
#6652=ORIENTED_EDGE('',*,*,#4837,.F.);
#6653=ORIENTED_EDGE('',*,*,#4840,.F.);
#6654=ORIENTED_EDGE('',*,*,#4843,.F.);
#6655=ORIENTED_EDGE('',*,*,#4846,.F.);
#6656=ORIENTED_EDGE('',*,*,#4849,.F.);
#6657=ORIENTED_EDGE('',*,*,#4852,.F.);
#6658=ORIENTED_EDGE('',*,*,#4855,.F.);
#6659=ORIENTED_EDGE('',*,*,#4858,.F.);
#6660=ORIENTED_EDGE('',*,*,#4861,.F.);
#6661=ORIENTED_EDGE('',*,*,#4864,.F.);
#6662=ORIENTED_EDGE('',*,*,#4893,.F.);
#6663=ORIENTED_EDGE('',*,*,#4886,.F.);
#6664=ORIENTED_EDGE('',*,*,#4301,.F.);
#6665=ORIENTED_EDGE('',*,*,#4305,.F.);
#6666=ORIENTED_EDGE('',*,*,#4308,.F.);
#6667=ORIENTED_EDGE('',*,*,#4311,.F.);
#6668=ORIENTED_EDGE('',*,*,#4314,.F.);
#6669=ORIENTED_EDGE('',*,*,#4317,.F.);
#6670=ORIENTED_EDGE('',*,*,#4320,.F.);
#6671=ORIENTED_EDGE('',*,*,#4323,.F.);
#6672=ORIENTED_EDGE('',*,*,#4326,.F.);
#6673=ORIENTED_EDGE('',*,*,#4329,.F.);
#6674=ORIENTED_EDGE('',*,*,#4332,.F.);
#6675=ORIENTED_EDGE('',*,*,#4335,.F.);
#6676=ORIENTED_EDGE('',*,*,#4338,.F.);
#6677=ORIENTED_EDGE('',*,*,#4341,.F.);
#6678=ORIENTED_EDGE('',*,*,#4344,.F.);
#6679=ORIENTED_EDGE('',*,*,#4347,.F.);
#6680=ORIENTED_EDGE('',*,*,#4350,.F.);
#6681=ORIENTED_EDGE('',*,*,#4353,.F.);
#6682=ORIENTED_EDGE('',*,*,#4356,.F.);
#6683=ORIENTED_EDGE('',*,*,#4359,.F.);
#6684=ORIENTED_EDGE('',*,*,#4362,.F.);
#6685=ORIENTED_EDGE('',*,*,#4365,.F.);
#6686=ORIENTED_EDGE('',*,*,#4368,.F.);
#6687=ORIENTED_EDGE('',*,*,#4371,.F.);
#6688=ORIENTED_EDGE('',*,*,#4374,.F.);
#6689=ORIENTED_EDGE('',*,*,#4377,.F.);
#6690=ORIENTED_EDGE('',*,*,#4380,.F.);
#6691=ORIENTED_EDGE('',*,*,#4383,.F.);
#6692=ORIENTED_EDGE('',*,*,#4386,.F.);
#6693=ORIENTED_EDGE('',*,*,#4389,.F.);
#6694=ORIENTED_EDGE('',*,*,#4392,.F.);
#6695=ORIENTED_EDGE('',*,*,#4395,.F.);
#6696=ORIENTED_EDGE('',*,*,#4398,.F.);
#6697=ORIENTED_EDGE('',*,*,#4401,.F.);
#6698=ORIENTED_EDGE('',*,*,#4404,.F.);
#6699=ORIENTED_EDGE('',*,*,#4407,.F.);
#6700=ORIENTED_EDGE('',*,*,#4410,.F.);
#6701=ORIENTED_EDGE('',*,*,#4413,.F.);
#6702=ORIENTED_EDGE('',*,*,#4416,.F.);
#6703=ORIENTED_EDGE('',*,*,#4419,.F.);
#6704=ORIENTED_EDGE('',*,*,#4422,.F.);
#6705=ORIENTED_EDGE('',*,*,#4425,.F.);
#6706=ORIENTED_EDGE('',*,*,#4428,.F.);
#6707=ORIENTED_EDGE('',*,*,#4431,.F.);
#6708=ORIENTED_EDGE('',*,*,#4434,.F.);
#6709=ORIENTED_EDGE('',*,*,#4437,.F.);
#6710=ORIENTED_EDGE('',*,*,#4440,.F.);
#6711=ORIENTED_EDGE('',*,*,#4443,.F.);
#6712=ORIENTED_EDGE('',*,*,#4446,.F.);
#6713=ORIENTED_EDGE('',*,*,#4449,.F.);
#6714=ORIENTED_EDGE('',*,*,#4452,.F.);
#6715=ORIENTED_EDGE('',*,*,#4455,.F.);
#6716=ORIENTED_EDGE('',*,*,#4458,.F.);
#6717=ORIENTED_EDGE('',*,*,#4461,.F.);
#6718=ORIENTED_EDGE('',*,*,#4464,.F.);
#6719=ORIENTED_EDGE('',*,*,#4467,.F.);
#6720=ORIENTED_EDGE('',*,*,#4470,.F.);
#6721=ORIENTED_EDGE('',*,*,#4473,.F.);
#6722=ORIENTED_EDGE('',*,*,#4476,.F.);
#6723=ORIENTED_EDGE('',*,*,#4479,.F.);
#6724=ORIENTED_EDGE('',*,*,#4482,.F.);
#6725=ORIENTED_EDGE('',*,*,#4485,.F.);
#6726=ORIENTED_EDGE('',*,*,#4488,.F.);
#6727=ORIENTED_EDGE('',*,*,#4491,.F.);
#6728=ORIENTED_EDGE('',*,*,#4494,.F.);
#6729=ORIENTED_EDGE('',*,*,#4497,.F.);
#6730=ORIENTED_EDGE('',*,*,#4500,.F.);
#6731=ORIENTED_EDGE('',*,*,#4503,.F.);
#6732=ORIENTED_EDGE('',*,*,#4506,.F.);
#6733=ORIENTED_EDGE('',*,*,#4509,.F.);
#6734=ORIENTED_EDGE('',*,*,#4512,.F.);
#6735=ORIENTED_EDGE('',*,*,#4515,.F.);
#6736=ORIENTED_EDGE('',*,*,#4518,.F.);
#6737=ORIENTED_EDGE('',*,*,#4521,.F.);
#6738=ORIENTED_EDGE('',*,*,#4524,.F.);
#6739=ORIENTED_EDGE('',*,*,#4527,.F.);
#6740=ORIENTED_EDGE('',*,*,#4530,.F.);
#6741=ORIENTED_EDGE('',*,*,#4533,.F.);
#6742=ORIENTED_EDGE('',*,*,#4536,.F.);
#6743=ORIENTED_EDGE('',*,*,#4539,.F.);
#6744=ORIENTED_EDGE('',*,*,#4542,.F.);
#6745=ORIENTED_EDGE('',*,*,#4545,.F.);
#6746=ORIENTED_EDGE('',*,*,#4548,.F.);
#6747=ORIENTED_EDGE('',*,*,#4551,.F.);
#6748=ORIENTED_EDGE('',*,*,#4554,.F.);
#6749=ORIENTED_EDGE('',*,*,#4557,.F.);
#6750=ORIENTED_EDGE('',*,*,#4560,.F.);
#6751=ORIENTED_EDGE('',*,*,#4563,.F.);
#6752=ORIENTED_EDGE('',*,*,#4566,.F.);
#6753=ORIENTED_EDGE('',*,*,#4569,.F.);
#6754=ORIENTED_EDGE('',*,*,#4572,.F.);
#6755=ORIENTED_EDGE('',*,*,#4575,.F.);
#6756=ORIENTED_EDGE('',*,*,#4578,.F.);
#6757=ORIENTED_EDGE('',*,*,#4581,.F.);
#6758=ORIENTED_EDGE('',*,*,#4895,.F.);
#6759=ORIENTED_EDGE('',*,*,#4890,.T.);
#6760=ORIENTED_EDGE('',*,*,#4585,.T.);
#6761=ORIENTED_EDGE('',*,*,#4894,.T.);
#6762=ORIENTED_EDGE('',*,*,#4896,.T.);
#6763=ORIENTED_EDGE('',*,*,#4580,.T.);
#6764=ORIENTED_EDGE('',*,*,#4891,.T.);
#6765=ORIENTED_EDGE('',*,*,#4896,.F.);
#6766=ORIENTED_EDGE('',*,*,#4895,.T.);
#6767=ORIENTED_EDGE('',*,*,#4897,.F.);
#6768=ORIENTED_EDGE('',*,*,#4898,.T.);
#6769=ORIENTED_EDGE('',*,*,#4899,.T.);
#6770=ORIENTED_EDGE('',*,*,#4898,.F.);
#6771=ORIENTED_EDGE('',*,*,#4897,.T.);
#6772=ORIENTED_EDGE('',*,*,#4899,.F.);
#6773=ORIENTED_EDGE('',*,*,#4900,.F.);
#6774=ORIENTED_EDGE('',*,*,#4901,.T.);
#6775=ORIENTED_EDGE('',*,*,#4902,.T.);
#6776=ORIENTED_EDGE('',*,*,#4901,.F.);
#6777=ORIENTED_EDGE('',*,*,#4900,.T.);
#6778=ORIENTED_EDGE('',*,*,#4902,.F.);
#6779=ORIENTED_EDGE('',*,*,#4903,.F.);
#6780=ORIENTED_EDGE('',*,*,#4904,.F.);
#6781=ORIENTED_EDGE('',*,*,#4905,.F.);
#6782=ORIENTED_EDGE('',*,*,#4906,.F.);
#6783=ORIENTED_EDGE('',*,*,#4905,.T.);
#6784=ORIENTED_EDGE('',*,*,#4907,.T.);
#6785=ORIENTED_EDGE('',*,*,#4908,.T.);
#6786=ORIENTED_EDGE('',*,*,#4909,.T.);
#6787=ORIENTED_EDGE('',*,*,#4910,.T.);
#6788=ORIENTED_EDGE('',*,*,#4911,.T.);
#6789=ORIENTED_EDGE('',*,*,#4912,.T.);
#6790=ORIENTED_EDGE('',*,*,#4913,.T.);
#6791=ORIENTED_EDGE('',*,*,#4904,.T.);
#6792=ORIENTED_EDGE('',*,*,#4914,.F.);
#6793=ORIENTED_EDGE('',*,*,#4915,.F.);
#6794=ORIENTED_EDGE('',*,*,#4907,.F.);
#6795=ORIENTED_EDGE('',*,*,#4916,.F.);
#6796=ORIENTED_EDGE('',*,*,#4917,.T.);
#6797=ORIENTED_EDGE('',*,*,#4918,.F.);
#6798=ORIENTED_EDGE('',*,*,#4917,.F.);
#6799=ORIENTED_EDGE('',*,*,#4919,.F.);
#6800=ORIENTED_EDGE('',*,*,#4920,.F.);
#6801=ORIENTED_EDGE('',*,*,#4921,.F.);
#6802=ORIENTED_EDGE('',*,*,#4922,.T.);
#6803=ORIENTED_EDGE('',*,*,#4919,.T.);
#6804=ORIENTED_EDGE('',*,*,#4923,.T.);
#6805=ORIENTED_EDGE('',*,*,#4924,.F.);
#6806=ORIENTED_EDGE('',*,*,#4925,.T.);
#6807=ORIENTED_EDGE('',*,*,#4926,.T.);
#6808=ORIENTED_EDGE('',*,*,#4927,.F.);
#6809=ORIENTED_EDGE('',*,*,#4928,.F.);
#6810=ORIENTED_EDGE('',*,*,#4929,.F.);
#6811=ORIENTED_EDGE('',*,*,#4930,.T.);
#6812=ORIENTED_EDGE('',*,*,#4923,.F.);
#6813=ORIENTED_EDGE('',*,*,#4922,.F.);
#6814=ORIENTED_EDGE('',*,*,#4916,.T.);
#6815=ORIENTED_EDGE('',*,*,#4921,.T.);
#6816=ORIENTED_EDGE('',*,*,#4931,.T.);
#6817=ORIENTED_EDGE('',*,*,#4932,.F.);
#6818=ORIENTED_EDGE('',*,*,#4926,.F.);
#6819=ORIENTED_EDGE('',*,*,#4933,.T.);
#6820=ORIENTED_EDGE('',*,*,#4934,.T.);
#6821=ORIENTED_EDGE('',*,*,#4927,.T.);
#6822=ORIENTED_EDGE('',*,*,#4932,.T.);
#6823=ORIENTED_EDGE('',*,*,#4925,.F.);
#6824=ORIENTED_EDGE('',*,*,#4935,.F.);
#6825=ORIENTED_EDGE('',*,*,#4910,.F.);
#6826=ORIENTED_EDGE('',*,*,#4936,.T.);
#6827=ORIENTED_EDGE('',*,*,#4933,.F.);
#6828=ORIENTED_EDGE('',*,*,#4931,.F.);
#6829=ORIENTED_EDGE('',*,*,#4920,.T.);
#6830=ORIENTED_EDGE('',*,*,#4918,.T.);
#6831=ORIENTED_EDGE('',*,*,#4924,.T.);
#6832=ORIENTED_EDGE('',*,*,#4930,.F.);
#6833=ORIENTED_EDGE('',*,*,#4937,.F.);
#6834=ORIENTED_EDGE('',*,*,#4938,.F.);
#6835=ORIENTED_EDGE('',*,*,#4911,.F.);
#6836=ORIENTED_EDGE('',*,*,#4935,.T.);
#6837=ORIENTED_EDGE('',*,*,#4939,.F.);
#6838=ORIENTED_EDGE('',*,*,#4940,.F.);
#6839=ORIENTED_EDGE('',*,*,#4928,.T.);
#6840=ORIENTED_EDGE('',*,*,#4934,.F.);
#6841=ORIENTED_EDGE('',*,*,#4936,.F.);
#6842=ORIENTED_EDGE('',*,*,#4909,.F.);
#6843=ORIENTED_EDGE('',*,*,#4903,.T.);
#6844=ORIENTED_EDGE('',*,*,#4941,.T.);
#6845=ORIENTED_EDGE('',*,*,#4942,.F.);
#6846=ORIENTED_EDGE('',*,*,#4937,.T.);
#6847=ORIENTED_EDGE('',*,*,#4929,.T.);
#6848=ORIENTED_EDGE('',*,*,#4940,.T.);
#6849=ORIENTED_EDGE('',*,*,#4943,.F.);
#6850=ORIENTED_EDGE('',*,*,#4914,.T.);
#6851=ORIENTED_EDGE('',*,*,#4939,.T.);
#6852=ORIENTED_EDGE('',*,*,#4908,.F.);
#6853=ORIENTED_EDGE('',*,*,#4915,.T.);
#6854=ORIENTED_EDGE('',*,*,#4943,.T.);
#6855=ORIENTED_EDGE('',*,*,#4938,.T.);
#6856=ORIENTED_EDGE('',*,*,#4942,.T.);
#6857=ORIENTED_EDGE('',*,*,#4944,.T.);
#6858=ORIENTED_EDGE('',*,*,#4912,.F.);
#6859=ORIENTED_EDGE('',*,*,#4906,.T.);
#6860=ORIENTED_EDGE('',*,*,#4913,.F.);
#6861=ORIENTED_EDGE('',*,*,#4944,.F.);
#6862=ORIENTED_EDGE('',*,*,#4941,.F.);
#6863=ORIENTED_EDGE('',*,*,#4945,.F.);
#6864=ORIENTED_EDGE('',*,*,#4946,.T.);
#6865=ORIENTED_EDGE('',*,*,#4947,.F.);
#6866=ORIENTED_EDGE('',*,*,#4946,.F.);
#6867=ORIENTED_EDGE('',*,*,#4948,.F.);
#6868=ORIENTED_EDGE('',*,*,#4949,.T.);
#6869=ORIENTED_EDGE('',*,*,#4950,.F.);
#6870=ORIENTED_EDGE('',*,*,#4951,.F.);
#6871=ORIENTED_EDGE('',*,*,#4952,.F.);
#6872=ORIENTED_EDGE('',*,*,#4951,.T.);
#6873=ORIENTED_EDGE('',*,*,#4953,.F.);
#6874=ORIENTED_EDGE('',*,*,#4954,.F.);
#6875=ORIENTED_EDGE('',*,*,#4945,.T.);
#6876=ORIENTED_EDGE('',*,*,#4955,.F.);
#6877=ORIENTED_EDGE('',*,*,#4954,.T.);
#6878=ORIENTED_EDGE('',*,*,#4956,.F.);
#6879=ORIENTED_EDGE('',*,*,#4957,.F.);
#6880=ORIENTED_EDGE('',*,*,#4958,.F.);
#6881=ORIENTED_EDGE('',*,*,#4957,.T.);
#6882=ORIENTED_EDGE('',*,*,#4959,.F.);
#6883=ORIENTED_EDGE('',*,*,#4949,.F.);
#6884=ORIENTED_EDGE('',*,*,#4947,.T.);
#6885=ORIENTED_EDGE('',*,*,#4959,.T.);
#6886=ORIENTED_EDGE('',*,*,#4956,.T.);
#6887=ORIENTED_EDGE('',*,*,#4953,.T.);
#6888=ORIENTED_EDGE('',*,*,#4950,.T.);
#6889=ORIENTED_EDGE('',*,*,#4958,.T.);
#6890=ORIENTED_EDGE('',*,*,#4948,.T.);
#6891=ORIENTED_EDGE('',*,*,#4952,.T.);
#6892=ORIENTED_EDGE('',*,*,#4955,.T.);
#6893=ORIENTED_EDGE('',*,*,#4960,.F.);
#6894=ORIENTED_EDGE('',*,*,#4961,.T.);
#6895=ORIENTED_EDGE('',*,*,#4962,.F.);
#6896=ORIENTED_EDGE('',*,*,#4961,.F.);
#6897=ORIENTED_EDGE('',*,*,#4963,.F.);
#6898=ORIENTED_EDGE('',*,*,#4964,.T.);
#6899=ORIENTED_EDGE('',*,*,#4965,.F.);
#6900=ORIENTED_EDGE('',*,*,#4966,.F.);
#6901=ORIENTED_EDGE('',*,*,#4967,.F.);
#6902=ORIENTED_EDGE('',*,*,#4966,.T.);
#6903=ORIENTED_EDGE('',*,*,#4968,.F.);
#6904=ORIENTED_EDGE('',*,*,#4969,.F.);
#6905=ORIENTED_EDGE('',*,*,#4960,.T.);
#6906=ORIENTED_EDGE('',*,*,#4970,.F.);
#6907=ORIENTED_EDGE('',*,*,#4969,.T.);
#6908=ORIENTED_EDGE('',*,*,#4971,.F.);
#6909=ORIENTED_EDGE('',*,*,#4972,.F.);
#6910=ORIENTED_EDGE('',*,*,#4973,.F.);
#6911=ORIENTED_EDGE('',*,*,#4972,.T.);
#6912=ORIENTED_EDGE('',*,*,#4974,.F.);
#6913=ORIENTED_EDGE('',*,*,#4964,.F.);
#6914=ORIENTED_EDGE('',*,*,#4962,.T.);
#6915=ORIENTED_EDGE('',*,*,#4974,.T.);
#6916=ORIENTED_EDGE('',*,*,#4971,.T.);
#6917=ORIENTED_EDGE('',*,*,#4968,.T.);
#6918=ORIENTED_EDGE('',*,*,#4965,.T.);
#6919=ORIENTED_EDGE('',*,*,#4973,.T.);
#6920=ORIENTED_EDGE('',*,*,#4963,.T.);
#6921=ORIENTED_EDGE('',*,*,#4967,.T.);
#6922=ORIENTED_EDGE('',*,*,#4970,.T.);
#6923=ORIENTED_EDGE('',*,*,#4975,.F.);
#6924=ORIENTED_EDGE('',*,*,#4976,.F.);
#6925=ORIENTED_EDGE('',*,*,#4977,.F.);
#6926=ORIENTED_EDGE('',*,*,#4978,.F.);
#6927=ORIENTED_EDGE('',*,*,#4976,.T.);
#6928=ORIENTED_EDGE('',*,*,#4979,.T.);
#6929=ORIENTED_EDGE('',*,*,#4980,.T.);
#6930=ORIENTED_EDGE('',*,*,#4981,.T.);
#6931=ORIENTED_EDGE('',*,*,#4975,.T.);
#6932=ORIENTED_EDGE('',*,*,#4982,.F.);
#6933=ORIENTED_EDGE('',*,*,#4983,.F.);
#6934=ORIENTED_EDGE('',*,*,#4979,.F.);
#6935=ORIENTED_EDGE('',*,*,#4977,.T.);
#6936=ORIENTED_EDGE('',*,*,#4981,.F.);
#6937=ORIENTED_EDGE('',*,*,#4984,.F.);
#6938=ORIENTED_EDGE('',*,*,#4985,.F.);
#6939=ORIENTED_EDGE('',*,*,#4984,.T.);
#6940=ORIENTED_EDGE('',*,*,#4980,.F.);
#6941=ORIENTED_EDGE('',*,*,#4983,.T.);
#6942=ORIENTED_EDGE('',*,*,#4986,.T.);
#6943=ORIENTED_EDGE('',*,*,#4978,.T.);
#6944=ORIENTED_EDGE('',*,*,#4985,.T.);
#6945=ORIENTED_EDGE('',*,*,#4986,.F.);
#6946=ORIENTED_EDGE('',*,*,#4982,.T.);
#6947=ORIENTED_EDGE('',*,*,#4987,.F.);
#6948=ORIENTED_EDGE('',*,*,#4988,.T.);
#6949=ORIENTED_EDGE('',*,*,#4989,.F.);
#6950=ORIENTED_EDGE('',*,*,#4988,.F.);
#6951=ORIENTED_EDGE('',*,*,#4990,.F.);
#6952=ORIENTED_EDGE('',*,*,#4991,.T.);
#6953=ORIENTED_EDGE('',*,*,#4992,.F.);
#6954=ORIENTED_EDGE('',*,*,#4993,.F.);
#6955=ORIENTED_EDGE('',*,*,#4994,.F.);
#6956=ORIENTED_EDGE('',*,*,#4993,.T.);
#6957=ORIENTED_EDGE('',*,*,#4995,.F.);
#6958=ORIENTED_EDGE('',*,*,#4996,.F.);
#6959=ORIENTED_EDGE('',*,*,#4987,.T.);
#6960=ORIENTED_EDGE('',*,*,#4997,.F.);
#6961=ORIENTED_EDGE('',*,*,#4996,.T.);
#6962=ORIENTED_EDGE('',*,*,#4998,.F.);
#6963=ORIENTED_EDGE('',*,*,#4999,.F.);
#6964=ORIENTED_EDGE('',*,*,#5000,.F.);
#6965=ORIENTED_EDGE('',*,*,#4999,.T.);
#6966=ORIENTED_EDGE('',*,*,#5001,.F.);
#6967=ORIENTED_EDGE('',*,*,#4991,.F.);
#6968=ORIENTED_EDGE('',*,*,#4989,.T.);
#6969=ORIENTED_EDGE('',*,*,#5001,.T.);
#6970=ORIENTED_EDGE('',*,*,#4998,.T.);
#6971=ORIENTED_EDGE('',*,*,#4995,.T.);
#6972=ORIENTED_EDGE('',*,*,#4992,.T.);
#6973=ORIENTED_EDGE('',*,*,#5000,.T.);
#6974=ORIENTED_EDGE('',*,*,#4990,.T.);
#6975=ORIENTED_EDGE('',*,*,#4994,.T.);
#6976=ORIENTED_EDGE('',*,*,#4997,.T.);
#6977=ORIENTED_EDGE('',*,*,#5002,.F.);
#6978=ORIENTED_EDGE('',*,*,#5003,.T.);
#6979=ORIENTED_EDGE('',*,*,#5004,.F.);
#6980=ORIENTED_EDGE('',*,*,#5003,.F.);
#6981=ORIENTED_EDGE('',*,*,#5005,.F.);
#6982=ORIENTED_EDGE('',*,*,#5006,.T.);
#6983=ORIENTED_EDGE('',*,*,#5007,.F.);
#6984=ORIENTED_EDGE('',*,*,#5008,.F.);
#6985=ORIENTED_EDGE('',*,*,#5009,.F.);
#6986=ORIENTED_EDGE('',*,*,#5008,.T.);
#6987=ORIENTED_EDGE('',*,*,#5010,.F.);
#6988=ORIENTED_EDGE('',*,*,#5011,.F.);
#6989=ORIENTED_EDGE('',*,*,#5002,.T.);
#6990=ORIENTED_EDGE('',*,*,#5012,.F.);
#6991=ORIENTED_EDGE('',*,*,#5011,.T.);
#6992=ORIENTED_EDGE('',*,*,#5013,.F.);
#6993=ORIENTED_EDGE('',*,*,#5014,.F.);
#6994=ORIENTED_EDGE('',*,*,#5015,.F.);
#6995=ORIENTED_EDGE('',*,*,#5014,.T.);
#6996=ORIENTED_EDGE('',*,*,#5016,.F.);
#6997=ORIENTED_EDGE('',*,*,#5006,.F.);
#6998=ORIENTED_EDGE('',*,*,#5004,.T.);
#6999=ORIENTED_EDGE('',*,*,#5016,.T.);
#7000=ORIENTED_EDGE('',*,*,#5013,.T.);
#7001=ORIENTED_EDGE('',*,*,#5010,.T.);
#7002=ORIENTED_EDGE('',*,*,#5007,.T.);
#7003=ORIENTED_EDGE('',*,*,#5015,.T.);
#7004=ORIENTED_EDGE('',*,*,#5005,.T.);
#7005=ORIENTED_EDGE('',*,*,#5009,.T.);
#7006=ORIENTED_EDGE('',*,*,#5012,.T.);
#7007=ORIENTED_EDGE('',*,*,#5017,.F.);
#7008=ORIENTED_EDGE('',*,*,#5018,.F.);
#7009=ORIENTED_EDGE('',*,*,#5019,.F.);
#7010=ORIENTED_EDGE('',*,*,#5020,.F.);
#7011=ORIENTED_EDGE('',*,*,#5021,.F.);
#7012=ORIENTED_EDGE('',*,*,#5022,.F.);
#7013=ORIENTED_EDGE('',*,*,#5023,.F.);
#7014=ORIENTED_EDGE('',*,*,#5024,.F.);
#7015=ORIENTED_EDGE('',*,*,#5022,.T.);
#7016=ORIENTED_EDGE('',*,*,#5025,.F.);
#7017=ORIENTED_EDGE('',*,*,#5020,.T.);
#7018=ORIENTED_EDGE('',*,*,#5026,.F.);
#7019=ORIENTED_EDGE('',*,*,#5023,.T.);
#7020=ORIENTED_EDGE('',*,*,#5026,.T.);
#7021=ORIENTED_EDGE('',*,*,#5019,.T.);
#7022=ORIENTED_EDGE('',*,*,#5027,.F.);
#7023=ORIENTED_EDGE('',*,*,#5021,.T.);
#7024=ORIENTED_EDGE('',*,*,#5028,.F.);
#7025=ORIENTED_EDGE('',*,*,#5017,.T.);
#7026=ORIENTED_EDGE('',*,*,#5025,.T.);
#7027=ORIENTED_EDGE('',*,*,#5024,.T.);
#7028=ORIENTED_EDGE('',*,*,#5027,.T.);
#7029=ORIENTED_EDGE('',*,*,#5018,.T.);
#7030=ORIENTED_EDGE('',*,*,#5028,.T.);
#7031=ORIENTED_EDGE('',*,*,#5029,.F.);
#7032=ORIENTED_EDGE('',*,*,#5030,.F.);
#7033=ORIENTED_EDGE('',*,*,#5031,.F.);
#7034=ORIENTED_EDGE('',*,*,#5032,.F.);
#7035=ORIENTED_EDGE('',*,*,#5033,.F.);
#7036=ORIENTED_EDGE('',*,*,#5034,.F.);
#7037=ORIENTED_EDGE('',*,*,#5035,.F.);
#7038=ORIENTED_EDGE('',*,*,#5036,.F.);
#7039=ORIENTED_EDGE('',*,*,#5034,.T.);
#7040=ORIENTED_EDGE('',*,*,#5037,.F.);
#7041=ORIENTED_EDGE('',*,*,#5032,.T.);
#7042=ORIENTED_EDGE('',*,*,#5038,.F.);
#7043=ORIENTED_EDGE('',*,*,#5035,.T.);
#7044=ORIENTED_EDGE('',*,*,#5038,.T.);
#7045=ORIENTED_EDGE('',*,*,#5031,.T.);
#7046=ORIENTED_EDGE('',*,*,#5039,.F.);
#7047=ORIENTED_EDGE('',*,*,#5033,.T.);
#7048=ORIENTED_EDGE('',*,*,#5040,.F.);
#7049=ORIENTED_EDGE('',*,*,#5029,.T.);
#7050=ORIENTED_EDGE('',*,*,#5037,.T.);
#7051=ORIENTED_EDGE('',*,*,#5036,.T.);
#7052=ORIENTED_EDGE('',*,*,#5039,.T.);
#7053=ORIENTED_EDGE('',*,*,#5030,.T.);
#7054=ORIENTED_EDGE('',*,*,#5040,.T.);
#7055=ORIENTED_EDGE('',*,*,#5041,.F.);
#7056=ORIENTED_EDGE('',*,*,#5042,.T.);
#7057=ORIENTED_EDGE('',*,*,#5043,.F.);
#7058=ORIENTED_EDGE('',*,*,#5044,.F.);
#7059=ORIENTED_EDGE('',*,*,#5045,.F.);
#7060=ORIENTED_EDGE('',*,*,#5046,.F.);
#7061=ORIENTED_EDGE('',*,*,#5047,.F.);
#7062=ORIENTED_EDGE('',*,*,#5048,.F.);
#7063=ORIENTED_EDGE('',*,*,#5049,.F.);
#7064=ORIENTED_EDGE('',*,*,#5050,.F.);
#7065=ORIENTED_EDGE('',*,*,#5051,.F.);
#7066=ORIENTED_EDGE('',*,*,#5042,.F.);
#7067=ORIENTED_EDGE('',*,*,#5046,.T.);
#7068=ORIENTED_EDGE('',*,*,#5052,.T.);
#7069=ORIENTED_EDGE('',*,*,#5053,.F.);
#7070=ORIENTED_EDGE('',*,*,#5054,.T.);
#7071=ORIENTED_EDGE('',*,*,#5045,.T.);
#7072=ORIENTED_EDGE('',*,*,#5055,.F.);
#7073=ORIENTED_EDGE('',*,*,#5056,.F.);
#7074=ORIENTED_EDGE('',*,*,#5052,.F.);
#7075=ORIENTED_EDGE('',*,*,#5043,.T.);
#7076=ORIENTED_EDGE('',*,*,#5051,.T.);
#7077=ORIENTED_EDGE('',*,*,#5057,.T.);
#7078=ORIENTED_EDGE('',*,*,#5058,.T.);
#7079=ORIENTED_EDGE('',*,*,#5059,.F.);
#7080=ORIENTED_EDGE('',*,*,#5060,.F.);
#7081=ORIENTED_EDGE('',*,*,#5061,.F.);
#7082=ORIENTED_EDGE('',*,*,#5062,.T.);
#7083=ORIENTED_EDGE('',*,*,#5063,.F.);
#7084=ORIENTED_EDGE('',*,*,#5062,.F.);
#7085=ORIENTED_EDGE('',*,*,#5064,.F.);
#7086=ORIENTED_EDGE('',*,*,#5065,.F.);
#7087=ORIENTED_EDGE('',*,*,#5066,.F.);
#7088=ORIENTED_EDGE('',*,*,#5067,.T.);
#7089=ORIENTED_EDGE('',*,*,#5064,.T.);
#7090=ORIENTED_EDGE('',*,*,#5068,.T.);
#7091=ORIENTED_EDGE('',*,*,#5058,.F.);
#7092=ORIENTED_EDGE('',*,*,#5069,.T.);
#7093=ORIENTED_EDGE('',*,*,#5070,.T.);
#7094=ORIENTED_EDGE('',*,*,#5071,.F.);
#7095=ORIENTED_EDGE('',*,*,#5072,.F.);
#7096=ORIENTED_EDGE('',*,*,#5073,.F.);
#7097=ORIENTED_EDGE('',*,*,#5059,.T.);
#7098=ORIENTED_EDGE('',*,*,#5068,.F.);
#7099=ORIENTED_EDGE('',*,*,#5067,.F.);
#7100=ORIENTED_EDGE('',*,*,#5061,.T.);
#7101=ORIENTED_EDGE('',*,*,#5066,.T.);
#7102=ORIENTED_EDGE('',*,*,#5074,.T.);
#7103=ORIENTED_EDGE('',*,*,#5075,.F.);
#7104=ORIENTED_EDGE('',*,*,#5070,.F.);
#7105=ORIENTED_EDGE('',*,*,#5076,.T.);
#7106=ORIENTED_EDGE('',*,*,#5077,.T.);
#7107=ORIENTED_EDGE('',*,*,#5071,.T.);
#7108=ORIENTED_EDGE('',*,*,#5075,.T.);
#7109=ORIENTED_EDGE('',*,*,#5050,.T.);
#7110=ORIENTED_EDGE('',*,*,#5078,.T.);
#7111=ORIENTED_EDGE('',*,*,#5076,.F.);
#7112=ORIENTED_EDGE('',*,*,#5074,.F.);
#7113=ORIENTED_EDGE('',*,*,#5065,.T.);
#7114=ORIENTED_EDGE('',*,*,#5069,.F.);
#7115=ORIENTED_EDGE('',*,*,#5057,.F.);
#7116=ORIENTED_EDGE('',*,*,#5063,.T.);
#7117=ORIENTED_EDGE('',*,*,#5041,.T.);
#7118=ORIENTED_EDGE('',*,*,#5079,.F.);
#7119=ORIENTED_EDGE('',*,*,#5072,.T.);
#7120=ORIENTED_EDGE('',*,*,#5077,.F.);
#7121=ORIENTED_EDGE('',*,*,#5078,.F.);
#7122=ORIENTED_EDGE('',*,*,#5049,.T.);
#7123=ORIENTED_EDGE('',*,*,#5047,.T.);
#7124=ORIENTED_EDGE('',*,*,#5054,.F.);
#7125=ORIENTED_EDGE('',*,*,#5080,.F.);
#7126=ORIENTED_EDGE('',*,*,#5081,.F.);
#7127=ORIENTED_EDGE('',*,*,#5048,.T.);
#7128=ORIENTED_EDGE('',*,*,#5081,.T.);
#7129=ORIENTED_EDGE('',*,*,#5082,.T.);
#7130=ORIENTED_EDGE('',*,*,#5055,.T.);
#7131=ORIENTED_EDGE('',*,*,#5044,.T.);
#7132=ORIENTED_EDGE('',*,*,#5060,.T.);
#7133=ORIENTED_EDGE('',*,*,#5073,.T.);
#7134=ORIENTED_EDGE('',*,*,#5079,.T.);
#7135=ORIENTED_EDGE('',*,*,#5056,.T.);
#7136=ORIENTED_EDGE('',*,*,#5082,.F.);
#7137=ORIENTED_EDGE('',*,*,#5080,.T.);
#7138=ORIENTED_EDGE('',*,*,#5053,.T.);
#7139=ORIENTED_EDGE('',*,*,#5083,.F.);
#7140=ORIENTED_EDGE('',*,*,#5084,.T.);
#7141=ORIENTED_EDGE('',*,*,#5085,.F.);
#7142=ORIENTED_EDGE('',*,*,#5084,.F.);
#7143=ORIENTED_EDGE('',*,*,#5086,.F.);
#7144=ORIENTED_EDGE('',*,*,#5087,.T.);
#7145=ORIENTED_EDGE('',*,*,#5088,.F.);
#7146=ORIENTED_EDGE('',*,*,#5089,.F.);
#7147=ORIENTED_EDGE('',*,*,#5090,.F.);
#7148=ORIENTED_EDGE('',*,*,#5089,.T.);
#7149=ORIENTED_EDGE('',*,*,#5091,.F.);
#7150=ORIENTED_EDGE('',*,*,#5092,.F.);
#7151=ORIENTED_EDGE('',*,*,#5083,.T.);
#7152=ORIENTED_EDGE('',*,*,#5093,.F.);
#7153=ORIENTED_EDGE('',*,*,#5092,.T.);
#7154=ORIENTED_EDGE('',*,*,#5094,.F.);
#7155=ORIENTED_EDGE('',*,*,#5095,.F.);
#7156=ORIENTED_EDGE('',*,*,#5096,.F.);
#7157=ORIENTED_EDGE('',*,*,#5095,.T.);
#7158=ORIENTED_EDGE('',*,*,#5097,.F.);
#7159=ORIENTED_EDGE('',*,*,#5087,.F.);
#7160=ORIENTED_EDGE('',*,*,#5085,.T.);
#7161=ORIENTED_EDGE('',*,*,#5097,.T.);
#7162=ORIENTED_EDGE('',*,*,#5094,.T.);
#7163=ORIENTED_EDGE('',*,*,#5091,.T.);
#7164=ORIENTED_EDGE('',*,*,#5088,.T.);
#7165=ORIENTED_EDGE('',*,*,#5096,.T.);
#7166=ORIENTED_EDGE('',*,*,#5086,.T.);
#7167=ORIENTED_EDGE('',*,*,#5090,.T.);
#7168=ORIENTED_EDGE('',*,*,#5093,.T.);
#7169=ORIENTED_EDGE('',*,*,#5098,.F.);
#7170=ORIENTED_EDGE('',*,*,#5099,.T.);
#7171=ORIENTED_EDGE('',*,*,#5100,.F.);
#7172=ORIENTED_EDGE('',*,*,#5099,.F.);
#7173=ORIENTED_EDGE('',*,*,#5101,.F.);
#7174=ORIENTED_EDGE('',*,*,#5102,.T.);
#7175=ORIENTED_EDGE('',*,*,#5103,.F.);
#7176=ORIENTED_EDGE('',*,*,#5104,.F.);
#7177=ORIENTED_EDGE('',*,*,#5105,.F.);
#7178=ORIENTED_EDGE('',*,*,#5104,.T.);
#7179=ORIENTED_EDGE('',*,*,#5106,.F.);
#7180=ORIENTED_EDGE('',*,*,#5107,.F.);
#7181=ORIENTED_EDGE('',*,*,#5098,.T.);
#7182=ORIENTED_EDGE('',*,*,#5108,.F.);
#7183=ORIENTED_EDGE('',*,*,#5107,.T.);
#7184=ORIENTED_EDGE('',*,*,#5109,.F.);
#7185=ORIENTED_EDGE('',*,*,#5110,.F.);
#7186=ORIENTED_EDGE('',*,*,#5111,.F.);
#7187=ORIENTED_EDGE('',*,*,#5110,.T.);
#7188=ORIENTED_EDGE('',*,*,#5112,.F.);
#7189=ORIENTED_EDGE('',*,*,#5102,.F.);
#7190=ORIENTED_EDGE('',*,*,#5100,.T.);
#7191=ORIENTED_EDGE('',*,*,#5112,.T.);
#7192=ORIENTED_EDGE('',*,*,#5109,.T.);
#7193=ORIENTED_EDGE('',*,*,#5106,.T.);
#7194=ORIENTED_EDGE('',*,*,#5103,.T.);
#7195=ORIENTED_EDGE('',*,*,#5111,.T.);
#7196=ORIENTED_EDGE('',*,*,#5101,.T.);
#7197=ORIENTED_EDGE('',*,*,#5105,.T.);
#7198=ORIENTED_EDGE('',*,*,#5108,.T.);
#7199=ORIENTED_EDGE('',*,*,#5113,.F.);
#7200=ORIENTED_EDGE('',*,*,#5114,.F.);
#7201=ORIENTED_EDGE('',*,*,#5115,.F.);
#7202=ORIENTED_EDGE('',*,*,#5116,.F.);
#7203=ORIENTED_EDGE('',*,*,#5114,.T.);
#7204=ORIENTED_EDGE('',*,*,#5117,.T.);
#7205=ORIENTED_EDGE('',*,*,#5118,.T.);
#7206=ORIENTED_EDGE('',*,*,#5119,.T.);
#7207=ORIENTED_EDGE('',*,*,#5113,.T.);
#7208=ORIENTED_EDGE('',*,*,#5120,.F.);
#7209=ORIENTED_EDGE('',*,*,#5121,.F.);
#7210=ORIENTED_EDGE('',*,*,#5117,.F.);
#7211=ORIENTED_EDGE('',*,*,#5115,.T.);
#7212=ORIENTED_EDGE('',*,*,#5119,.F.);
#7213=ORIENTED_EDGE('',*,*,#5122,.F.);
#7214=ORIENTED_EDGE('',*,*,#5123,.F.);
#7215=ORIENTED_EDGE('',*,*,#5122,.T.);
#7216=ORIENTED_EDGE('',*,*,#5118,.F.);
#7217=ORIENTED_EDGE('',*,*,#5121,.T.);
#7218=ORIENTED_EDGE('',*,*,#5124,.T.);
#7219=ORIENTED_EDGE('',*,*,#5116,.T.);
#7220=ORIENTED_EDGE('',*,*,#5123,.T.);
#7221=ORIENTED_EDGE('',*,*,#5124,.F.);
#7222=ORIENTED_EDGE('',*,*,#5120,.T.);
#7223=ORIENTED_EDGE('',*,*,#5125,.F.);
#7224=ORIENTED_EDGE('',*,*,#5126,.T.);
#7225=ORIENTED_EDGE('',*,*,#5127,.F.);
#7226=ORIENTED_EDGE('',*,*,#5126,.F.);
#7227=ORIENTED_EDGE('',*,*,#5128,.F.);
#7228=ORIENTED_EDGE('',*,*,#5129,.T.);
#7229=ORIENTED_EDGE('',*,*,#5130,.F.);
#7230=ORIENTED_EDGE('',*,*,#5131,.F.);
#7231=ORIENTED_EDGE('',*,*,#5132,.F.);
#7232=ORIENTED_EDGE('',*,*,#5131,.T.);
#7233=ORIENTED_EDGE('',*,*,#5133,.F.);
#7234=ORIENTED_EDGE('',*,*,#5134,.F.);
#7235=ORIENTED_EDGE('',*,*,#5125,.T.);
#7236=ORIENTED_EDGE('',*,*,#5135,.F.);
#7237=ORIENTED_EDGE('',*,*,#5134,.T.);
#7238=ORIENTED_EDGE('',*,*,#5136,.F.);
#7239=ORIENTED_EDGE('',*,*,#5137,.F.);
#7240=ORIENTED_EDGE('',*,*,#5138,.F.);
#7241=ORIENTED_EDGE('',*,*,#5137,.T.);
#7242=ORIENTED_EDGE('',*,*,#5139,.F.);
#7243=ORIENTED_EDGE('',*,*,#5129,.F.);
#7244=ORIENTED_EDGE('',*,*,#5127,.T.);
#7245=ORIENTED_EDGE('',*,*,#5139,.T.);
#7246=ORIENTED_EDGE('',*,*,#5136,.T.);
#7247=ORIENTED_EDGE('',*,*,#5133,.T.);
#7248=ORIENTED_EDGE('',*,*,#5130,.T.);
#7249=ORIENTED_EDGE('',*,*,#5138,.T.);
#7250=ORIENTED_EDGE('',*,*,#5128,.T.);
#7251=ORIENTED_EDGE('',*,*,#5132,.T.);
#7252=ORIENTED_EDGE('',*,*,#5135,.T.);
#7253=ORIENTED_EDGE('',*,*,#5140,.F.);
#7254=ORIENTED_EDGE('',*,*,#5141,.T.);
#7255=ORIENTED_EDGE('',*,*,#5142,.F.);
#7256=ORIENTED_EDGE('',*,*,#5141,.F.);
#7257=ORIENTED_EDGE('',*,*,#5143,.F.);
#7258=ORIENTED_EDGE('',*,*,#5144,.T.);
#7259=ORIENTED_EDGE('',*,*,#5145,.F.);
#7260=ORIENTED_EDGE('',*,*,#5146,.F.);
#7261=ORIENTED_EDGE('',*,*,#5147,.F.);
#7262=ORIENTED_EDGE('',*,*,#5146,.T.);
#7263=ORIENTED_EDGE('',*,*,#5148,.F.);
#7264=ORIENTED_EDGE('',*,*,#5149,.F.);
#7265=ORIENTED_EDGE('',*,*,#5140,.T.);
#7266=ORIENTED_EDGE('',*,*,#5150,.F.);
#7267=ORIENTED_EDGE('',*,*,#5149,.T.);
#7268=ORIENTED_EDGE('',*,*,#5151,.F.);
#7269=ORIENTED_EDGE('',*,*,#5152,.F.);
#7270=ORIENTED_EDGE('',*,*,#5153,.F.);
#7271=ORIENTED_EDGE('',*,*,#5152,.T.);
#7272=ORIENTED_EDGE('',*,*,#5154,.F.);
#7273=ORIENTED_EDGE('',*,*,#5144,.F.);
#7274=ORIENTED_EDGE('',*,*,#5142,.T.);
#7275=ORIENTED_EDGE('',*,*,#5154,.T.);
#7276=ORIENTED_EDGE('',*,*,#5151,.T.);
#7277=ORIENTED_EDGE('',*,*,#5148,.T.);
#7278=ORIENTED_EDGE('',*,*,#5145,.T.);
#7279=ORIENTED_EDGE('',*,*,#5153,.T.);
#7280=ORIENTED_EDGE('',*,*,#5143,.T.);
#7281=ORIENTED_EDGE('',*,*,#5147,.T.);
#7282=ORIENTED_EDGE('',*,*,#5150,.T.);
#7283=ORIENTED_EDGE('',*,*,#5155,.F.);
#7284=ORIENTED_EDGE('',*,*,#5156,.F.);
#7285=ORIENTED_EDGE('',*,*,#5157,.F.);
#7286=ORIENTED_EDGE('',*,*,#5158,.F.);
#7287=ORIENTED_EDGE('',*,*,#5159,.F.);
#7288=ORIENTED_EDGE('',*,*,#5160,.F.);
#7289=ORIENTED_EDGE('',*,*,#5161,.F.);
#7290=ORIENTED_EDGE('',*,*,#5162,.F.);
#7291=ORIENTED_EDGE('',*,*,#5160,.T.);
#7292=ORIENTED_EDGE('',*,*,#5163,.F.);
#7293=ORIENTED_EDGE('',*,*,#5158,.T.);
#7294=ORIENTED_EDGE('',*,*,#5164,.F.);
#7295=ORIENTED_EDGE('',*,*,#5161,.T.);
#7296=ORIENTED_EDGE('',*,*,#5164,.T.);
#7297=ORIENTED_EDGE('',*,*,#5157,.T.);
#7298=ORIENTED_EDGE('',*,*,#5165,.F.);
#7299=ORIENTED_EDGE('',*,*,#5159,.T.);
#7300=ORIENTED_EDGE('',*,*,#5166,.F.);
#7301=ORIENTED_EDGE('',*,*,#5155,.T.);
#7302=ORIENTED_EDGE('',*,*,#5163,.T.);
#7303=ORIENTED_EDGE('',*,*,#5162,.T.);
#7304=ORIENTED_EDGE('',*,*,#5165,.T.);
#7305=ORIENTED_EDGE('',*,*,#5156,.T.);
#7306=ORIENTED_EDGE('',*,*,#5166,.T.);
#7307=ORIENTED_EDGE('',*,*,#5167,.F.);
#7308=ORIENTED_EDGE('',*,*,#5168,.F.);
#7309=ORIENTED_EDGE('',*,*,#5169,.F.);
#7310=ORIENTED_EDGE('',*,*,#5170,.F.);
#7311=ORIENTED_EDGE('',*,*,#5171,.F.);
#7312=ORIENTED_EDGE('',*,*,#5172,.F.);
#7313=ORIENTED_EDGE('',*,*,#5173,.F.);
#7314=ORIENTED_EDGE('',*,*,#5174,.F.);
#7315=ORIENTED_EDGE('',*,*,#5172,.T.);
#7316=ORIENTED_EDGE('',*,*,#5175,.F.);
#7317=ORIENTED_EDGE('',*,*,#5170,.T.);
#7318=ORIENTED_EDGE('',*,*,#5176,.F.);
#7319=ORIENTED_EDGE('',*,*,#5173,.T.);
#7320=ORIENTED_EDGE('',*,*,#5176,.T.);
#7321=ORIENTED_EDGE('',*,*,#5169,.T.);
#7322=ORIENTED_EDGE('',*,*,#5177,.F.);
#7323=ORIENTED_EDGE('',*,*,#5171,.T.);
#7324=ORIENTED_EDGE('',*,*,#5178,.F.);
#7325=ORIENTED_EDGE('',*,*,#5167,.T.);
#7326=ORIENTED_EDGE('',*,*,#5175,.T.);
#7327=ORIENTED_EDGE('',*,*,#5174,.T.);
#7328=ORIENTED_EDGE('',*,*,#5177,.T.);
#7329=ORIENTED_EDGE('',*,*,#5168,.T.);
#7330=ORIENTED_EDGE('',*,*,#5178,.T.);
#7331=ORIENTED_EDGE('',*,*,#5179,.T.);
#7332=ORIENTED_EDGE('',*,*,#5180,.T.);
#7333=ORIENTED_EDGE('',*,*,#5181,.F.);
#7334=ORIENTED_EDGE('',*,*,#5182,.F.);
#7335=ORIENTED_EDGE('',*,*,#5183,.T.);
#7336=ORIENTED_EDGE('',*,*,#5182,.T.);
#7337=ORIENTED_EDGE('',*,*,#5184,.F.);
#7338=ORIENTED_EDGE('',*,*,#5185,.F.);
#7339=ORIENTED_EDGE('',*,*,#5186,.T.);
#7340=ORIENTED_EDGE('',*,*,#5185,.T.);
#7341=ORIENTED_EDGE('',*,*,#5187,.F.);
#7342=ORIENTED_EDGE('',*,*,#5188,.F.);
#7343=ORIENTED_EDGE('',*,*,#5189,.T.);
#7344=ORIENTED_EDGE('',*,*,#5188,.T.);
#7345=ORIENTED_EDGE('',*,*,#5190,.F.);
#7346=ORIENTED_EDGE('',*,*,#5180,.F.);
#7347=ORIENTED_EDGE('',*,*,#5190,.T.);
#7348=ORIENTED_EDGE('',*,*,#5187,.T.);
#7349=ORIENTED_EDGE('',*,*,#5184,.T.);
#7350=ORIENTED_EDGE('',*,*,#5181,.T.);
#7351=ORIENTED_EDGE('',*,*,#5189,.F.);
#7352=ORIENTED_EDGE('',*,*,#5179,.F.);
#7353=ORIENTED_EDGE('',*,*,#5183,.F.);
#7354=ORIENTED_EDGE('',*,*,#5186,.F.);
#7355=ORIENTED_EDGE('',*,*,#5191,.T.);
#7356=ORIENTED_EDGE('',*,*,#5192,.T.);
#7357=ORIENTED_EDGE('',*,*,#5193,.F.);
#7358=ORIENTED_EDGE('',*,*,#5194,.F.);
#7359=ORIENTED_EDGE('',*,*,#5195,.T.);
#7360=ORIENTED_EDGE('',*,*,#5194,.T.);
#7361=ORIENTED_EDGE('',*,*,#5196,.F.);
#7362=ORIENTED_EDGE('',*,*,#5197,.F.);
#7363=ORIENTED_EDGE('',*,*,#5198,.T.);
#7364=ORIENTED_EDGE('',*,*,#5197,.T.);
#7365=ORIENTED_EDGE('',*,*,#5199,.F.);
#7366=ORIENTED_EDGE('',*,*,#5200,.F.);
#7367=ORIENTED_EDGE('',*,*,#5201,.T.);
#7368=ORIENTED_EDGE('',*,*,#5200,.T.);
#7369=ORIENTED_EDGE('',*,*,#5202,.F.);
#7370=ORIENTED_EDGE('',*,*,#5192,.F.);
#7371=ORIENTED_EDGE('',*,*,#5202,.T.);
#7372=ORIENTED_EDGE('',*,*,#5199,.T.);
#7373=ORIENTED_EDGE('',*,*,#5196,.T.);
#7374=ORIENTED_EDGE('',*,*,#5193,.T.);
#7375=ORIENTED_EDGE('',*,*,#5201,.F.);
#7376=ORIENTED_EDGE('',*,*,#5191,.F.);
#7377=ORIENTED_EDGE('',*,*,#5195,.F.);
#7378=ORIENTED_EDGE('',*,*,#5198,.F.);
#7379=ORIENTED_EDGE('',*,*,#5203,.T.);
#7380=ORIENTED_EDGE('',*,*,#5204,.T.);
#7381=ORIENTED_EDGE('',*,*,#5205,.T.);
#7382=ORIENTED_EDGE('',*,*,#5206,.F.);
#7383=ORIENTED_EDGE('',*,*,#5207,.T.);
#7384=ORIENTED_EDGE('',*,*,#5208,.T.);
#7385=ORIENTED_EDGE('',*,*,#5209,.T.);
#7386=ORIENTED_EDGE('',*,*,#5204,.F.);
#7387=ORIENTED_EDGE('',*,*,#5210,.T.);
#7388=ORIENTED_EDGE('',*,*,#5211,.T.);
#7389=ORIENTED_EDGE('',*,*,#5212,.T.);
#7390=ORIENTED_EDGE('',*,*,#5208,.F.);
#7391=ORIENTED_EDGE('',*,*,#5213,.T.);
#7392=ORIENTED_EDGE('',*,*,#5214,.T.);
#7393=ORIENTED_EDGE('',*,*,#5215,.T.);
#7394=ORIENTED_EDGE('',*,*,#5211,.F.);
#7395=ORIENTED_EDGE('',*,*,#5216,.T.);
#7396=ORIENTED_EDGE('',*,*,#5217,.T.);
#7397=ORIENTED_EDGE('',*,*,#5218,.T.);
#7398=ORIENTED_EDGE('',*,*,#5214,.F.);
#7399=ORIENTED_EDGE('',*,*,#5219,.T.);
#7400=ORIENTED_EDGE('',*,*,#5206,.T.);
#7401=ORIENTED_EDGE('',*,*,#5220,.T.);
#7402=ORIENTED_EDGE('',*,*,#5217,.F.);
#7403=ORIENTED_EDGE('',*,*,#5219,.F.);
#7404=ORIENTED_EDGE('',*,*,#5216,.F.);
#7405=ORIENTED_EDGE('',*,*,#5213,.F.);
#7406=ORIENTED_EDGE('',*,*,#5210,.F.);
#7407=ORIENTED_EDGE('',*,*,#5207,.F.);
#7408=ORIENTED_EDGE('',*,*,#5203,.F.);
#7409=ORIENTED_EDGE('',*,*,#5220,.F.);
#7410=ORIENTED_EDGE('',*,*,#5205,.F.);
#7411=ORIENTED_EDGE('',*,*,#5209,.F.);
#7412=ORIENTED_EDGE('',*,*,#5212,.F.);
#7413=ORIENTED_EDGE('',*,*,#5215,.F.);
#7414=ORIENTED_EDGE('',*,*,#5218,.F.);
#7415=ORIENTED_EDGE('',*,*,#5221,.F.);
#7416=ORIENTED_EDGE('',*,*,#5222,.F.);
#7417=ORIENTED_EDGE('',*,*,#5223,.F.);
#7418=ORIENTED_EDGE('',*,*,#5224,.T.);
#7419=ORIENTED_EDGE('',*,*,#5222,.T.);
#7420=ORIENTED_EDGE('',*,*,#5224,.F.);
#7421=ORIENTED_EDGE('',*,*,#5225,.F.);
#7422=ORIENTED_EDGE('',*,*,#5226,.T.);
#7423=ORIENTED_EDGE('',*,*,#5223,.T.);
#7424=ORIENTED_EDGE('',*,*,#5226,.F.);
#7425=ORIENTED_EDGE('',*,*,#5227,.F.);
#7426=ORIENTED_EDGE('',*,*,#5228,.T.);
#7427=ORIENTED_EDGE('',*,*,#5225,.T.);
#7428=ORIENTED_EDGE('',*,*,#5228,.F.);
#7429=ORIENTED_EDGE('',*,*,#5227,.T.);
#7430=ORIENTED_EDGE('',*,*,#5229,.F.);
#7431=ORIENTED_EDGE('',*,*,#5230,.F.);
#7432=ORIENTED_EDGE('',*,*,#5231,.T.);
#7433=ORIENTED_EDGE('',*,*,#5229,.T.);
#7434=ORIENTED_EDGE('',*,*,#5231,.F.);
#7435=ORIENTED_EDGE('',*,*,#5221,.T.);
#7436=ORIENTED_EDGE('',*,*,#5232,.T.);
#7437=ORIENTED_EDGE('',*,*,#5230,.T.);
#7438=ORIENTED_EDGE('',*,*,#5232,.F.);
#7439=ORIENTED_EDGE('',*,*,#5233,.T.);
#7440=ORIENTED_EDGE('',*,*,#5234,.T.);
#7441=ORIENTED_EDGE('',*,*,#5235,.T.);
#7442=ORIENTED_EDGE('',*,*,#5236,.F.);
#7443=ORIENTED_EDGE('',*,*,#5237,.T.);
#7444=ORIENTED_EDGE('',*,*,#5238,.T.);
#7445=ORIENTED_EDGE('',*,*,#5239,.T.);
#7446=ORIENTED_EDGE('',*,*,#5234,.F.);
#7447=ORIENTED_EDGE('',*,*,#5240,.T.);
#7448=ORIENTED_EDGE('',*,*,#5241,.T.);
#7449=ORIENTED_EDGE('',*,*,#5242,.T.);
#7450=ORIENTED_EDGE('',*,*,#5238,.F.);
#7451=ORIENTED_EDGE('',*,*,#5243,.T.);
#7452=ORIENTED_EDGE('',*,*,#5244,.T.);
#7453=ORIENTED_EDGE('',*,*,#5245,.T.);
#7454=ORIENTED_EDGE('',*,*,#5241,.F.);
#7455=ORIENTED_EDGE('',*,*,#5246,.T.);
#7456=ORIENTED_EDGE('',*,*,#5247,.T.);
#7457=ORIENTED_EDGE('',*,*,#5248,.T.);
#7458=ORIENTED_EDGE('',*,*,#5244,.F.);
#7459=ORIENTED_EDGE('',*,*,#5249,.T.);
#7460=ORIENTED_EDGE('',*,*,#5236,.T.);
#7461=ORIENTED_EDGE('',*,*,#5250,.T.);
#7462=ORIENTED_EDGE('',*,*,#5247,.F.);
#7463=ORIENTED_EDGE('',*,*,#5249,.F.);
#7464=ORIENTED_EDGE('',*,*,#5246,.F.);
#7465=ORIENTED_EDGE('',*,*,#5243,.F.);
#7466=ORIENTED_EDGE('',*,*,#5240,.F.);
#7467=ORIENTED_EDGE('',*,*,#5237,.F.);
#7468=ORIENTED_EDGE('',*,*,#5233,.F.);
#7469=ORIENTED_EDGE('',*,*,#5250,.F.);
#7470=ORIENTED_EDGE('',*,*,#5235,.F.);
#7471=ORIENTED_EDGE('',*,*,#5239,.F.);
#7472=ORIENTED_EDGE('',*,*,#5242,.F.);
#7473=ORIENTED_EDGE('',*,*,#5245,.F.);
#7474=ORIENTED_EDGE('',*,*,#5248,.F.);
#7475=ORIENTED_EDGE('',*,*,#5251,.T.);
#7476=ORIENTED_EDGE('',*,*,#5252,.F.);
#7477=ORIENTED_EDGE('',*,*,#5251,.F.);
#7478=ORIENTED_EDGE('',*,*,#5253,.T.);
#7479=ORIENTED_EDGE('',*,*,#5254,.T.);
#7480=ORIENTED_EDGE('',*,*,#5253,.F.);
#7481=ORIENTED_EDGE('',*,*,#5254,.F.);
#7482=ORIENTED_EDGE('',*,*,#5255,.F.);
#7483=ORIENTED_EDGE('',*,*,#5256,.F.);
#7484=ORIENTED_EDGE('',*,*,#5257,.T.);
#7485=ORIENTED_EDGE('',*,*,#5255,.T.);
#7486=ORIENTED_EDGE('',*,*,#5257,.F.);
#7487=ORIENTED_EDGE('',*,*,#5258,.F.);
#7488=ORIENTED_EDGE('',*,*,#5259,.T.);
#7489=ORIENTED_EDGE('',*,*,#5256,.T.);
#7490=ORIENTED_EDGE('',*,*,#5259,.F.);
#7491=ORIENTED_EDGE('',*,*,#5260,.F.);
#7492=ORIENTED_EDGE('',*,*,#5261,.T.);
#7493=ORIENTED_EDGE('',*,*,#5258,.T.);
#7494=ORIENTED_EDGE('',*,*,#5261,.F.);
#7495=ORIENTED_EDGE('',*,*,#5260,.T.);
#7496=ORIENTED_EDGE('',*,*,#5262,.F.);
#7497=ORIENTED_EDGE('',*,*,#5263,.F.);
#7498=ORIENTED_EDGE('',*,*,#5264,.T.);
#7499=ORIENTED_EDGE('',*,*,#5262,.T.);
#7500=ORIENTED_EDGE('',*,*,#5264,.F.);
#7501=ORIENTED_EDGE('',*,*,#5252,.T.);
#7502=ORIENTED_EDGE('',*,*,#5265,.T.);
#7503=ORIENTED_EDGE('',*,*,#5263,.T.);
#7504=ORIENTED_EDGE('',*,*,#5265,.F.);
#7505=ORIENTED_EDGE('',*,*,#5266,.F.);
#7506=ORIENTED_EDGE('',*,*,#5267,.T.);
#7507=ORIENTED_EDGE('',*,*,#5268,.T.);
#7508=ORIENTED_EDGE('',*,*,#5267,.F.);
#7509=ORIENTED_EDGE('',*,*,#5269,.F.);
#7510=ORIENTED_EDGE('',*,*,#5270,.T.);
#7511=ORIENTED_EDGE('',*,*,#5271,.T.);
#7512=ORIENTED_EDGE('',*,*,#5270,.F.);
#7513=ORIENTED_EDGE('',*,*,#5269,.T.);
#7514=ORIENTED_EDGE('',*,*,#5266,.T.);
#7515=ORIENTED_EDGE('',*,*,#5271,.F.);
#7516=ORIENTED_EDGE('',*,*,#5268,.F.);
#7517=ORIENTED_EDGE('',*,*,#5272,.F.);
#7518=ORIENTED_EDGE('',*,*,#5273,.F.);
#7519=ORIENTED_EDGE('',*,*,#5274,.T.);
#7520=ORIENTED_EDGE('',*,*,#5275,.F.);
#7521=ORIENTED_EDGE('',*,*,#5274,.F.);
#7522=ORIENTED_EDGE('',*,*,#5276,.F.);
#7523=ORIENTED_EDGE('',*,*,#5277,.F.);
#7524=ORIENTED_EDGE('',*,*,#5278,.F.);
#7525=ORIENTED_EDGE('',*,*,#5279,.F.);
#7526=ORIENTED_EDGE('',*,*,#5280,.F.);
#7527=ORIENTED_EDGE('',*,*,#5281,.T.);
#7528=ORIENTED_EDGE('',*,*,#5282,.F.);
#7529=ORIENTED_EDGE('',*,*,#5283,.F.);
#7530=ORIENTED_EDGE('',*,*,#5284,.F.);
#7531=ORIENTED_EDGE('',*,*,#5285,.F.);
#7532=ORIENTED_EDGE('',*,*,#5286,.F.);
#7533=ORIENTED_EDGE('',*,*,#5287,.F.);
#7534=ORIENTED_EDGE('',*,*,#5281,.F.);
#7535=ORIENTED_EDGE('',*,*,#5277,.T.);
#7536=ORIENTED_EDGE('',*,*,#5288,.T.);
#7537=ORIENTED_EDGE('',*,*,#5286,.T.);
#7538=ORIENTED_EDGE('',*,*,#5289,.F.);
#7539=ORIENTED_EDGE('',*,*,#5276,.T.);
#7540=ORIENTED_EDGE('',*,*,#5290,.T.);
#7541=ORIENTED_EDGE('',*,*,#5287,.T.);
#7542=ORIENTED_EDGE('',*,*,#5288,.F.);
#7543=ORIENTED_EDGE('',*,*,#5273,.T.);
#7544=ORIENTED_EDGE('',*,*,#5291,.T.);
#7545=ORIENTED_EDGE('',*,*,#5282,.T.);
#7546=ORIENTED_EDGE('',*,*,#5290,.F.);
#7547=ORIENTED_EDGE('',*,*,#5292,.F.);
#7548=ORIENTED_EDGE('',*,*,#5293,.T.);
#7549=ORIENTED_EDGE('',*,*,#5294,.T.);
#7550=ORIENTED_EDGE('',*,*,#5293,.F.);
#7551=ORIENTED_EDGE('',*,*,#5272,.T.);
#7552=ORIENTED_EDGE('',*,*,#5295,.T.);
#7553=ORIENTED_EDGE('',*,*,#5283,.T.);
#7554=ORIENTED_EDGE('',*,*,#5291,.F.);
#7555=ORIENTED_EDGE('',*,*,#5278,.T.);
#7556=ORIENTED_EDGE('',*,*,#5289,.T.);
#7557=ORIENTED_EDGE('',*,*,#5285,.T.);
#7558=ORIENTED_EDGE('',*,*,#5296,.F.);
#7559=ORIENTED_EDGE('',*,*,#5279,.T.);
#7560=ORIENTED_EDGE('',*,*,#5296,.T.);
#7561=ORIENTED_EDGE('',*,*,#5284,.T.);
#7562=ORIENTED_EDGE('',*,*,#5295,.F.);
#7563=ORIENTED_EDGE('',*,*,#5280,.T.);
#7564=ORIENTED_EDGE('',*,*,#5292,.T.);
#7565=ORIENTED_EDGE('',*,*,#5275,.T.);
#7566=ORIENTED_EDGE('',*,*,#5294,.F.);
#7567=ORIENTED_EDGE('',*,*,#5297,.T.);
#7568=ORIENTED_EDGE('',*,*,#5298,.T.);
#7569=ORIENTED_EDGE('',*,*,#5299,.F.);
#7570=ORIENTED_EDGE('',*,*,#5300,.T.);
#7571=ORIENTED_EDGE('',*,*,#5301,.T.);
#7572=ORIENTED_EDGE('',*,*,#5302,.T.);
#7573=ORIENTED_EDGE('',*,*,#5297,.F.);
#7574=ORIENTED_EDGE('',*,*,#5303,.T.);
#7575=ORIENTED_EDGE('',*,*,#5304,.T.);
#7576=ORIENTED_EDGE('',*,*,#5305,.T.);
#7577=ORIENTED_EDGE('',*,*,#5301,.F.);
#7578=ORIENTED_EDGE('',*,*,#5306,.T.);
#7579=ORIENTED_EDGE('',*,*,#5307,.F.);
#7580=ORIENTED_EDGE('',*,*,#5308,.T.);
#7581=ORIENTED_EDGE('',*,*,#5309,.F.);
#7582=ORIENTED_EDGE('',*,*,#5310,.T.);
#7583=ORIENTED_EDGE('',*,*,#5311,.T.);
#7584=ORIENTED_EDGE('',*,*,#5312,.T.);
#7585=ORIENTED_EDGE('',*,*,#5313,.F.);
#7586=ORIENTED_EDGE('',*,*,#5314,.F.);
#7587=ORIENTED_EDGE('',*,*,#5315,.T.);
#7588=ORIENTED_EDGE('',*,*,#5316,.T.);
#7589=ORIENTED_EDGE('',*,*,#5311,.F.);
#7590=ORIENTED_EDGE('',*,*,#5317,.F.);
#7591=ORIENTED_EDGE('',*,*,#5318,.T.);
#7592=ORIENTED_EDGE('',*,*,#5319,.T.);
#7593=ORIENTED_EDGE('',*,*,#5315,.F.);
#7594=ORIENTED_EDGE('',*,*,#5320,.F.);
#7595=ORIENTED_EDGE('',*,*,#5321,.F.);
#7596=ORIENTED_EDGE('',*,*,#5322,.F.);
#7597=ORIENTED_EDGE('',*,*,#5323,.F.);
#7598=ORIENTED_EDGE('',*,*,#5324,.T.);
#7599=ORIENTED_EDGE('',*,*,#5321,.T.);
#7600=ORIENTED_EDGE('',*,*,#5325,.T.);
#7601=ORIENTED_EDGE('',*,*,#5318,.F.);
#7602=ORIENTED_EDGE('',*,*,#5326,.F.);
#7603=ORIENTED_EDGE('',*,*,#5327,.F.);
#7604=ORIENTED_EDGE('',*,*,#5312,.F.);
#7605=ORIENTED_EDGE('',*,*,#5316,.F.);
#7606=ORIENTED_EDGE('',*,*,#5319,.F.);
#7607=ORIENTED_EDGE('',*,*,#5325,.F.);
#7608=ORIENTED_EDGE('',*,*,#5324,.F.);
#7609=ORIENTED_EDGE('',*,*,#5328,.F.);
#7610=ORIENTED_EDGE('',*,*,#5308,.F.);
#7611=ORIENTED_EDGE('',*,*,#5329,.F.);
#7612=ORIENTED_EDGE('',*,*,#5306,.F.);
#7613=ORIENTED_EDGE('',*,*,#5303,.F.);
#7614=ORIENTED_EDGE('',*,*,#5300,.F.);
#7615=ORIENTED_EDGE('',*,*,#5330,.F.);
#7616=ORIENTED_EDGE('',*,*,#5298,.F.);
#7617=ORIENTED_EDGE('',*,*,#5302,.F.);
#7618=ORIENTED_EDGE('',*,*,#5305,.F.);
#7619=ORIENTED_EDGE('',*,*,#5331,.F.);
#7620=ORIENTED_EDGE('',*,*,#5310,.F.);
#7621=ORIENTED_EDGE('',*,*,#5332,.F.);
#7622=ORIENTED_EDGE('',*,*,#5322,.T.);
#7623=ORIENTED_EDGE('',*,*,#5326,.T.);
#7624=ORIENTED_EDGE('',*,*,#5320,.T.);
#7625=ORIENTED_EDGE('',*,*,#5317,.T.);
#7626=ORIENTED_EDGE('',*,*,#5314,.T.);
#7627=ORIENTED_EDGE('',*,*,#5333,.T.);
#7628=ORIENTED_EDGE('',*,*,#5334,.T.);
#7629=ORIENTED_EDGE('',*,*,#5335,.T.);
#7630=ORIENTED_EDGE('',*,*,#5336,.T.);
#7631=ORIENTED_EDGE('',*,*,#5337,.T.);
#7632=ORIENTED_EDGE('',*,*,#5338,.T.);
#7633=ORIENTED_EDGE('',*,*,#5330,.T.);
#7634=ORIENTED_EDGE('',*,*,#5313,.T.);
#7635=ORIENTED_EDGE('',*,*,#5327,.T.);
#7636=ORIENTED_EDGE('',*,*,#5299,.T.);
#7637=ORIENTED_EDGE('',*,*,#5307,.T.);
#7638=ORIENTED_EDGE('',*,*,#5331,.T.);
#7639=ORIENTED_EDGE('',*,*,#5304,.F.);
#7640=ORIENTED_EDGE('',*,*,#5329,.T.);
#7641=ORIENTED_EDGE('',*,*,#5339,.T.);
#7642=ORIENTED_EDGE('',*,*,#5340,.T.);
#7643=ORIENTED_EDGE('',*,*,#5338,.F.);
#7644=ORIENTED_EDGE('',*,*,#5341,.F.);
#7645=ORIENTED_EDGE('',*,*,#5342,.T.);
#7646=ORIENTED_EDGE('',*,*,#5341,.T.);
#7647=ORIENTED_EDGE('',*,*,#5337,.F.);
#7648=ORIENTED_EDGE('',*,*,#5343,.F.);
#7649=ORIENTED_EDGE('',*,*,#5344,.T.);
#7650=ORIENTED_EDGE('',*,*,#5343,.T.);
#7651=ORIENTED_EDGE('',*,*,#5336,.F.);
#7652=ORIENTED_EDGE('',*,*,#5345,.F.);
#7653=ORIENTED_EDGE('',*,*,#5346,.T.);
#7654=ORIENTED_EDGE('',*,*,#5345,.T.);
#7655=ORIENTED_EDGE('',*,*,#5335,.F.);
#7656=ORIENTED_EDGE('',*,*,#5347,.F.);
#7657=ORIENTED_EDGE('',*,*,#5348,.T.);
#7658=ORIENTED_EDGE('',*,*,#5347,.T.);
#7659=ORIENTED_EDGE('',*,*,#5334,.F.);
#7660=ORIENTED_EDGE('',*,*,#5349,.F.);
#7661=ORIENTED_EDGE('',*,*,#5350,.T.);
#7662=ORIENTED_EDGE('',*,*,#5349,.T.);
#7663=ORIENTED_EDGE('',*,*,#5333,.F.);
#7664=ORIENTED_EDGE('',*,*,#5340,.F.);
#7665=ORIENTED_EDGE('',*,*,#5350,.F.);
#7666=ORIENTED_EDGE('',*,*,#5339,.F.);
#7667=ORIENTED_EDGE('',*,*,#5342,.F.);
#7668=ORIENTED_EDGE('',*,*,#5344,.F.);
#7669=ORIENTED_EDGE('',*,*,#5346,.F.);
#7670=ORIENTED_EDGE('',*,*,#5348,.F.);
#7671=ORIENTED_EDGE('',*,*,#5332,.T.);
#7672=ORIENTED_EDGE('',*,*,#5309,.T.);
#7673=ORIENTED_EDGE('',*,*,#5328,.T.);
#7674=ORIENTED_EDGE('',*,*,#5323,.T.);
#7675=ORIENTED_EDGE('',*,*,#5351,.T.);
#7676=ORIENTED_EDGE('',*,*,#5352,.T.);
#7677=ORIENTED_EDGE('',*,*,#5353,.F.);
#7678=ORIENTED_EDGE('',*,*,#5354,.T.);
#7679=ORIENTED_EDGE('',*,*,#5355,.T.);
#7680=ORIENTED_EDGE('',*,*,#5356,.T.);
#7681=ORIENTED_EDGE('',*,*,#5351,.F.);
#7682=ORIENTED_EDGE('',*,*,#5357,.T.);
#7683=ORIENTED_EDGE('',*,*,#5358,.T.);
#7684=ORIENTED_EDGE('',*,*,#5359,.T.);
#7685=ORIENTED_EDGE('',*,*,#5355,.F.);
#7686=ORIENTED_EDGE('',*,*,#5360,.T.);
#7687=ORIENTED_EDGE('',*,*,#5361,.F.);
#7688=ORIENTED_EDGE('',*,*,#5362,.T.);
#7689=ORIENTED_EDGE('',*,*,#5363,.F.);
#7690=ORIENTED_EDGE('',*,*,#5364,.T.);
#7691=ORIENTED_EDGE('',*,*,#5365,.T.);
#7692=ORIENTED_EDGE('',*,*,#5366,.T.);
#7693=ORIENTED_EDGE('',*,*,#5367,.F.);
#7694=ORIENTED_EDGE('',*,*,#5368,.F.);
#7695=ORIENTED_EDGE('',*,*,#5369,.T.);
#7696=ORIENTED_EDGE('',*,*,#5370,.T.);
#7697=ORIENTED_EDGE('',*,*,#5365,.F.);
#7698=ORIENTED_EDGE('',*,*,#5371,.F.);
#7699=ORIENTED_EDGE('',*,*,#5372,.T.);
#7700=ORIENTED_EDGE('',*,*,#5373,.T.);
#7701=ORIENTED_EDGE('',*,*,#5369,.F.);
#7702=ORIENTED_EDGE('',*,*,#5374,.F.);
#7703=ORIENTED_EDGE('',*,*,#5375,.F.);
#7704=ORIENTED_EDGE('',*,*,#5376,.F.);
#7705=ORIENTED_EDGE('',*,*,#5377,.F.);
#7706=ORIENTED_EDGE('',*,*,#5378,.T.);
#7707=ORIENTED_EDGE('',*,*,#5375,.T.);
#7708=ORIENTED_EDGE('',*,*,#5379,.T.);
#7709=ORIENTED_EDGE('',*,*,#5372,.F.);
#7710=ORIENTED_EDGE('',*,*,#5380,.F.);
#7711=ORIENTED_EDGE('',*,*,#5381,.F.);
#7712=ORIENTED_EDGE('',*,*,#5366,.F.);
#7713=ORIENTED_EDGE('',*,*,#5370,.F.);
#7714=ORIENTED_EDGE('',*,*,#5373,.F.);
#7715=ORIENTED_EDGE('',*,*,#5379,.F.);
#7716=ORIENTED_EDGE('',*,*,#5378,.F.);
#7717=ORIENTED_EDGE('',*,*,#5382,.F.);
#7718=ORIENTED_EDGE('',*,*,#5362,.F.);
#7719=ORIENTED_EDGE('',*,*,#5383,.F.);
#7720=ORIENTED_EDGE('',*,*,#5360,.F.);
#7721=ORIENTED_EDGE('',*,*,#5357,.F.);
#7722=ORIENTED_EDGE('',*,*,#5354,.F.);
#7723=ORIENTED_EDGE('',*,*,#5384,.F.);
#7724=ORIENTED_EDGE('',*,*,#5352,.F.);
#7725=ORIENTED_EDGE('',*,*,#5356,.F.);
#7726=ORIENTED_EDGE('',*,*,#5359,.F.);
#7727=ORIENTED_EDGE('',*,*,#5385,.F.);
#7728=ORIENTED_EDGE('',*,*,#5364,.F.);
#7729=ORIENTED_EDGE('',*,*,#5386,.F.);
#7730=ORIENTED_EDGE('',*,*,#5376,.T.);
#7731=ORIENTED_EDGE('',*,*,#5380,.T.);
#7732=ORIENTED_EDGE('',*,*,#5374,.T.);
#7733=ORIENTED_EDGE('',*,*,#5371,.T.);
#7734=ORIENTED_EDGE('',*,*,#5368,.T.);
#7735=ORIENTED_EDGE('',*,*,#5387,.T.);
#7736=ORIENTED_EDGE('',*,*,#5388,.T.);
#7737=ORIENTED_EDGE('',*,*,#5389,.T.);
#7738=ORIENTED_EDGE('',*,*,#5390,.T.);
#7739=ORIENTED_EDGE('',*,*,#5391,.T.);
#7740=ORIENTED_EDGE('',*,*,#5392,.T.);
#7741=ORIENTED_EDGE('',*,*,#5384,.T.);
#7742=ORIENTED_EDGE('',*,*,#5367,.T.);
#7743=ORIENTED_EDGE('',*,*,#5381,.T.);
#7744=ORIENTED_EDGE('',*,*,#5353,.T.);
#7745=ORIENTED_EDGE('',*,*,#5361,.T.);
#7746=ORIENTED_EDGE('',*,*,#5385,.T.);
#7747=ORIENTED_EDGE('',*,*,#5358,.F.);
#7748=ORIENTED_EDGE('',*,*,#5383,.T.);
#7749=ORIENTED_EDGE('',*,*,#5393,.T.);
#7750=ORIENTED_EDGE('',*,*,#5394,.T.);
#7751=ORIENTED_EDGE('',*,*,#5392,.F.);
#7752=ORIENTED_EDGE('',*,*,#5395,.F.);
#7753=ORIENTED_EDGE('',*,*,#5396,.T.);
#7754=ORIENTED_EDGE('',*,*,#5395,.T.);
#7755=ORIENTED_EDGE('',*,*,#5391,.F.);
#7756=ORIENTED_EDGE('',*,*,#5397,.F.);
#7757=ORIENTED_EDGE('',*,*,#5398,.T.);
#7758=ORIENTED_EDGE('',*,*,#5397,.T.);
#7759=ORIENTED_EDGE('',*,*,#5390,.F.);
#7760=ORIENTED_EDGE('',*,*,#5399,.F.);
#7761=ORIENTED_EDGE('',*,*,#5400,.T.);
#7762=ORIENTED_EDGE('',*,*,#5399,.T.);
#7763=ORIENTED_EDGE('',*,*,#5389,.F.);
#7764=ORIENTED_EDGE('',*,*,#5401,.F.);
#7765=ORIENTED_EDGE('',*,*,#5402,.T.);
#7766=ORIENTED_EDGE('',*,*,#5401,.T.);
#7767=ORIENTED_EDGE('',*,*,#5388,.F.);
#7768=ORIENTED_EDGE('',*,*,#5403,.F.);
#7769=ORIENTED_EDGE('',*,*,#5404,.T.);
#7770=ORIENTED_EDGE('',*,*,#5403,.T.);
#7771=ORIENTED_EDGE('',*,*,#5387,.F.);
#7772=ORIENTED_EDGE('',*,*,#5394,.F.);
#7773=ORIENTED_EDGE('',*,*,#5404,.F.);
#7774=ORIENTED_EDGE('',*,*,#5393,.F.);
#7775=ORIENTED_EDGE('',*,*,#5396,.F.);
#7776=ORIENTED_EDGE('',*,*,#5398,.F.);
#7777=ORIENTED_EDGE('',*,*,#5400,.F.);
#7778=ORIENTED_EDGE('',*,*,#5402,.F.);
#7779=ORIENTED_EDGE('',*,*,#5386,.T.);
#7780=ORIENTED_EDGE('',*,*,#5363,.T.);
#7781=ORIENTED_EDGE('',*,*,#5382,.T.);
#7782=ORIENTED_EDGE('',*,*,#5377,.T.);
#7783=ORIENTED_EDGE('',*,*,#5405,.T.);
#7784=ORIENTED_EDGE('',*,*,#5406,.T.);
#7785=ORIENTED_EDGE('',*,*,#5407,.F.);
#7786=ORIENTED_EDGE('',*,*,#5408,.T.);
#7787=ORIENTED_EDGE('',*,*,#5409,.T.);
#7788=ORIENTED_EDGE('',*,*,#5410,.T.);
#7789=ORIENTED_EDGE('',*,*,#5405,.F.);
#7790=ORIENTED_EDGE('',*,*,#5411,.T.);
#7791=ORIENTED_EDGE('',*,*,#5412,.T.);
#7792=ORIENTED_EDGE('',*,*,#5413,.T.);
#7793=ORIENTED_EDGE('',*,*,#5409,.F.);
#7794=ORIENTED_EDGE('',*,*,#5414,.T.);
#7795=ORIENTED_EDGE('',*,*,#5415,.F.);
#7796=ORIENTED_EDGE('',*,*,#5416,.T.);
#7797=ORIENTED_EDGE('',*,*,#5417,.F.);
#7798=ORIENTED_EDGE('',*,*,#5418,.T.);
#7799=ORIENTED_EDGE('',*,*,#5419,.T.);
#7800=ORIENTED_EDGE('',*,*,#5420,.T.);
#7801=ORIENTED_EDGE('',*,*,#5421,.F.);
#7802=ORIENTED_EDGE('',*,*,#5422,.F.);
#7803=ORIENTED_EDGE('',*,*,#5423,.T.);
#7804=ORIENTED_EDGE('',*,*,#5424,.T.);
#7805=ORIENTED_EDGE('',*,*,#5419,.F.);
#7806=ORIENTED_EDGE('',*,*,#5425,.F.);
#7807=ORIENTED_EDGE('',*,*,#5426,.T.);
#7808=ORIENTED_EDGE('',*,*,#5427,.T.);
#7809=ORIENTED_EDGE('',*,*,#5423,.F.);
#7810=ORIENTED_EDGE('',*,*,#5428,.F.);
#7811=ORIENTED_EDGE('',*,*,#5429,.F.);
#7812=ORIENTED_EDGE('',*,*,#5430,.F.);
#7813=ORIENTED_EDGE('',*,*,#5431,.F.);
#7814=ORIENTED_EDGE('',*,*,#5432,.T.);
#7815=ORIENTED_EDGE('',*,*,#5429,.T.);
#7816=ORIENTED_EDGE('',*,*,#5433,.T.);
#7817=ORIENTED_EDGE('',*,*,#5426,.F.);
#7818=ORIENTED_EDGE('',*,*,#5434,.F.);
#7819=ORIENTED_EDGE('',*,*,#5435,.F.);
#7820=ORIENTED_EDGE('',*,*,#5420,.F.);
#7821=ORIENTED_EDGE('',*,*,#5424,.F.);
#7822=ORIENTED_EDGE('',*,*,#5427,.F.);
#7823=ORIENTED_EDGE('',*,*,#5433,.F.);
#7824=ORIENTED_EDGE('',*,*,#5432,.F.);
#7825=ORIENTED_EDGE('',*,*,#5436,.F.);
#7826=ORIENTED_EDGE('',*,*,#5416,.F.);
#7827=ORIENTED_EDGE('',*,*,#5437,.F.);
#7828=ORIENTED_EDGE('',*,*,#5414,.F.);
#7829=ORIENTED_EDGE('',*,*,#5411,.F.);
#7830=ORIENTED_EDGE('',*,*,#5408,.F.);
#7831=ORIENTED_EDGE('',*,*,#5438,.F.);
#7832=ORIENTED_EDGE('',*,*,#5406,.F.);
#7833=ORIENTED_EDGE('',*,*,#5410,.F.);
#7834=ORIENTED_EDGE('',*,*,#5413,.F.);
#7835=ORIENTED_EDGE('',*,*,#5439,.F.);
#7836=ORIENTED_EDGE('',*,*,#5418,.F.);
#7837=ORIENTED_EDGE('',*,*,#5440,.F.);
#7838=ORIENTED_EDGE('',*,*,#5430,.T.);
#7839=ORIENTED_EDGE('',*,*,#5434,.T.);
#7840=ORIENTED_EDGE('',*,*,#5428,.T.);
#7841=ORIENTED_EDGE('',*,*,#5425,.T.);
#7842=ORIENTED_EDGE('',*,*,#5422,.T.);
#7843=ORIENTED_EDGE('',*,*,#5441,.T.);
#7844=ORIENTED_EDGE('',*,*,#5442,.T.);
#7845=ORIENTED_EDGE('',*,*,#5443,.T.);
#7846=ORIENTED_EDGE('',*,*,#5444,.T.);
#7847=ORIENTED_EDGE('',*,*,#5445,.T.);
#7848=ORIENTED_EDGE('',*,*,#5446,.T.);
#7849=ORIENTED_EDGE('',*,*,#5438,.T.);
#7850=ORIENTED_EDGE('',*,*,#5421,.T.);
#7851=ORIENTED_EDGE('',*,*,#5435,.T.);
#7852=ORIENTED_EDGE('',*,*,#5407,.T.);
#7853=ORIENTED_EDGE('',*,*,#5415,.T.);
#7854=ORIENTED_EDGE('',*,*,#5439,.T.);
#7855=ORIENTED_EDGE('',*,*,#5412,.F.);
#7856=ORIENTED_EDGE('',*,*,#5437,.T.);
#7857=ORIENTED_EDGE('',*,*,#5447,.T.);
#7858=ORIENTED_EDGE('',*,*,#5448,.T.);
#7859=ORIENTED_EDGE('',*,*,#5446,.F.);
#7860=ORIENTED_EDGE('',*,*,#5449,.F.);
#7861=ORIENTED_EDGE('',*,*,#5450,.T.);
#7862=ORIENTED_EDGE('',*,*,#5449,.T.);
#7863=ORIENTED_EDGE('',*,*,#5445,.F.);
#7864=ORIENTED_EDGE('',*,*,#5451,.F.);
#7865=ORIENTED_EDGE('',*,*,#5452,.T.);
#7866=ORIENTED_EDGE('',*,*,#5451,.T.);
#7867=ORIENTED_EDGE('',*,*,#5444,.F.);
#7868=ORIENTED_EDGE('',*,*,#5453,.F.);
#7869=ORIENTED_EDGE('',*,*,#5454,.T.);
#7870=ORIENTED_EDGE('',*,*,#5453,.T.);
#7871=ORIENTED_EDGE('',*,*,#5443,.F.);
#7872=ORIENTED_EDGE('',*,*,#5455,.F.);
#7873=ORIENTED_EDGE('',*,*,#5456,.T.);
#7874=ORIENTED_EDGE('',*,*,#5455,.T.);
#7875=ORIENTED_EDGE('',*,*,#5442,.F.);
#7876=ORIENTED_EDGE('',*,*,#5457,.F.);
#7877=ORIENTED_EDGE('',*,*,#5458,.T.);
#7878=ORIENTED_EDGE('',*,*,#5457,.T.);
#7879=ORIENTED_EDGE('',*,*,#5441,.F.);
#7880=ORIENTED_EDGE('',*,*,#5448,.F.);
#7881=ORIENTED_EDGE('',*,*,#5458,.F.);
#7882=ORIENTED_EDGE('',*,*,#5447,.F.);
#7883=ORIENTED_EDGE('',*,*,#5450,.F.);
#7884=ORIENTED_EDGE('',*,*,#5452,.F.);
#7885=ORIENTED_EDGE('',*,*,#5454,.F.);
#7886=ORIENTED_EDGE('',*,*,#5456,.F.);
#7887=ORIENTED_EDGE('',*,*,#5440,.T.);
#7888=ORIENTED_EDGE('',*,*,#5417,.T.);
#7889=ORIENTED_EDGE('',*,*,#5436,.T.);
#7890=ORIENTED_EDGE('',*,*,#5431,.T.);
#7891=ORIENTED_EDGE('',*,*,#5459,.T.);
#7892=ORIENTED_EDGE('',*,*,#5460,.T.);
#7893=ORIENTED_EDGE('',*,*,#5461,.F.);
#7894=ORIENTED_EDGE('',*,*,#5462,.T.);
#7895=ORIENTED_EDGE('',*,*,#5463,.T.);
#7896=ORIENTED_EDGE('',*,*,#5464,.T.);
#7897=ORIENTED_EDGE('',*,*,#5459,.F.);
#7898=ORIENTED_EDGE('',*,*,#5465,.T.);
#7899=ORIENTED_EDGE('',*,*,#5466,.T.);
#7900=ORIENTED_EDGE('',*,*,#5467,.T.);
#7901=ORIENTED_EDGE('',*,*,#5463,.F.);
#7902=ORIENTED_EDGE('',*,*,#5468,.T.);
#7903=ORIENTED_EDGE('',*,*,#5469,.F.);
#7904=ORIENTED_EDGE('',*,*,#5470,.T.);
#7905=ORIENTED_EDGE('',*,*,#5471,.F.);
#7906=ORIENTED_EDGE('',*,*,#5472,.T.);
#7907=ORIENTED_EDGE('',*,*,#5473,.T.);
#7908=ORIENTED_EDGE('',*,*,#5474,.T.);
#7909=ORIENTED_EDGE('',*,*,#5475,.F.);
#7910=ORIENTED_EDGE('',*,*,#5476,.F.);
#7911=ORIENTED_EDGE('',*,*,#5477,.T.);
#7912=ORIENTED_EDGE('',*,*,#5478,.T.);
#7913=ORIENTED_EDGE('',*,*,#5473,.F.);
#7914=ORIENTED_EDGE('',*,*,#5479,.F.);
#7915=ORIENTED_EDGE('',*,*,#5480,.T.);
#7916=ORIENTED_EDGE('',*,*,#5481,.T.);
#7917=ORIENTED_EDGE('',*,*,#5477,.F.);
#7918=ORIENTED_EDGE('',*,*,#5482,.F.);
#7919=ORIENTED_EDGE('',*,*,#5483,.F.);
#7920=ORIENTED_EDGE('',*,*,#5484,.F.);
#7921=ORIENTED_EDGE('',*,*,#5485,.F.);
#7922=ORIENTED_EDGE('',*,*,#5486,.T.);
#7923=ORIENTED_EDGE('',*,*,#5483,.T.);
#7924=ORIENTED_EDGE('',*,*,#5487,.T.);
#7925=ORIENTED_EDGE('',*,*,#5480,.F.);
#7926=ORIENTED_EDGE('',*,*,#5488,.F.);
#7927=ORIENTED_EDGE('',*,*,#5489,.F.);
#7928=ORIENTED_EDGE('',*,*,#5474,.F.);
#7929=ORIENTED_EDGE('',*,*,#5478,.F.);
#7930=ORIENTED_EDGE('',*,*,#5481,.F.);
#7931=ORIENTED_EDGE('',*,*,#5487,.F.);
#7932=ORIENTED_EDGE('',*,*,#5486,.F.);
#7933=ORIENTED_EDGE('',*,*,#5490,.F.);
#7934=ORIENTED_EDGE('',*,*,#5470,.F.);
#7935=ORIENTED_EDGE('',*,*,#5491,.F.);
#7936=ORIENTED_EDGE('',*,*,#5468,.F.);
#7937=ORIENTED_EDGE('',*,*,#5465,.F.);
#7938=ORIENTED_EDGE('',*,*,#5462,.F.);
#7939=ORIENTED_EDGE('',*,*,#5492,.F.);
#7940=ORIENTED_EDGE('',*,*,#5460,.F.);
#7941=ORIENTED_EDGE('',*,*,#5464,.F.);
#7942=ORIENTED_EDGE('',*,*,#5467,.F.);
#7943=ORIENTED_EDGE('',*,*,#5493,.F.);
#7944=ORIENTED_EDGE('',*,*,#5472,.F.);
#7945=ORIENTED_EDGE('',*,*,#5494,.F.);
#7946=ORIENTED_EDGE('',*,*,#5484,.T.);
#7947=ORIENTED_EDGE('',*,*,#5488,.T.);
#7948=ORIENTED_EDGE('',*,*,#5482,.T.);
#7949=ORIENTED_EDGE('',*,*,#5479,.T.);
#7950=ORIENTED_EDGE('',*,*,#5476,.T.);
#7951=ORIENTED_EDGE('',*,*,#5495,.T.);
#7952=ORIENTED_EDGE('',*,*,#5496,.T.);
#7953=ORIENTED_EDGE('',*,*,#5497,.T.);
#7954=ORIENTED_EDGE('',*,*,#5498,.T.);
#7955=ORIENTED_EDGE('',*,*,#5499,.T.);
#7956=ORIENTED_EDGE('',*,*,#5500,.T.);
#7957=ORIENTED_EDGE('',*,*,#5492,.T.);
#7958=ORIENTED_EDGE('',*,*,#5475,.T.);
#7959=ORIENTED_EDGE('',*,*,#5489,.T.);
#7960=ORIENTED_EDGE('',*,*,#5461,.T.);
#7961=ORIENTED_EDGE('',*,*,#5469,.T.);
#7962=ORIENTED_EDGE('',*,*,#5493,.T.);
#7963=ORIENTED_EDGE('',*,*,#5466,.F.);
#7964=ORIENTED_EDGE('',*,*,#5491,.T.);
#7965=ORIENTED_EDGE('',*,*,#5501,.T.);
#7966=ORIENTED_EDGE('',*,*,#5502,.T.);
#7967=ORIENTED_EDGE('',*,*,#5500,.F.);
#7968=ORIENTED_EDGE('',*,*,#5503,.F.);
#7969=ORIENTED_EDGE('',*,*,#5504,.T.);
#7970=ORIENTED_EDGE('',*,*,#5503,.T.);
#7971=ORIENTED_EDGE('',*,*,#5499,.F.);
#7972=ORIENTED_EDGE('',*,*,#5505,.F.);
#7973=ORIENTED_EDGE('',*,*,#5506,.T.);
#7974=ORIENTED_EDGE('',*,*,#5505,.T.);
#7975=ORIENTED_EDGE('',*,*,#5498,.F.);
#7976=ORIENTED_EDGE('',*,*,#5507,.F.);
#7977=ORIENTED_EDGE('',*,*,#5508,.T.);
#7978=ORIENTED_EDGE('',*,*,#5507,.T.);
#7979=ORIENTED_EDGE('',*,*,#5497,.F.);
#7980=ORIENTED_EDGE('',*,*,#5509,.F.);
#7981=ORIENTED_EDGE('',*,*,#5510,.T.);
#7982=ORIENTED_EDGE('',*,*,#5509,.T.);
#7983=ORIENTED_EDGE('',*,*,#5496,.F.);
#7984=ORIENTED_EDGE('',*,*,#5511,.F.);
#7985=ORIENTED_EDGE('',*,*,#5512,.T.);
#7986=ORIENTED_EDGE('',*,*,#5511,.T.);
#7987=ORIENTED_EDGE('',*,*,#5495,.F.);
#7988=ORIENTED_EDGE('',*,*,#5502,.F.);
#7989=ORIENTED_EDGE('',*,*,#5512,.F.);
#7990=ORIENTED_EDGE('',*,*,#5501,.F.);
#7991=ORIENTED_EDGE('',*,*,#5504,.F.);
#7992=ORIENTED_EDGE('',*,*,#5506,.F.);
#7993=ORIENTED_EDGE('',*,*,#5508,.F.);
#7994=ORIENTED_EDGE('',*,*,#5510,.F.);
#7995=ORIENTED_EDGE('',*,*,#5494,.T.);
#7996=ORIENTED_EDGE('',*,*,#5471,.T.);
#7997=ORIENTED_EDGE('',*,*,#5490,.T.);
#7998=ORIENTED_EDGE('',*,*,#5485,.T.);
#7999=CYLINDRICAL_SURFACE('',#9046,0.15);
#8000=CYLINDRICAL_SURFACE('',#9050,0.15);
#8001=CYLINDRICAL_SURFACE('',#9054,0.25);
#8002=CYLINDRICAL_SURFACE('',#9057,0.25);
#8003=CYLINDRICAL_SURFACE('',#9060,0.25);
#8004=CYLINDRICAL_SURFACE('',#9063,0.25);
#8005=CYLINDRICAL_SURFACE('',#9073,1.188225);
#8006=CYLINDRICAL_SURFACE('',#9075,1.188225);
#8007=CYLINDRICAL_SURFACE('',#9076,1.188225);
#8008=CYLINDRICAL_SURFACE('',#9077,1.188225);
#8009=CYLINDRICAL_SURFACE('',#9078,1.188225);
#8010=CYLINDRICAL_SURFACE('',#9079,1.188225);
#8011=CYLINDRICAL_SURFACE('',#9080,1.188225);
#8012=CYLINDRICAL_SURFACE('',#9081,1.188225);
#8013=CYLINDRICAL_SURFACE('',#9082,1.188225);
#8014=CYLINDRICAL_SURFACE('',#9083,1.188225);
#8015=CYLINDRICAL_SURFACE('',#9084,1.188225);
#8016=CYLINDRICAL_SURFACE('',#9085,1.188225);
#8017=CYLINDRICAL_SURFACE('',#9086,1.188225);
#8018=CYLINDRICAL_SURFACE('',#9087,1.188225);
#8019=CYLINDRICAL_SURFACE('',#9088,1.188225);
#8020=CYLINDRICAL_SURFACE('',#9089,1.188225);
#8021=CYLINDRICAL_SURFACE('',#9090,1.188225);
#8022=CYLINDRICAL_SURFACE('',#9091,1.188225);
#8023=CYLINDRICAL_SURFACE('',#9092,1.188225);
#8024=CYLINDRICAL_SURFACE('',#9093,1.188225);
#8025=CYLINDRICAL_SURFACE('',#9094,1.188225);
#8026=CYLINDRICAL_SURFACE('',#9095,1.188225);
#8027=CYLINDRICAL_SURFACE('',#9096,1.188225);
#8028=CYLINDRICAL_SURFACE('',#9097,1.188225);
#8029=CYLINDRICAL_SURFACE('',#9098,1.188225);
#8030=CYLINDRICAL_SURFACE('',#9099,1.188225);
#8031=CYLINDRICAL_SURFACE('',#9100,1.188225);
#8032=CYLINDRICAL_SURFACE('',#9101,1.188225);
#8033=CYLINDRICAL_SURFACE('',#9102,1.188225);
#8034=CYLINDRICAL_SURFACE('',#9103,1.188225);
#8035=CYLINDRICAL_SURFACE('',#9104,1.188225);
#8036=CYLINDRICAL_SURFACE('',#9105,1.188225);
#8037=CYLINDRICAL_SURFACE('',#9106,1.188225);
#8038=CYLINDRICAL_SURFACE('',#9107,1.188225);
#8039=CYLINDRICAL_SURFACE('',#9108,1.188225);
#8040=CYLINDRICAL_SURFACE('',#9109,1.188225);
#8041=CYLINDRICAL_SURFACE('',#9110,1.188225);
#8042=CYLINDRICAL_SURFACE('',#9111,1.188225);
#8043=CYLINDRICAL_SURFACE('',#9112,1.188225);
#8044=CYLINDRICAL_SURFACE('',#9113,1.188225);
#8045=CYLINDRICAL_SURFACE('',#9114,1.188225);
#8046=CYLINDRICAL_SURFACE('',#9115,1.188225);
#8047=CYLINDRICAL_SURFACE('',#9116,1.188225);
#8048=CYLINDRICAL_SURFACE('',#9117,1.188225);
#8049=CYLINDRICAL_SURFACE('',#9118,1.188225);
#8050=CYLINDRICAL_SURFACE('',#9119,1.188225);
#8051=CYLINDRICAL_SURFACE('',#9120,1.188225);
#8052=CYLINDRICAL_SURFACE('',#9121,1.188225);
#8053=CYLINDRICAL_SURFACE('',#9122,1.188225);
#8054=CYLINDRICAL_SURFACE('',#9123,1.188225);
#8055=CYLINDRICAL_SURFACE('',#9124,1.188225);
#8056=CYLINDRICAL_SURFACE('',#9125,1.188225);
#8057=CYLINDRICAL_SURFACE('',#9126,1.188225);
#8058=CYLINDRICAL_SURFACE('',#9127,1.188225);
#8059=CYLINDRICAL_SURFACE('',#9128,1.188225);
#8060=CYLINDRICAL_SURFACE('',#9129,1.188225);
#8061=CYLINDRICAL_SURFACE('',#9130,1.188225);
#8062=CYLINDRICAL_SURFACE('',#9131,1.188225);
#8063=CYLINDRICAL_SURFACE('',#9132,1.188225);
#8064=CYLINDRICAL_SURFACE('',#9133,1.188225);
#8065=CYLINDRICAL_SURFACE('',#9134,1.188225);
#8066=CYLINDRICAL_SURFACE('',#9135,1.188225);
#8067=CYLINDRICAL_SURFACE('',#9136,1.188225);
#8068=CYLINDRICAL_SURFACE('',#9137,1.188225);
#8069=CYLINDRICAL_SURFACE('',#9138,1.188225);
#8070=CYLINDRICAL_SURFACE('',#9139,1.188225);
#8071=CYLINDRICAL_SURFACE('',#9140,1.188225);
#8072=CYLINDRICAL_SURFACE('',#9141,1.188225);
#8073=CYLINDRICAL_SURFACE('',#9142,1.188225);
#8074=CYLINDRICAL_SURFACE('',#9143,1.188225);
#8075=CYLINDRICAL_SURFACE('',#9144,1.188225);
#8076=CYLINDRICAL_SURFACE('',#9145,1.188225);
#8077=CYLINDRICAL_SURFACE('',#9146,1.188225);
#8078=CYLINDRICAL_SURFACE('',#9147,1.188225);
#8079=CYLINDRICAL_SURFACE('',#9148,1.188225);
#8080=CYLINDRICAL_SURFACE('',#9149,1.188225);
#8081=CYLINDRICAL_SURFACE('',#9150,1.188225);
#8082=CYLINDRICAL_SURFACE('',#9151,1.188225);
#8083=CYLINDRICAL_SURFACE('',#9152,1.188225);
#8084=CYLINDRICAL_SURFACE('',#9153,1.188225);
#8085=CYLINDRICAL_SURFACE('',#9154,1.188225);
#8086=CYLINDRICAL_SURFACE('',#9155,1.188225);
#8087=CYLINDRICAL_SURFACE('',#9156,1.188225);
#8088=CYLINDRICAL_SURFACE('',#9157,1.188225);
#8089=CYLINDRICAL_SURFACE('',#9158,1.188225);
#8090=CYLINDRICAL_SURFACE('',#9159,1.188225);
#8091=CYLINDRICAL_SURFACE('',#9160,1.188225);
#8092=CYLINDRICAL_SURFACE('',#9161,1.188225);
#8093=CYLINDRICAL_SURFACE('',#9162,1.188225);
#8094=CYLINDRICAL_SURFACE('',#9163,1.188225);
#8095=CYLINDRICAL_SURFACE('',#9164,1.188225);
#8096=CYLINDRICAL_SURFACE('',#9165,1.188225);
#8097=CYLINDRICAL_SURFACE('',#9166,1.188225);
#8098=CYLINDRICAL_SURFACE('',#9167,1.188225);
#8099=CYLINDRICAL_SURFACE('',#9168,1.016475);
#8100=CYLINDRICAL_SURFACE('',#9170,1.016475);
#8101=CYLINDRICAL_SURFACE('',#9171,1.016475);
#8102=CYLINDRICAL_SURFACE('',#9172,1.016475);
#8103=CYLINDRICAL_SURFACE('',#9173,1.016475);
#8104=CYLINDRICAL_SURFACE('',#9174,1.016475);
#8105=CYLINDRICAL_SURFACE('',#9175,1.016475);
#8106=CYLINDRICAL_SURFACE('',#9176,1.016475);
#8107=CYLINDRICAL_SURFACE('',#9177,1.016475);
#8108=CYLINDRICAL_SURFACE('',#9178,1.016475);
#8109=CYLINDRICAL_SURFACE('',#9179,1.016475);
#8110=CYLINDRICAL_SURFACE('',#9180,1.016475);
#8111=CYLINDRICAL_SURFACE('',#9181,1.016475);
#8112=CYLINDRICAL_SURFACE('',#9182,1.016475);
#8113=CYLINDRICAL_SURFACE('',#9183,1.016475);
#8114=CYLINDRICAL_SURFACE('',#9184,1.016475);
#8115=CYLINDRICAL_SURFACE('',#9185,1.016475);
#8116=CYLINDRICAL_SURFACE('',#9186,1.016475);
#8117=CYLINDRICAL_SURFACE('',#9187,1.016475);
#8118=CYLINDRICAL_SURFACE('',#9188,1.016475);
#8119=CYLINDRICAL_SURFACE('',#9189,1.016475);
#8120=CYLINDRICAL_SURFACE('',#9190,1.016475);
#8121=CYLINDRICAL_SURFACE('',#9191,1.016475);
#8122=CYLINDRICAL_SURFACE('',#9192,1.016475);
#8123=CYLINDRICAL_SURFACE('',#9193,1.016475);
#8124=CYLINDRICAL_SURFACE('',#9194,1.016475);
#8125=CYLINDRICAL_SURFACE('',#9195,1.016475);
#8126=CYLINDRICAL_SURFACE('',#9196,1.016475);
#8127=CYLINDRICAL_SURFACE('',#9197,1.016475);
#8128=CYLINDRICAL_SURFACE('',#9198,1.016475);
#8129=CYLINDRICAL_SURFACE('',#9199,1.016475);
#8130=CYLINDRICAL_SURFACE('',#9200,1.016475);
#8131=CYLINDRICAL_SURFACE('',#9201,1.016475);
#8132=CYLINDRICAL_SURFACE('',#9202,1.016475);
#8133=CYLINDRICAL_SURFACE('',#9203,1.016475);
#8134=CYLINDRICAL_SURFACE('',#9204,1.016475);
#8135=CYLINDRICAL_SURFACE('',#9205,1.016475);
#8136=CYLINDRICAL_SURFACE('',#9206,1.016475);
#8137=CYLINDRICAL_SURFACE('',#9207,1.016475);
#8138=CYLINDRICAL_SURFACE('',#9208,1.016475);
#8139=CYLINDRICAL_SURFACE('',#9209,1.016475);
#8140=CYLINDRICAL_SURFACE('',#9210,1.016475);
#8141=CYLINDRICAL_SURFACE('',#9211,1.016475);
#8142=CYLINDRICAL_SURFACE('',#9212,1.016475);
#8143=CYLINDRICAL_SURFACE('',#9213,1.016475);
#8144=CYLINDRICAL_SURFACE('',#9214,1.016475);
#8145=CYLINDRICAL_SURFACE('',#9215,1.016475);
#8146=CYLINDRICAL_SURFACE('',#9216,1.016475);
#8147=CYLINDRICAL_SURFACE('',#9217,1.016475);
#8148=CYLINDRICAL_SURFACE('',#9218,1.016475);
#8149=CYLINDRICAL_SURFACE('',#9219,1.016475);
#8150=CYLINDRICAL_SURFACE('',#9220,1.016475);
#8151=CYLINDRICAL_SURFACE('',#9221,1.016475);
#8152=CYLINDRICAL_SURFACE('',#9222,1.016475);
#8153=CYLINDRICAL_SURFACE('',#9223,1.016475);
#8154=CYLINDRICAL_SURFACE('',#9224,1.016475);
#8155=CYLINDRICAL_SURFACE('',#9225,1.016475);
#8156=CYLINDRICAL_SURFACE('',#9226,1.016475);
#8157=CYLINDRICAL_SURFACE('',#9227,1.016475);
#8158=CYLINDRICAL_SURFACE('',#9228,1.016475);
#8159=CYLINDRICAL_SURFACE('',#9229,1.016475);
#8160=CYLINDRICAL_SURFACE('',#9230,1.016475);
#8161=CYLINDRICAL_SURFACE('',#9231,1.016475);
#8162=CYLINDRICAL_SURFACE('',#9232,1.016475);
#8163=CYLINDRICAL_SURFACE('',#9233,1.016475);
#8164=CYLINDRICAL_SURFACE('',#9234,1.016475);
#8165=CYLINDRICAL_SURFACE('',#9235,1.016475);
#8166=CYLINDRICAL_SURFACE('',#9236,1.016475);
#8167=CYLINDRICAL_SURFACE('',#9237,1.016475);
#8168=CYLINDRICAL_SURFACE('',#9238,1.016475);
#8169=CYLINDRICAL_SURFACE('',#9239,1.016475);
#8170=CYLINDRICAL_SURFACE('',#9240,1.016475);
#8171=CYLINDRICAL_SURFACE('',#9241,1.016475);
#8172=CYLINDRICAL_SURFACE('',#9242,1.016475);
#8173=CYLINDRICAL_SURFACE('',#9243,1.016475);
#8174=CYLINDRICAL_SURFACE('',#9244,1.016475);
#8175=CYLINDRICAL_SURFACE('',#9245,1.016475);
#8176=CYLINDRICAL_SURFACE('',#9246,1.016475);
#8177=CYLINDRICAL_SURFACE('',#9247,1.016475);
#8178=CYLINDRICAL_SURFACE('',#9248,1.016475);
#8179=CYLINDRICAL_SURFACE('',#9249,1.016475);
#8180=CYLINDRICAL_SURFACE('',#9250,1.016475);
#8181=CYLINDRICAL_SURFACE('',#9251,1.016475);
#8182=CYLINDRICAL_SURFACE('',#9252,1.016475);
#8183=CYLINDRICAL_SURFACE('',#9253,1.016475);
#8184=CYLINDRICAL_SURFACE('',#9254,1.016475);
#8185=CYLINDRICAL_SURFACE('',#9255,1.016475);
#8186=CYLINDRICAL_SURFACE('',#9256,1.016475);
#8187=CYLINDRICAL_SURFACE('',#9257,1.016475);
#8188=CYLINDRICAL_SURFACE('',#9258,1.016475);
#8189=CYLINDRICAL_SURFACE('',#9259,1.016475);
#8190=CYLINDRICAL_SURFACE('',#9260,1.016475);
#8191=CYLINDRICAL_SURFACE('',#9261,1.016475);
#8192=CYLINDRICAL_SURFACE('',#9262,1.016475);
#8193=CYLINDRICAL_SURFACE('',#9263,0.15);
#8194=CYLINDRICAL_SURFACE('',#9266,0.15);
#8195=CYLINDRICAL_SURFACE('',#9269,0.33);
#8196=CYLINDRICAL_SURFACE('',#9272,0.33);
#8197=CYLINDRICAL_SURFACE('',#9275,0.33);
#8198=CYLINDRICAL_SURFACE('',#9278,0.33);
#8199=CYLINDRICAL_SURFACE('',#9284,3.8);
#8200=CYLINDRICAL_SURFACE('',#9287,1.016475);
#8201=CYLINDRICAL_SURFACE('',#9290,1.188225);
#8202=CYLINDRICAL_SURFACE('',#9292,0.15);
#8203=CYLINDRICAL_SURFACE('',#9298,0.15);
#8204=CYLINDRICAL_SURFACE('',#9304,1.1);
#8205=CYLINDRICAL_SURFACE('',#9311,1.21);
#8206=CYLINDRICAL_SURFACE('',#9314,2.);
#8207=CYLINDRICAL_SURFACE('',#9327,2.);
#8208=CYLINDRICAL_SURFACE('',#9328,2.);
#8209=CYLINDRICAL_SURFACE('',#9330,0.425);
#8210=CYLINDRICAL_SURFACE('',#9339,0.425);
#8211=CYLINDRICAL_SURFACE('',#9349,1.1);
#8212=CYLINDRICAL_SURFACE('',#9356,2.);
#8213=CYLINDRICAL_SURFACE('',#9359,0.425);
#8214=CYLINDRICAL_SURFACE('',#9368,0.425);
#8215=CYLINDRICAL_SURFACE('',#9383,1.);
#8216=CYLINDRICAL_SURFACE('',#9385,1.1);
#8217=CYLINDRICAL_SURFACE('',#9394,1.);
#8218=CYLINDRICAL_SURFACE('',#9396,1.1);
#8219=CYLINDRICAL_SURFACE('',#9400,3.1);
#8220=CYLINDRICAL_SURFACE('',#9410,1.21);
#8221=CYLINDRICAL_SURFACE('',#9413,2.);
#8222=CYLINDRICAL_SURFACE('',#9425,4.2);
#8223=CYLINDRICAL_SURFACE('',#9426,0.425);
#8224=CYLINDRICAL_SURFACE('',#9435,0.425);
#8225=CYLINDRICAL_SURFACE('',#9445,3.1);
#8226=CYLINDRICAL_SURFACE('',#9452,4.2);
#8227=CYLINDRICAL_SURFACE('',#9455,0.425);
#8228=CYLINDRICAL_SURFACE('',#9464,0.425);
#8229=CYLINDRICAL_SURFACE('',#9479,3.);
#8230=CYLINDRICAL_SURFACE('',#9481,3.1);
#8231=CYLINDRICAL_SURFACE('',#9490,3.);
#8232=CYLINDRICAL_SURFACE('',#9492,3.1);
#8233=CYLINDRICAL_SURFACE('',#9524,0.5);
#8234=CYLINDRICAL_SURFACE('',#9532,0.2942);
#8235=CYLINDRICAL_SURFACE('',#9545,0.4);
#8236=CYLINDRICAL_SURFACE('',#9552,0.65);
#8237=CYLINDRICAL_SURFACE('',#9560,0.3933);
#8238=CYLINDRICAL_SURFACE('',#9562,0.42);
#8239=CYLINDRICAL_SURFACE('',#9565,0.8);
#8240=CYLINDRICAL_SURFACE('',#9578,0.338975);
#8241=CYLINDRICAL_SURFACE('',#9622,1.0501);
#8242=CYLINDRICAL_SURFACE('',#9624,1.0501);
#8243=CYLINDRICAL_SURFACE('',#9625,1.0501);
#8244=CYLINDRICAL_SURFACE('',#9626,1.0501);
#8245=CYLINDRICAL_SURFACE('',#9628,1.21745);
#8246=CYLINDRICAL_SURFACE('',#9630,1.21745);
#8247=CYLINDRICAL_SURFACE('',#9631,1.21745);
#8248=CYLINDRICAL_SURFACE('',#9632,1.21745);
#8249=CYLINDRICAL_SURFACE('',#9634,1.21745);
#8250=CYLINDRICAL_SURFACE('',#9636,1.0501);
#8251=CYLINDRICAL_SURFACE('',#9647,1.0501);
#8252=CYLINDRICAL_SURFACE('',#9649,1.0501);
#8253=CYLINDRICAL_SURFACE('',#9650,1.0501);
#8254=CYLINDRICAL_SURFACE('',#9651,1.0501);
#8255=CYLINDRICAL_SURFACE('',#9653,1.21745);
#8256=CYLINDRICAL_SURFACE('',#9655,1.21745);
#8257=CYLINDRICAL_SURFACE('',#9656,1.21745);
#8258=CYLINDRICAL_SURFACE('',#9657,1.21745);
#8259=CYLINDRICAL_SURFACE('',#9659,1.21745);
#8260=CYLINDRICAL_SURFACE('',#9661,1.0501);
#8261=CYLINDRICAL_SURFACE('',#9672,1.0501);
#8262=CYLINDRICAL_SURFACE('',#9674,1.0501);
#8263=CYLINDRICAL_SURFACE('',#9675,1.0501);
#8264=CYLINDRICAL_SURFACE('',#9676,1.0501);
#8265=CYLINDRICAL_SURFACE('',#9678,1.21745);
#8266=CYLINDRICAL_SURFACE('',#9680,1.21745);
#8267=CYLINDRICAL_SURFACE('',#9681,1.21745);
#8268=CYLINDRICAL_SURFACE('',#9682,1.21745);
#8269=CYLINDRICAL_SURFACE('',#9684,1.21745);
#8270=CYLINDRICAL_SURFACE('',#9686,1.0501);
#8271=CYLINDRICAL_SURFACE('',#9697,1.0501);
#8272=CYLINDRICAL_SURFACE('',#9699,1.0501);
#8273=CYLINDRICAL_SURFACE('',#9700,1.0501);
#8274=CYLINDRICAL_SURFACE('',#9701,1.0501);
#8275=CYLINDRICAL_SURFACE('',#9703,1.21745);
#8276=CYLINDRICAL_SURFACE('',#9705,1.21745);
#8277=CYLINDRICAL_SURFACE('',#9706,1.21745);
#8278=CYLINDRICAL_SURFACE('',#9707,1.21745);
#8279=CYLINDRICAL_SURFACE('',#9709,1.21745);
#8280=CYLINDRICAL_SURFACE('',#9711,1.0501);
#8281=ADVANCED_FACE('',(#1044),#7999,.F.);
#8282=ADVANCED_FACE('',(#1045),#857,.T.);
#8283=ADVANCED_FACE('',(#1046),#8000,.F.);
#8284=ADVANCED_FACE('',(#1047),#858,.T.);
#8285=ADVANCED_FACE('',(#1048),#8001,.F.);
#8286=ADVANCED_FACE('',(#1049),#8002,.F.);
#8287=ADVANCED_FACE('',(#1050),#8003,.F.);
#8288=ADVANCED_FACE('',(#1051),#8004,.F.);
#8289=ADVANCED_FACE('',(#1052),#859,.T.);
#8290=ADVANCED_FACE('',(#1053),#860,.T.);
#8291=ADVANCED_FACE('',(#1054),#861,.T.);
#8292=ADVANCED_FACE('',(#1055),#862,.T.);
#8293=ADVANCED_FACE('',(#1056,#799,#800,#801,#802,#803,#804),#863,.T.);
#8294=ADVANCED_FACE('',(#1057,#805,#806,#807,#808),#864,.F.);
#8295=ADVANCED_FACE('',(#1058),#8005,.T.);
#8296=ADVANCED_FACE('',(#1059),#8006,.T.);
#8297=ADVANCED_FACE('',(#1060),#8007,.T.);
#8298=ADVANCED_FACE('',(#1061),#8008,.T.);
#8299=ADVANCED_FACE('',(#1062),#8009,.T.);
#8300=ADVANCED_FACE('',(#1063),#8010,.T.);
#8301=ADVANCED_FACE('',(#1064),#8011,.T.);
#8302=ADVANCED_FACE('',(#1065),#8012,.T.);
#8303=ADVANCED_FACE('',(#1066),#8013,.T.);
#8304=ADVANCED_FACE('',(#1067),#8014,.T.);
#8305=ADVANCED_FACE('',(#1068),#8015,.T.);
#8306=ADVANCED_FACE('',(#1069),#8016,.T.);
#8307=ADVANCED_FACE('',(#1070),#8017,.T.);
#8308=ADVANCED_FACE('',(#1071),#8018,.T.);
#8309=ADVANCED_FACE('',(#1072),#8019,.T.);
#8310=ADVANCED_FACE('',(#1073),#8020,.T.);
#8311=ADVANCED_FACE('',(#1074),#8021,.T.);
#8312=ADVANCED_FACE('',(#1075),#8022,.T.);
#8313=ADVANCED_FACE('',(#1076),#8023,.T.);
#8314=ADVANCED_FACE('',(#1077),#8024,.T.);
#8315=ADVANCED_FACE('',(#1078),#8025,.T.);
#8316=ADVANCED_FACE('',(#1079),#8026,.T.);
#8317=ADVANCED_FACE('',(#1080),#8027,.T.);
#8318=ADVANCED_FACE('',(#1081),#8028,.T.);
#8319=ADVANCED_FACE('',(#1082),#8029,.T.);
#8320=ADVANCED_FACE('',(#1083),#8030,.T.);
#8321=ADVANCED_FACE('',(#1084),#8031,.T.);
#8322=ADVANCED_FACE('',(#1085),#8032,.T.);
#8323=ADVANCED_FACE('',(#1086),#8033,.T.);
#8324=ADVANCED_FACE('',(#1087),#8034,.T.);
#8325=ADVANCED_FACE('',(#1088),#8035,.T.);
#8326=ADVANCED_FACE('',(#1089),#8036,.T.);
#8327=ADVANCED_FACE('',(#1090),#8037,.T.);
#8328=ADVANCED_FACE('',(#1091),#8038,.T.);
#8329=ADVANCED_FACE('',(#1092),#8039,.T.);
#8330=ADVANCED_FACE('',(#1093),#8040,.T.);
#8331=ADVANCED_FACE('',(#1094),#8041,.T.);
#8332=ADVANCED_FACE('',(#1095),#8042,.T.);
#8333=ADVANCED_FACE('',(#1096),#8043,.T.);
#8334=ADVANCED_FACE('',(#1097),#8044,.T.);
#8335=ADVANCED_FACE('',(#1098),#8045,.T.);
#8336=ADVANCED_FACE('',(#1099),#8046,.T.);
#8337=ADVANCED_FACE('',(#1100),#8047,.T.);
#8338=ADVANCED_FACE('',(#1101),#8048,.T.);
#8339=ADVANCED_FACE('',(#1102),#8049,.T.);
#8340=ADVANCED_FACE('',(#1103),#8050,.T.);
#8341=ADVANCED_FACE('',(#1104),#8051,.T.);
#8342=ADVANCED_FACE('',(#1105),#8052,.T.);
#8343=ADVANCED_FACE('',(#1106),#8053,.T.);
#8344=ADVANCED_FACE('',(#1107),#8054,.T.);
#8345=ADVANCED_FACE('',(#1108),#8055,.T.);
#8346=ADVANCED_FACE('',(#1109),#8056,.T.);
#8347=ADVANCED_FACE('',(#1110),#8057,.T.);
#8348=ADVANCED_FACE('',(#1111),#8058,.T.);
#8349=ADVANCED_FACE('',(#1112),#8059,.T.);
#8350=ADVANCED_FACE('',(#1113),#8060,.T.);
#8351=ADVANCED_FACE('',(#1114),#8061,.T.);
#8352=ADVANCED_FACE('',(#1115),#8062,.T.);
#8353=ADVANCED_FACE('',(#1116),#8063,.T.);
#8354=ADVANCED_FACE('',(#1117),#8064,.T.);
#8355=ADVANCED_FACE('',(#1118),#8065,.T.);
#8356=ADVANCED_FACE('',(#1119),#8066,.T.);
#8357=ADVANCED_FACE('',(#1120),#8067,.T.);
#8358=ADVANCED_FACE('',(#1121),#8068,.T.);
#8359=ADVANCED_FACE('',(#1122),#8069,.T.);
#8360=ADVANCED_FACE('',(#1123),#8070,.T.);
#8361=ADVANCED_FACE('',(#1124),#8071,.T.);
#8362=ADVANCED_FACE('',(#1125),#8072,.T.);
#8363=ADVANCED_FACE('',(#1126),#8073,.T.);
#8364=ADVANCED_FACE('',(#1127),#8074,.T.);
#8365=ADVANCED_FACE('',(#1128),#8075,.T.);
#8366=ADVANCED_FACE('',(#1129),#8076,.T.);
#8367=ADVANCED_FACE('',(#1130),#8077,.T.);
#8368=ADVANCED_FACE('',(#1131),#8078,.T.);
#8369=ADVANCED_FACE('',(#1132),#8079,.T.);
#8370=ADVANCED_FACE('',(#1133),#8080,.T.);
#8371=ADVANCED_FACE('',(#1134),#8081,.T.);
#8372=ADVANCED_FACE('',(#1135),#8082,.T.);
#8373=ADVANCED_FACE('',(#1136),#8083,.T.);
#8374=ADVANCED_FACE('',(#1137),#8084,.T.);
#8375=ADVANCED_FACE('',(#1138),#8085,.T.);
#8376=ADVANCED_FACE('',(#1139),#8086,.T.);
#8377=ADVANCED_FACE('',(#1140),#8087,.T.);
#8378=ADVANCED_FACE('',(#1141),#8088,.T.);
#8379=ADVANCED_FACE('',(#1142),#8089,.T.);
#8380=ADVANCED_FACE('',(#1143),#8090,.T.);
#8381=ADVANCED_FACE('',(#1144),#8091,.T.);
#8382=ADVANCED_FACE('',(#1145),#8092,.T.);
#8383=ADVANCED_FACE('',(#1146),#8093,.T.);
#8384=ADVANCED_FACE('',(#1147),#8094,.T.);
#8385=ADVANCED_FACE('',(#1148),#8095,.T.);
#8386=ADVANCED_FACE('',(#1149),#8096,.T.);
#8387=ADVANCED_FACE('',(#1150),#8097,.T.);
#8388=ADVANCED_FACE('',(#1151),#8098,.T.);
#8389=ADVANCED_FACE('',(#1152),#8099,.T.);
#8390=ADVANCED_FACE('',(#1153),#8100,.T.);
#8391=ADVANCED_FACE('',(#1154),#8101,.T.);
#8392=ADVANCED_FACE('',(#1155),#8102,.T.);
#8393=ADVANCED_FACE('',(#1156),#8103,.T.);
#8394=ADVANCED_FACE('',(#1157),#8104,.T.);
#8395=ADVANCED_FACE('',(#1158),#8105,.T.);
#8396=ADVANCED_FACE('',(#1159),#8106,.T.);
#8397=ADVANCED_FACE('',(#1160),#8107,.T.);
#8398=ADVANCED_FACE('',(#1161),#8108,.T.);
#8399=ADVANCED_FACE('',(#1162),#8109,.T.);
#8400=ADVANCED_FACE('',(#1163),#8110,.T.);
#8401=ADVANCED_FACE('',(#1164),#8111,.T.);
#8402=ADVANCED_FACE('',(#1165),#8112,.T.);
#8403=ADVANCED_FACE('',(#1166),#8113,.T.);
#8404=ADVANCED_FACE('',(#1167),#8114,.T.);
#8405=ADVANCED_FACE('',(#1168),#8115,.T.);
#8406=ADVANCED_FACE('',(#1169),#8116,.T.);
#8407=ADVANCED_FACE('',(#1170),#8117,.T.);
#8408=ADVANCED_FACE('',(#1171),#8118,.T.);
#8409=ADVANCED_FACE('',(#1172),#8119,.T.);
#8410=ADVANCED_FACE('',(#1173),#8120,.T.);
#8411=ADVANCED_FACE('',(#1174),#8121,.T.);
#8412=ADVANCED_FACE('',(#1175),#8122,.T.);
#8413=ADVANCED_FACE('',(#1176),#8123,.T.);
#8414=ADVANCED_FACE('',(#1177),#8124,.T.);
#8415=ADVANCED_FACE('',(#1178),#8125,.T.);
#8416=ADVANCED_FACE('',(#1179),#8126,.T.);
#8417=ADVANCED_FACE('',(#1180),#8127,.T.);
#8418=ADVANCED_FACE('',(#1181),#8128,.T.);
#8419=ADVANCED_FACE('',(#1182),#8129,.T.);
#8420=ADVANCED_FACE('',(#1183),#8130,.T.);
#8421=ADVANCED_FACE('',(#1184),#8131,.T.);
#8422=ADVANCED_FACE('',(#1185),#8132,.T.);
#8423=ADVANCED_FACE('',(#1186),#8133,.T.);
#8424=ADVANCED_FACE('',(#1187),#8134,.T.);
#8425=ADVANCED_FACE('',(#1188),#8135,.T.);
#8426=ADVANCED_FACE('',(#1189),#8136,.T.);
#8427=ADVANCED_FACE('',(#1190),#8137,.T.);
#8428=ADVANCED_FACE('',(#1191),#8138,.T.);
#8429=ADVANCED_FACE('',(#1192),#8139,.T.);
#8430=ADVANCED_FACE('',(#1193),#8140,.T.);
#8431=ADVANCED_FACE('',(#1194),#8141,.T.);
#8432=ADVANCED_FACE('',(#1195),#8142,.T.);
#8433=ADVANCED_FACE('',(#1196),#8143,.T.);
#8434=ADVANCED_FACE('',(#1197),#8144,.T.);
#8435=ADVANCED_FACE('',(#1198),#8145,.T.);
#8436=ADVANCED_FACE('',(#1199),#8146,.T.);
#8437=ADVANCED_FACE('',(#1200),#8147,.T.);
#8438=ADVANCED_FACE('',(#1201),#8148,.T.);
#8439=ADVANCED_FACE('',(#1202),#8149,.T.);
#8440=ADVANCED_FACE('',(#1203),#8150,.T.);
#8441=ADVANCED_FACE('',(#1204),#8151,.T.);
#8442=ADVANCED_FACE('',(#1205),#8152,.T.);
#8443=ADVANCED_FACE('',(#1206),#8153,.T.);
#8444=ADVANCED_FACE('',(#1207),#8154,.T.);
#8445=ADVANCED_FACE('',(#1208),#8155,.T.);
#8446=ADVANCED_FACE('',(#1209),#8156,.T.);
#8447=ADVANCED_FACE('',(#1210),#8157,.T.);
#8448=ADVANCED_FACE('',(#1211),#8158,.T.);
#8449=ADVANCED_FACE('',(#1212),#8159,.T.);
#8450=ADVANCED_FACE('',(#1213),#8160,.T.);
#8451=ADVANCED_FACE('',(#1214),#8161,.T.);
#8452=ADVANCED_FACE('',(#1215),#8162,.T.);
#8453=ADVANCED_FACE('',(#1216),#8163,.T.);
#8454=ADVANCED_FACE('',(#1217),#8164,.T.);
#8455=ADVANCED_FACE('',(#1218),#8165,.T.);
#8456=ADVANCED_FACE('',(#1219),#8166,.T.);
#8457=ADVANCED_FACE('',(#1220),#8167,.T.);
#8458=ADVANCED_FACE('',(#1221),#8168,.T.);
#8459=ADVANCED_FACE('',(#1222),#8169,.T.);
#8460=ADVANCED_FACE('',(#1223),#8170,.T.);
#8461=ADVANCED_FACE('',(#1224),#8171,.T.);
#8462=ADVANCED_FACE('',(#1225),#8172,.T.);
#8463=ADVANCED_FACE('',(#1226),#8173,.T.);
#8464=ADVANCED_FACE('',(#1227),#8174,.T.);
#8465=ADVANCED_FACE('',(#1228),#8175,.T.);
#8466=ADVANCED_FACE('',(#1229),#8176,.T.);
#8467=ADVANCED_FACE('',(#1230),#8177,.T.);
#8468=ADVANCED_FACE('',(#1231),#8178,.T.);
#8469=ADVANCED_FACE('',(#1232),#8179,.T.);
#8470=ADVANCED_FACE('',(#1233),#8180,.T.);
#8471=ADVANCED_FACE('',(#1234),#8181,.T.);
#8472=ADVANCED_FACE('',(#1235),#8182,.T.);
#8473=ADVANCED_FACE('',(#1236),#8183,.T.);
#8474=ADVANCED_FACE('',(#1237),#8184,.T.);
#8475=ADVANCED_FACE('',(#1238),#8185,.T.);
#8476=ADVANCED_FACE('',(#1239),#8186,.T.);
#8477=ADVANCED_FACE('',(#1240),#8187,.T.);
#8478=ADVANCED_FACE('',(#1241),#8188,.T.);
#8479=ADVANCED_FACE('',(#1242),#8189,.T.);
#8480=ADVANCED_FACE('',(#1243),#8190,.T.);
#8481=ADVANCED_FACE('',(#1244),#8191,.T.);
#8482=ADVANCED_FACE('',(#1245),#8192,.T.);
#8483=ADVANCED_FACE('',(#1246),#8193,.F.);
#8484=ADVANCED_FACE('',(#1247),#8194,.F.);
#8485=ADVANCED_FACE('',(#1248),#8195,.F.);
#8486=ADVANCED_FACE('',(#1249),#8196,.F.);
#8487=ADVANCED_FACE('',(#1250),#8197,.F.);
#8488=ADVANCED_FACE('',(#1251),#8198,.F.);
#8489=ADVANCED_FACE('',(#1252,#809,#810,#811,#812,#813,#814,#815),#865,
 .T.);
#8490=ADVANCED_FACE('',(#1253),#8199,.T.);
#8491=ADVANCED_FACE('',(#1254,#816,#817,#818,#819,#820,#821),#866,.F.);
#8492=ADVANCED_FACE('',(#1255),#207,.F.);
#8493=ADVANCED_FACE('',(#1256),#8200,.T.);
#8494=ADVANCED_FACE('',(#1257),#208,.F.);
#8495=ADVANCED_FACE('',(#1258),#867,.T.);
#8496=ADVANCED_FACE('',(#1259),#8201,.T.);
#8497=ADVANCED_FACE('',(#1260),#8202,.T.);
#8498=ADVANCED_FACE('',(#1261),#868,.T.);
#8499=ADVANCED_FACE('',(#1262),#869,.F.);
#8500=ADVANCED_FACE('',(#1263),#8203,.T.);
#8501=ADVANCED_FACE('',(#1264),#870,.T.);
#8502=ADVANCED_FACE('',(#1265),#871,.F.);
#8503=ADVANCED_FACE('',(#1266),#8204,.F.);
#8504=ADVANCED_FACE('',(#1267),#872,.T.);
#8505=ADVANCED_FACE('',(#1268),#873,.F.);
#8506=ADVANCED_FACE('',(#1269),#8205,.F.);
#8507=ADVANCED_FACE('',(#1270),#8206,.T.);
#8508=ADVANCED_FACE('',(#1271),#874,.F.);
#8509=ADVANCED_FACE('',(#1272,#822),#875,.T.);
#8510=ADVANCED_FACE('',(#1273),#876,.T.);
#8511=ADVANCED_FACE('',(#1274),#877,.T.);
#8512=ADVANCED_FACE('',(#1275,#823),#878,.T.);
#8513=ADVANCED_FACE('',(#1276),#879,.T.);
#8514=ADVANCED_FACE('',(#1277),#880,.T.);
#8515=ADVANCED_FACE('',(#1278),#881,.F.);
#8516=ADVANCED_FACE('',(#1279),#8207,.T.);
#8517=ADVANCED_FACE('',(#1280),#8208,.T.);
#8518=ADVANCED_FACE('',(#1281),#882,.F.);
#8519=ADVANCED_FACE('',(#1282),#8209,.F.);
#8520=ADVANCED_FACE('',(#1283),#883,.T.);
#8521=ADVANCED_FACE('',(#1284,#824),#884,.T.);
#8522=ADVANCED_FACE('',(#1285),#885,.T.);
#8523=ADVANCED_FACE('',(#1286,#825),#886,.T.);
#8524=ADVANCED_FACE('',(#1287),#887,.T.);
#8525=ADVANCED_FACE('',(#1288),#888,.F.);
#8526=ADVANCED_FACE('',(#1289),#8210,.F.);
#8527=ADVANCED_FACE('',(#1290),#889,.T.);
#8528=ADVANCED_FACE('',(#1291,#826),#890,.T.);
#8529=ADVANCED_FACE('',(#1292),#891,.T.);
#8530=ADVANCED_FACE('',(#1293,#827),#892,.T.);
#8531=ADVANCED_FACE('',(#1294),#893,.T.);
#8532=ADVANCED_FACE('',(#1295),#894,.F.);
#8533=ADVANCED_FACE('',(#1296),#8211,.F.);
#8534=ADVANCED_FACE('',(#1297),#895,.T.);
#8535=ADVANCED_FACE('',(#1298),#896,.F.);
#8536=ADVANCED_FACE('',(#1299),#897,.F.);
#8537=ADVANCED_FACE('',(#1300),#8212,.T.);
#8538=ADVANCED_FACE('',(#1301),#898,.F.);
#8539=ADVANCED_FACE('',(#1302),#8213,.F.);
#8540=ADVANCED_FACE('',(#1303),#899,.T.);
#8541=ADVANCED_FACE('',(#1304,#828),#900,.T.);
#8542=ADVANCED_FACE('',(#1305),#901,.T.);
#8543=ADVANCED_FACE('',(#1306,#829),#902,.T.);
#8544=ADVANCED_FACE('',(#1307),#903,.T.);
#8545=ADVANCED_FACE('',(#1308),#904,.F.);
#8546=ADVANCED_FACE('',(#1309),#8214,.F.);
#8547=ADVANCED_FACE('',(#1310),#905,.T.);
#8548=ADVANCED_FACE('',(#1311,#830),#906,.T.);
#8549=ADVANCED_FACE('',(#1312),#907,.T.);
#8550=ADVANCED_FACE('',(#1313,#831),#908,.T.);
#8551=ADVANCED_FACE('',(#1314),#909,.T.);
#8552=ADVANCED_FACE('',(#1315),#910,.F.);
#8553=ADVANCED_FACE('',(#1316),#911,.F.);
#8554=ADVANCED_FACE('',(#1317),#912,.F.);
#8555=ADVANCED_FACE('',(#1318),#913,.F.);
#8556=ADVANCED_FACE('',(#1319),#8215,.F.);
#8557=ADVANCED_FACE('',(#1320),#8216,.T.);
#8558=ADVANCED_FACE('',(#1321),#914,.T.);
#8559=ADVANCED_FACE('',(#1322),#915,.F.);
#8560=ADVANCED_FACE('',(#1323),#916,.F.);
#8561=ADVANCED_FACE('',(#1324),#917,.F.);
#8562=ADVANCED_FACE('',(#1325),#8217,.F.);
#8563=ADVANCED_FACE('',(#1326),#8218,.T.);
#8564=ADVANCED_FACE('',(#1327),#918,.T.);
#8565=ADVANCED_FACE('',(#1328),#8219,.F.);
#8566=ADVANCED_FACE('',(#1329),#919,.F.);
#8567=ADVANCED_FACE('',(#1330),#920,.F.);
#8568=ADVANCED_FACE('',(#1331),#921,.F.);
#8569=ADVANCED_FACE('',(#1332),#922,.T.);
#8570=ADVANCED_FACE('',(#1333),#8220,.F.);
#8571=ADVANCED_FACE('',(#1334),#8221,.T.);
#8572=ADVANCED_FACE('',(#1335),#923,.F.);
#8573=ADVANCED_FACE('',(#1336,#832),#924,.T.);
#8574=ADVANCED_FACE('',(#1337),#925,.T.);
#8575=ADVANCED_FACE('',(#1338),#926,.T.);
#8576=ADVANCED_FACE('',(#1339,#833),#927,.T.);
#8577=ADVANCED_FACE('',(#1340),#928,.T.);
#8578=ADVANCED_FACE('',(#1341),#929,.F.);
#8579=ADVANCED_FACE('',(#1342),#930,.T.);
#8580=ADVANCED_FACE('',(#1343),#8222,.T.);
#8581=ADVANCED_FACE('',(#1344),#8223,.F.);
#8582=ADVANCED_FACE('',(#1345),#931,.T.);
#8583=ADVANCED_FACE('',(#1346,#834),#932,.T.);
#8584=ADVANCED_FACE('',(#1347),#933,.T.);
#8585=ADVANCED_FACE('',(#1348,#835),#934,.T.);
#8586=ADVANCED_FACE('',(#1349),#935,.T.);
#8587=ADVANCED_FACE('',(#1350),#936,.F.);
#8588=ADVANCED_FACE('',(#1351),#8224,.F.);
#8589=ADVANCED_FACE('',(#1352),#937,.T.);
#8590=ADVANCED_FACE('',(#1353,#836),#938,.T.);
#8591=ADVANCED_FACE('',(#1354),#939,.T.);
#8592=ADVANCED_FACE('',(#1355,#837),#940,.T.);
#8593=ADVANCED_FACE('',(#1356),#941,.T.);
#8594=ADVANCED_FACE('',(#1357),#942,.F.);
#8595=ADVANCED_FACE('',(#1358),#8225,.F.);
#8596=ADVANCED_FACE('',(#1359),#943,.T.);
#8597=ADVANCED_FACE('',(#1360),#944,.F.);
#8598=ADVANCED_FACE('',(#1361),#945,.F.);
#8599=ADVANCED_FACE('',(#1362),#8226,.T.);
#8600=ADVANCED_FACE('',(#1363),#946,.F.);
#8601=ADVANCED_FACE('',(#1364),#8227,.F.);
#8602=ADVANCED_FACE('',(#1365),#947,.T.);
#8603=ADVANCED_FACE('',(#1366,#838),#948,.T.);
#8604=ADVANCED_FACE('',(#1367),#949,.T.);
#8605=ADVANCED_FACE('',(#1368,#839),#950,.T.);
#8606=ADVANCED_FACE('',(#1369),#951,.T.);
#8607=ADVANCED_FACE('',(#1370),#952,.F.);
#8608=ADVANCED_FACE('',(#1371),#8228,.F.);
#8609=ADVANCED_FACE('',(#1372),#953,.T.);
#8610=ADVANCED_FACE('',(#1373,#840),#954,.T.);
#8611=ADVANCED_FACE('',(#1374),#955,.T.);
#8612=ADVANCED_FACE('',(#1375,#841),#956,.T.);
#8613=ADVANCED_FACE('',(#1376),#957,.T.);
#8614=ADVANCED_FACE('',(#1377),#958,.F.);
#8615=ADVANCED_FACE('',(#1378),#959,.F.);
#8616=ADVANCED_FACE('',(#1379),#960,.F.);
#8617=ADVANCED_FACE('',(#1380),#961,.F.);
#8618=ADVANCED_FACE('',(#1381),#8229,.F.);
#8619=ADVANCED_FACE('',(#1382),#8230,.T.);
#8620=ADVANCED_FACE('',(#1383),#962,.T.);
#8621=ADVANCED_FACE('',(#1384),#963,.F.);
#8622=ADVANCED_FACE('',(#1385),#964,.F.);
#8623=ADVANCED_FACE('',(#1386),#965,.F.);
#8624=ADVANCED_FACE('',(#1387),#8231,.F.);
#8625=ADVANCED_FACE('',(#1388),#8232,.T.);
#8626=ADVANCED_FACE('',(#1389),#966,.T.);
#8627=ADVANCED_FACE('',(#1390),#967,.T.);
#8628=ADVANCED_FACE('',(#1391),#968,.T.);
#8629=ADVANCED_FACE('',(#1392),#969,.T.);
#8630=ADVANCED_FACE('',(#1393),#970,.T.);
#8631=ADVANCED_FACE('',(#1394),#971,.T.);
#8632=ADVANCED_FACE('',(#1395),#972,.F.);
#8633=ADVANCED_FACE('',(#1396),#973,.T.);
#8634=ADVANCED_FACE('',(#1397),#974,.T.);
#8635=ADVANCED_FACE('',(#1398),#975,.T.);
#8636=ADVANCED_FACE('',(#1399),#976,.T.);
#8637=ADVANCED_FACE('',(#1400),#977,.T.);
#8638=ADVANCED_FACE('',(#1401),#978,.F.);
#8639=ADVANCED_FACE('',(#1402),#979,.F.);
#8640=ADVANCED_FACE('',(#1403),#980,.F.);
#8641=ADVANCED_FACE('',(#1404),#981,.F.);
#8642=ADVANCED_FACE('',(#1405),#982,.F.);
#8643=ADVANCED_FACE('',(#1406),#983,.F.);
#8644=ADVANCED_FACE('',(#1407),#984,.F.);
#8645=ADVANCED_FACE('',(#1408),#985,.F.);
#8646=ADVANCED_FACE('',(#1409),#986,.F.);
#8647=ADVANCED_FACE('',(#1410),#987,.F.);
#8648=ADVANCED_FACE('',(#1411),#988,.T.);
#8649=ADVANCED_FACE('',(#1412),#195,.T.);
#8650=ADVANCED_FACE('',(#1413),#8233,.T.);
#8651=ADVANCED_FACE('',(#1414),#196,.T.);
#8652=ADVANCED_FACE('',(#1415,#842),#989,.T.);
#8653=ADVANCED_FACE('',(#1416),#197,.T.);
#8654=ADVANCED_FACE('',(#1417),#8234,.T.);
#8655=ADVANCED_FACE('',(#1418),#990,.F.);
#8656=ADVANCED_FACE('',(#1419),#991,.F.);
#8657=ADVANCED_FACE('',(#1420),#992,.F.);
#8658=ADVANCED_FACE('',(#1421),#993,.F.);
#8659=ADVANCED_FACE('',(#1422),#994,.F.);
#8660=ADVANCED_FACE('',(#1423),#995,.F.);
#8661=ADVANCED_FACE('',(#1424),#996,.F.);
#8662=ADVANCED_FACE('',(#1425),#997,.F.);
#8663=ADVANCED_FACE('',(#1426,#843),#998,.T.);
#8664=ADVANCED_FACE('',(#1427),#8235,.T.);
#8665=ADVANCED_FACE('',(#1428),#999,.F.);
#8666=ADVANCED_FACE('',(#1429),#1000,.T.);
#8667=ADVANCED_FACE('',(#1430),#198,.T.);
#8668=ADVANCED_FACE('',(#1431),#8236,.T.);
#8669=ADVANCED_FACE('',(#1432),#199,.T.);
#8670=ADVANCED_FACE('',(#1433,#844),#1001,.T.);
#8671=ADVANCED_FACE('',(#1434),#200,.T.);
#8672=ADVANCED_FACE('',(#1435),#8237,.T.);
#8673=ADVANCED_FACE('',(#1436),#8238,.F.);
#8674=ADVANCED_FACE('',(#1437),#8239,.T.);
#8675=ADVANCED_FACE('',(#1438,#845),#1002,.T.);
#8676=ADVANCED_FACE('',(#1439,#846),#1003,.F.);
#8677=ADVANCED_FACE('',(#1440),#201,.T.);
#8678=ADVANCED_FACE('',(#1441),#202,.T.);
#8679=ADVANCED_FACE('',(#1442),#1004,.T.);
#8680=ADVANCED_FACE('',(#1443),#1005,.T.);
#8681=ADVANCED_FACE('',(#1444),#1006,.T.);
#8682=ADVANCED_FACE('',(#1445),#8240,.F.);
#8683=ADVANCED_FACE('',(#1446),#1007,.T.);
#8684=ADVANCED_FACE('',(#1447),#1008,.T.);
#8685=ADVANCED_FACE('',(#1448),#1009,.T.);
#8686=ADVANCED_FACE('',(#1449,#847),#1010,.T.);
#8687=ADVANCED_FACE('',(#1450,#848),#1011,.F.);
#8688=ADVANCED_FACE('',(#1451),#8241,.F.);
#8689=ADVANCED_FACE('',(#1452),#8242,.F.);
#8690=ADVANCED_FACE('',(#1453),#8243,.F.);
#8691=ADVANCED_FACE('',(#1454),#8244,.F.);
#8692=ADVANCED_FACE('',(#1455),#8245,.F.);
#8693=ADVANCED_FACE('',(#1456),#8246,.F.);
#8694=ADVANCED_FACE('',(#1457),#8247,.F.);
#8695=ADVANCED_FACE('',(#1458),#8248,.F.);
#8696=ADVANCED_FACE('',(#1459),#8249,.F.);
#8697=ADVANCED_FACE('',(#1460),#209,.F.);
#8698=ADVANCED_FACE('',(#1461),#210,.F.);
#8699=ADVANCED_FACE('',(#1462,#849),#1012,.T.);
#8700=ADVANCED_FACE('',(#1463),#8250,.F.);
#8701=ADVANCED_FACE('',(#1464),#1013,.T.);
#8702=ADVANCED_FACE('',(#1465),#1014,.T.);
#8703=ADVANCED_FACE('',(#1466),#1015,.T.);
#8704=ADVANCED_FACE('',(#1467),#1016,.T.);
#8705=ADVANCED_FACE('',(#1468),#1017,.T.);
#8706=ADVANCED_FACE('',(#1469),#1018,.T.);
#8707=ADVANCED_FACE('',(#1470,#850),#1019,.F.);
#8708=ADVANCED_FACE('',(#1471),#8251,.F.);
#8709=ADVANCED_FACE('',(#1472),#8252,.F.);
#8710=ADVANCED_FACE('',(#1473),#8253,.F.);
#8711=ADVANCED_FACE('',(#1474),#8254,.F.);
#8712=ADVANCED_FACE('',(#1475),#8255,.F.);
#8713=ADVANCED_FACE('',(#1476),#8256,.F.);
#8714=ADVANCED_FACE('',(#1477),#8257,.F.);
#8715=ADVANCED_FACE('',(#1478),#8258,.F.);
#8716=ADVANCED_FACE('',(#1479),#8259,.F.);
#8717=ADVANCED_FACE('',(#1480),#211,.F.);
#8718=ADVANCED_FACE('',(#1481),#212,.F.);
#8719=ADVANCED_FACE('',(#1482,#851),#1020,.T.);
#8720=ADVANCED_FACE('',(#1483),#8260,.F.);
#8721=ADVANCED_FACE('',(#1484),#1021,.T.);
#8722=ADVANCED_FACE('',(#1485),#1022,.T.);
#8723=ADVANCED_FACE('',(#1486),#1023,.T.);
#8724=ADVANCED_FACE('',(#1487),#1024,.T.);
#8725=ADVANCED_FACE('',(#1488),#1025,.T.);
#8726=ADVANCED_FACE('',(#1489),#1026,.T.);
#8727=ADVANCED_FACE('',(#1490,#852),#1027,.F.);
#8728=ADVANCED_FACE('',(#1491),#8261,.F.);
#8729=ADVANCED_FACE('',(#1492),#8262,.F.);
#8730=ADVANCED_FACE('',(#1493),#8263,.F.);
#8731=ADVANCED_FACE('',(#1494),#8264,.F.);
#8732=ADVANCED_FACE('',(#1495),#8265,.F.);
#8733=ADVANCED_FACE('',(#1496),#8266,.F.);
#8734=ADVANCED_FACE('',(#1497),#8267,.F.);
#8735=ADVANCED_FACE('',(#1498),#8268,.F.);
#8736=ADVANCED_FACE('',(#1499),#8269,.F.);
#8737=ADVANCED_FACE('',(#1500),#213,.F.);
#8738=ADVANCED_FACE('',(#1501),#214,.F.);
#8739=ADVANCED_FACE('',(#1502,#853),#1028,.T.);
#8740=ADVANCED_FACE('',(#1503),#8270,.F.);
#8741=ADVANCED_FACE('',(#1504),#1029,.T.);
#8742=ADVANCED_FACE('',(#1505),#1030,.T.);
#8743=ADVANCED_FACE('',(#1506),#1031,.T.);
#8744=ADVANCED_FACE('',(#1507),#1032,.T.);
#8745=ADVANCED_FACE('',(#1508),#1033,.T.);
#8746=ADVANCED_FACE('',(#1509),#1034,.T.);
#8747=ADVANCED_FACE('',(#1510,#854),#1035,.F.);
#8748=ADVANCED_FACE('',(#1511),#8271,.F.);
#8749=ADVANCED_FACE('',(#1512),#8272,.F.);
#8750=ADVANCED_FACE('',(#1513),#8273,.F.);
#8751=ADVANCED_FACE('',(#1514),#8274,.F.);
#8752=ADVANCED_FACE('',(#1515),#8275,.F.);
#8753=ADVANCED_FACE('',(#1516),#8276,.F.);
#8754=ADVANCED_FACE('',(#1517),#8277,.F.);
#8755=ADVANCED_FACE('',(#1518),#8278,.F.);
#8756=ADVANCED_FACE('',(#1519),#8279,.F.);
#8757=ADVANCED_FACE('',(#1520),#215,.F.);
#8758=ADVANCED_FACE('',(#1521),#216,.F.);
#8759=ADVANCED_FACE('',(#1522,#855),#1036,.T.);
#8760=ADVANCED_FACE('',(#1523),#8280,.F.);
#8761=ADVANCED_FACE('',(#1524),#1037,.T.);
#8762=ADVANCED_FACE('',(#1525),#1038,.T.);
#8763=ADVANCED_FACE('',(#1526),#1039,.T.);
#8764=ADVANCED_FACE('',(#1527),#1040,.T.);
#8765=ADVANCED_FACE('',(#1528),#1041,.T.);
#8766=ADVANCED_FACE('',(#1529),#1042,.T.);
#8767=ADVANCED_FACE('',(#1530,#856),#1043,.F.);
#8768=CLOSED_SHELL('',(#8281,#8282,#8283,#8284,#8285,#8286,#8287,#8288,
#8289,#8290,#8291,#8292,#8293,#8294));
#8769=CLOSED_SHELL('',(#8295,#8296,#8297,#8298,#8299,#8300,#8301,#8302,
#8303,#8304,#8305,#8306,#8307,#8308,#8309,#8310,#8311,#8312,#8313,#8314,
#8315,#8316,#8317,#8318,#8319,#8320,#8321,#8322,#8323,#8324,#8325,#8326,
#8327,#8328,#8329,#8330,#8331,#8332,#8333,#8334,#8335,#8336,#8337,#8338,
#8339,#8340,#8341,#8342,#8343,#8344,#8345,#8346,#8347,#8348,#8349,#8350,
#8351,#8352,#8353,#8354,#8355,#8356,#8357,#8358,#8359,#8360,#8361,#8362,
#8363,#8364,#8365,#8366,#8367,#8368,#8369,#8370,#8371,#8372,#8373,#8374,
#8375,#8376,#8377,#8378,#8379,#8380,#8381,#8382,#8383,#8384,#8385,#8386,
#8387,#8388,#8389,#8390,#8391,#8392,#8393,#8394,#8395,#8396,#8397,#8398,
#8399,#8400,#8401,#8402,#8403,#8404,#8405,#8406,#8407,#8408,#8409,#8410,
#8411,#8412,#8413,#8414,#8415,#8416,#8417,#8418,#8419,#8420,#8421,#8422,
#8423,#8424,#8425,#8426,#8427,#8428,#8429,#8430,#8431,#8432,#8433,#8434,
#8435,#8436,#8437,#8438,#8439,#8440,#8441,#8442,#8443,#8444,#8445,#8446,
#8447,#8448,#8449,#8450,#8451,#8452,#8453,#8454,#8455,#8456,#8457,#8458,
#8459,#8460,#8461,#8462,#8463,#8464,#8465,#8466,#8467,#8468,#8469,#8470,
#8471,#8472,#8473,#8474,#8475,#8476,#8477,#8478,#8479,#8480,#8481,#8482,
#8483,#8484,#8485,#8486,#8487,#8488,#8489,#8490,#8491,#8492,#8493,#8494,
#8495,#8496));
#8770=CLOSED_SHELL('',(#8497,#8498,#8499));
#8771=CLOSED_SHELL('',(#8500,#8501,#8502));
#8772=CLOSED_SHELL('',(#8503,#8504,#8505,#8506,#8507,#8508,#8509,#8510,
#8511,#8512,#8513,#8514,#8515,#8516,#8517,#8518));
#8773=CLOSED_SHELL('',(#8519,#8520,#8521,#8522,#8523,#8524,#8525));
#8774=CLOSED_SHELL('',(#8526,#8527,#8528,#8529,#8530,#8531,#8532));
#8775=CLOSED_SHELL('',(#8533,#8534,#8535,#8536,#8537,#8538));
#8776=CLOSED_SHELL('',(#8539,#8540,#8541,#8542,#8543,#8544,#8545));
#8777=CLOSED_SHELL('',(#8546,#8547,#8548,#8549,#8550,#8551,#8552));
#8778=CLOSED_SHELL('',(#8553,#8554,#8555,#8556,#8557,#8558));
#8779=CLOSED_SHELL('',(#8559,#8560,#8561,#8562,#8563,#8564));
#8780=CLOSED_SHELL('',(#8565,#8566,#8567,#8568,#8569,#8570,#8571,#8572,
#8573,#8574,#8575,#8576,#8577,#8578,#8579,#8580));
#8781=CLOSED_SHELL('',(#8581,#8582,#8583,#8584,#8585,#8586,#8587));
#8782=CLOSED_SHELL('',(#8588,#8589,#8590,#8591,#8592,#8593,#8594));
#8783=CLOSED_SHELL('',(#8595,#8596,#8597,#8598,#8599,#8600));
#8784=CLOSED_SHELL('',(#8601,#8602,#8603,#8604,#8605,#8606,#8607));
#8785=CLOSED_SHELL('',(#8608,#8609,#8610,#8611,#8612,#8613,#8614));
#8786=CLOSED_SHELL('',(#8615,#8616,#8617,#8618,#8619,#8620));
#8787=CLOSED_SHELL('',(#8621,#8622,#8623,#8624,#8625,#8626));
#8788=CLOSED_SHELL('',(#8627,#8628,#8629,#8630,#8631,#8632));
#8789=CLOSED_SHELL('',(#8633,#8634,#8635,#8636,#8637,#8638));
#8790=CLOSED_SHELL('',(#8639,#8640,#8641,#8642,#8643,#8644,#8645,#8646));
#8791=CLOSED_SHELL('',(#8647,#8648,#8649,#8650,#8651,#8652,#8653,#8654));
#8792=CLOSED_SHELL('',(#8655,#8656,#8657,#8658,#8659,#8660,#8661,#8662));
#8793=CLOSED_SHELL('',(#8663,#8664,#8665,#8666,#8667,#8668,#8669,#8670,
#8671,#8672));
#8794=CLOSED_SHELL('',(#8673,#8674,#8675,#8676));
#8795=CLOSED_SHELL('',(#8677,#8678,#8679,#8680,#8681,#8682,#8683,#8684,
#8685,#8686,#8687));
#8796=CLOSED_SHELL('',(#8688,#8689,#8690,#8691,#8692,#8693,#8694,#8695,
#8696,#8697,#8698,#8699,#8700,#8701,#8702,#8703,#8704,#8705,#8706,#8707));
#8797=CLOSED_SHELL('',(#8708,#8709,#8710,#8711,#8712,#8713,#8714,#8715,
#8716,#8717,#8718,#8719,#8720,#8721,#8722,#8723,#8724,#8725,#8726,#8727));
#8798=CLOSED_SHELL('',(#8728,#8729,#8730,#8731,#8732,#8733,#8734,#8735,
#8736,#8737,#8738,#8739,#8740,#8741,#8742,#8743,#8744,#8745,#8746,#8747));
#8799=CLOSED_SHELL('',(#8748,#8749,#8750,#8751,#8752,#8753,#8754,#8755,
#8756,#8757,#8758,#8759,#8760,#8761,#8762,#8763,#8764,#8765,#8766,#8767));
#8800=DERIVED_UNIT_ELEMENT(#8844,1.);
#8801=DERIVED_UNIT_ELEMENT(#34435,-3.);
#8802=DERIVED_UNIT_ELEMENT(#8844,1.);
#8803=DERIVED_UNIT_ELEMENT(#34435,-3.);
#8804=DERIVED_UNIT_ELEMENT(#8844,1.);
#8805=DERIVED_UNIT_ELEMENT(#34435,-3.);
#8806=DERIVED_UNIT_ELEMENT(#8844,1.);
#8807=DERIVED_UNIT_ELEMENT(#34435,-3.);
#8808=DERIVED_UNIT_ELEMENT(#8844,1.);
#8809=DERIVED_UNIT_ELEMENT(#34435,-3.);
#8810=DERIVED_UNIT_ELEMENT(#8844,1.);
#8811=DERIVED_UNIT_ELEMENT(#34435,-3.);
#8812=DERIVED_UNIT_ELEMENT(#8844,1.);
#8813=DERIVED_UNIT_ELEMENT(#34435,-3.);
#8814=DERIVED_UNIT_ELEMENT(#8844,1.);
#8815=DERIVED_UNIT_ELEMENT(#34435,-3.);
#8816=DERIVED_UNIT_ELEMENT(#8844,1.);
#8817=DERIVED_UNIT_ELEMENT(#34435,-3.);
#8818=DERIVED_UNIT_ELEMENT(#8844,1.);
#8819=DERIVED_UNIT_ELEMENT(#34435,-3.);
#8820=DERIVED_UNIT_ELEMENT(#8844,1.);
#8821=DERIVED_UNIT_ELEMENT(#34435,-3.);
#8822=DERIVED_UNIT_ELEMENT(#8844,1.);
#8823=DERIVED_UNIT_ELEMENT(#34435,-3.);
#8824=DERIVED_UNIT_ELEMENT(#8844,1.);
#8825=DERIVED_UNIT_ELEMENT(#34435,-3.);
#8826=DERIVED_UNIT_ELEMENT(#8844,1.);
#8827=DERIVED_UNIT_ELEMENT(#34435,-3.);
#8828=DERIVED_UNIT_ELEMENT(#8844,1.);
#8829=DERIVED_UNIT_ELEMENT(#34435,-3.);
#8830=DERIVED_UNIT_ELEMENT(#8844,1.);
#8831=DERIVED_UNIT_ELEMENT(#34435,-3.);
#8832=DERIVED_UNIT_ELEMENT(#8844,1.);
#8833=DERIVED_UNIT_ELEMENT(#34435,-3.);
#8834=DERIVED_UNIT_ELEMENT(#8844,1.);
#8835=DERIVED_UNIT_ELEMENT(#34435,-3.);
#8836=DERIVED_UNIT_ELEMENT(#8844,1.);
#8837=DERIVED_UNIT_ELEMENT(#34435,-3.);
#8838=DERIVED_UNIT_ELEMENT(#8844,1.);
#8839=DERIVED_UNIT_ELEMENT(#34435,-3.);
#8840=DERIVED_UNIT_ELEMENT(#8844,1.);
#8841=DERIVED_UNIT_ELEMENT(#34435,-3.);
#8842=DERIVED_UNIT_ELEMENT(#8844,1.);
#8843=DERIVED_UNIT_ELEMENT(#34435,-3.);
#8844=(
MASS_UNIT()
NAMED_UNIT(*)
SI_UNIT(.KILO.,.GRAM.)
);
#8845=DERIVED_UNIT((#8800,#8801));
#8846=DERIVED_UNIT((#8802,#8803));
#8847=DERIVED_UNIT((#8804,#8805));
#8848=DERIVED_UNIT((#8806,#8807));
#8849=DERIVED_UNIT((#8808,#8809));
#8850=DERIVED_UNIT((#8810,#8811));
#8851=DERIVED_UNIT((#8812,#8813));
#8852=DERIVED_UNIT((#8814,#8815));
#8853=DERIVED_UNIT((#8816,#8817));
#8854=DERIVED_UNIT((#8818,#8819));
#8855=DERIVED_UNIT((#8820,#8821));
#8856=DERIVED_UNIT((#8822,#8823));
#8857=DERIVED_UNIT((#8824,#8825));
#8858=DERIVED_UNIT((#8826,#8827));
#8859=DERIVED_UNIT((#8828,#8829));
#8860=DERIVED_UNIT((#8830,#8831));
#8861=DERIVED_UNIT((#8832,#8833));
#8862=DERIVED_UNIT((#8834,#8835));
#8863=DERIVED_UNIT((#8836,#8837));
#8864=DERIVED_UNIT((#8838,#8839));
#8865=DERIVED_UNIT((#8840,#8841));
#8866=DERIVED_UNIT((#8842,#8843));
#8867=MEASURE_REPRESENTATION_ITEM('density measure',
POSITIVE_RATIO_MEASURE(7850.),#8845);
#8868=MEASURE_REPRESENTATION_ITEM('density measure',
POSITIVE_RATIO_MEASURE(7850.),#8846);
#8869=MEASURE_REPRESENTATION_ITEM('density measure',
POSITIVE_RATIO_MEASURE(7850.),#8847);
#8870=MEASURE_REPRESENTATION_ITEM('density measure',
POSITIVE_RATIO_MEASURE(7850.),#8848);
#8871=MEASURE_REPRESENTATION_ITEM('density measure',
POSITIVE_RATIO_MEASURE(7850.),#8849);
#8872=MEASURE_REPRESENTATION_ITEM('density measure',
POSITIVE_RATIO_MEASURE(7850.),#8850);
#8873=MEASURE_REPRESENTATION_ITEM('density measure',
POSITIVE_RATIO_MEASURE(7850.),#8851);
#8874=MEASURE_REPRESENTATION_ITEM('density measure',
POSITIVE_RATIO_MEASURE(7850.),#8852);
#8875=MEASURE_REPRESENTATION_ITEM('density measure',
POSITIVE_RATIO_MEASURE(7850.),#8853);
#8876=MEASURE_REPRESENTATION_ITEM('density measure',
POSITIVE_RATIO_MEASURE(7850.),#8854);
#8877=MEASURE_REPRESENTATION_ITEM('density measure',
POSITIVE_RATIO_MEASURE(7850.),#8855);
#8878=MEASURE_REPRESENTATION_ITEM('density measure',
POSITIVE_RATIO_MEASURE(7850.),#8856);
#8879=MEASURE_REPRESENTATION_ITEM('density measure',
POSITIVE_RATIO_MEASURE(7850.),#8857);
#8880=MEASURE_REPRESENTATION_ITEM('density measure',
POSITIVE_RATIO_MEASURE(7850.),#8858);
#8881=MEASURE_REPRESENTATION_ITEM('density measure',
POSITIVE_RATIO_MEASURE(7850.),#8859);
#8882=MEASURE_REPRESENTATION_ITEM('density measure',
POSITIVE_RATIO_MEASURE(7850.),#8860);
#8883=MEASURE_REPRESENTATION_ITEM('density measure',
POSITIVE_RATIO_MEASURE(7850.),#8861);
#8884=MEASURE_REPRESENTATION_ITEM('density measure',
POSITIVE_RATIO_MEASURE(7850.),#8862);
#8885=MEASURE_REPRESENTATION_ITEM('density measure',
POSITIVE_RATIO_MEASURE(7850.),#8863);
#8886=MEASURE_REPRESENTATION_ITEM('density measure',
POSITIVE_RATIO_MEASURE(7850.),#8864);
#8887=MEASURE_REPRESENTATION_ITEM('density measure',
POSITIVE_RATIO_MEASURE(7850.),#8865);
#8888=MEASURE_REPRESENTATION_ITEM('density measure',
POSITIVE_RATIO_MEASURE(7850.),#8866);
#8889=PROPERTY_DEFINITION_REPRESENTATION(#8999,#8933);
#8890=PROPERTY_DEFINITION_REPRESENTATION(#9000,#8934);
#8891=PROPERTY_DEFINITION_REPRESENTATION(#9001,#8935);
#8892=PROPERTY_DEFINITION_REPRESENTATION(#9002,#8936);
#8893=PROPERTY_DEFINITION_REPRESENTATION(#9003,#8937);
#8894=PROPERTY_DEFINITION_REPRESENTATION(#9004,#8938);
#8895=PROPERTY_DEFINITION_REPRESENTATION(#9005,#8939);
#8896=PROPERTY_DEFINITION_REPRESENTATION(#9006,#8940);
#8897=PROPERTY_DEFINITION_REPRESENTATION(#9007,#8941);
#8898=PROPERTY_DEFINITION_REPRESENTATION(#9008,#8942);
#8899=PROPERTY_DEFINITION_REPRESENTATION(#9009,#8943);
#8900=PROPERTY_DEFINITION_REPRESENTATION(#9010,#8944);
#8901=PROPERTY_DEFINITION_REPRESENTATION(#9011,#8945);
#8902=PROPERTY_DEFINITION_REPRESENTATION(#9012,#8946);
#8903=PROPERTY_DEFINITION_REPRESENTATION(#9013,#8947);
#8904=PROPERTY_DEFINITION_REPRESENTATION(#9014,#8948);
#8905=PROPERTY_DEFINITION_REPRESENTATION(#9015,#8949);
#8906=PROPERTY_DEFINITION_REPRESENTATION(#9016,#8950);
#8907=PROPERTY_DEFINITION_REPRESENTATION(#9017,#8951);
#8908=PROPERTY_DEFINITION_REPRESENTATION(#9018,#8952);
#8909=PROPERTY_DEFINITION_REPRESENTATION(#9019,#8953);
#8910=PROPERTY_DEFINITION_REPRESENTATION(#9020,#8954);
#8911=PROPERTY_DEFINITION_REPRESENTATION(#9021,#8955);
#8912=PROPERTY_DEFINITION_REPRESENTATION(#9022,#8956);
#8913=PROPERTY_DEFINITION_REPRESENTATION(#9023,#8957);
#8914=PROPERTY_DEFINITION_REPRESENTATION(#9024,#8958);
#8915=PROPERTY_DEFINITION_REPRESENTATION(#9025,#8959);
#8916=PROPERTY_DEFINITION_REPRESENTATION(#9026,#8960);
#8917=PROPERTY_DEFINITION_REPRESENTATION(#9027,#8961);
#8918=PROPERTY_DEFINITION_REPRESENTATION(#9028,#8962);
#8919=PROPERTY_DEFINITION_REPRESENTATION(#9029,#8963);
#8920=PROPERTY_DEFINITION_REPRESENTATION(#9030,#8964);
#8921=PROPERTY_DEFINITION_REPRESENTATION(#9031,#8965);
#8922=PROPERTY_DEFINITION_REPRESENTATION(#9032,#8966);
#8923=PROPERTY_DEFINITION_REPRESENTATION(#9033,#8967);
#8924=PROPERTY_DEFINITION_REPRESENTATION(#9034,#8968);
#8925=PROPERTY_DEFINITION_REPRESENTATION(#9035,#8969);
#8926=PROPERTY_DEFINITION_REPRESENTATION(#9036,#8970);
#8927=PROPERTY_DEFINITION_REPRESENTATION(#9037,#8971);
#8928=PROPERTY_DEFINITION_REPRESENTATION(#9038,#8972);
#8929=PROPERTY_DEFINITION_REPRESENTATION(#9039,#8973);
#8930=PROPERTY_DEFINITION_REPRESENTATION(#9040,#8974);
#8931=PROPERTY_DEFINITION_REPRESENTATION(#9041,#8975);
#8932=PROPERTY_DEFINITION_REPRESENTATION(#9042,#8976);
#8933=REPRESENTATION('material name',(#8977),#34407);
#8934=REPRESENTATION('density',(#8867),#34407);
#8935=REPRESENTATION('material name',(#8978),#34408);
#8936=REPRESENTATION('density',(#8868),#34408);
#8937=REPRESENTATION('material name',(#8979),#34409);
#8938=REPRESENTATION('density',(#8869),#34409);
#8939=REPRESENTATION('material name',(#8980),#34410);
#8940=REPRESENTATION('density',(#8870),#34410);
#8941=REPRESENTATION('material name',(#8981),#34411);
#8942=REPRESENTATION('density',(#8871),#34411);
#8943=REPRESENTATION('material name',(#8982),#34412);
#8944=REPRESENTATION('density',(#8872),#34412);
#8945=REPRESENTATION('material name',(#8983),#34413);
#8946=REPRESENTATION('density',(#8873),#34413);
#8947=REPRESENTATION('material name',(#8984),#34414);
#8948=REPRESENTATION('density',(#8874),#34414);
#8949=REPRESENTATION('material name',(#8985),#34415);
#8950=REPRESENTATION('density',(#8875),#34415);
#8951=REPRESENTATION('material name',(#8986),#34416);
#8952=REPRESENTATION('density',(#8876),#34416);
#8953=REPRESENTATION('material name',(#8987),#34417);
#8954=REPRESENTATION('density',(#8877),#34417);
#8955=REPRESENTATION('material name',(#8988),#34418);
#8956=REPRESENTATION('density',(#8878),#34418);
#8957=REPRESENTATION('material name',(#8989),#34419);
#8958=REPRESENTATION('density',(#8879),#34419);
#8959=REPRESENTATION('material name',(#8990),#34420);
#8960=REPRESENTATION('density',(#8880),#34420);
#8961=REPRESENTATION('material name',(#8991),#34421);
#8962=REPRESENTATION('density',(#8881),#34421);
#8963=REPRESENTATION('material name',(#8992),#34422);
#8964=REPRESENTATION('density',(#8882),#34422);
#8965=REPRESENTATION('material name',(#8993),#34423);
#8966=REPRESENTATION('density',(#8883),#34423);
#8967=REPRESENTATION('material name',(#8994),#34424);
#8968=REPRESENTATION('density',(#8884),#34424);
#8969=REPRESENTATION('material name',(#8995),#34426);
#8970=REPRESENTATION('density',(#8885),#34426);
#8971=REPRESENTATION('material name',(#8996),#34428);
#8972=REPRESENTATION('density',(#8886),#34428);
#8973=REPRESENTATION('material name',(#8997),#34430);
#8974=REPRESENTATION('density',(#8887),#34430);
#8975=REPRESENTATION('material name',(#8998),#34432);
#8976=REPRESENTATION('density',(#8888),#34432);
#8977=DESCRIPTIVE_REPRESENTATION_ITEM('Steel','Steel');
#8978=DESCRIPTIVE_REPRESENTATION_ITEM('Steel','Steel');
#8979=DESCRIPTIVE_REPRESENTATION_ITEM('Steel','Steel');
#8980=DESCRIPTIVE_REPRESENTATION_ITEM('Steel','Steel');
#8981=DESCRIPTIVE_REPRESENTATION_ITEM('Steel','Steel');
#8982=DESCRIPTIVE_REPRESENTATION_ITEM('Steel','Steel');
#8983=DESCRIPTIVE_REPRESENTATION_ITEM('Steel','Steel');
#8984=DESCRIPTIVE_REPRESENTATION_ITEM('Steel','Steel');
#8985=DESCRIPTIVE_REPRESENTATION_ITEM('Steel','Steel');
#8986=DESCRIPTIVE_REPRESENTATION_ITEM('Steel','Steel');
#8987=DESCRIPTIVE_REPRESENTATION_ITEM('Steel','Steel');
#8988=DESCRIPTIVE_REPRESENTATION_ITEM('Steel','Steel');
#8989=DESCRIPTIVE_REPRESENTATION_ITEM('Steel','Steel');
#8990=DESCRIPTIVE_REPRESENTATION_ITEM('Steel','Steel');
#8991=DESCRIPTIVE_REPRESENTATION_ITEM('Steel','Steel');
#8992=DESCRIPTIVE_REPRESENTATION_ITEM('Steel','Steel');
#8993=DESCRIPTIVE_REPRESENTATION_ITEM('Steel','Steel');
#8994=DESCRIPTIVE_REPRESENTATION_ITEM('Steel','Steel');
#8995=DESCRIPTIVE_REPRESENTATION_ITEM('Steel','Steel');
#8996=DESCRIPTIVE_REPRESENTATION_ITEM('Steel','Steel');
#8997=DESCRIPTIVE_REPRESENTATION_ITEM('Steel','Steel');
#8998=DESCRIPTIVE_REPRESENTATION_ITEM('Steel','Steel');
#8999=PROPERTY_DEFINITION('material property','material name',#34568);
#9000=PROPERTY_DEFINITION('material property','density of part',#34568);
#9001=PROPERTY_DEFINITION('material property','material name',#34569);
#9002=PROPERTY_DEFINITION('material property','density of part',#34569);
#9003=PROPERTY_DEFINITION('material property','material name',#34570);
#9004=PROPERTY_DEFINITION('material property','density of part',#34570);
#9005=PROPERTY_DEFINITION('material property','material name',#34571);
#9006=PROPERTY_DEFINITION('material property','density of part',#34571);
#9007=PROPERTY_DEFINITION('material property','material name',#34572);
#9008=PROPERTY_DEFINITION('material property','density of part',#34572);
#9009=PROPERTY_DEFINITION('material property','material name',#34573);
#9010=PROPERTY_DEFINITION('material property','density of part',#34573);
#9011=PROPERTY_DEFINITION('material property','material name',#34574);
#9012=PROPERTY_DEFINITION('material property','density of part',#34574);
#9013=PROPERTY_DEFINITION('material property','material name',#34575);
#9014=PROPERTY_DEFINITION('material property','density of part',#34575);
#9015=PROPERTY_DEFINITION('material property','material name',#34576);
#9016=PROPERTY_DEFINITION('material property','density of part',#34576);
#9017=PROPERTY_DEFINITION('material property','material name',#34577);
#9018=PROPERTY_DEFINITION('material property','density of part',#34577);
#9019=PROPERTY_DEFINITION('material property','material name',#34578);
#9020=PROPERTY_DEFINITION('material property','density of part',#34578);
#9021=PROPERTY_DEFINITION('material property','material name',#34579);
#9022=PROPERTY_DEFINITION('material property','density of part',#34579);
#9023=PROPERTY_DEFINITION('material property','material name',#34580);
#9024=PROPERTY_DEFINITION('material property','density of part',#34580);
#9025=PROPERTY_DEFINITION('material property','material name',#34581);
#9026=PROPERTY_DEFINITION('material property','density of part',#34581);
#9027=PROPERTY_DEFINITION('material property','material name',#34582);
#9028=PROPERTY_DEFINITION('material property','density of part',#34582);
#9029=PROPERTY_DEFINITION('material property','material name',#34583);
#9030=PROPERTY_DEFINITION('material property','density of part',#34583);
#9031=PROPERTY_DEFINITION('material property','material name',#34584);
#9032=PROPERTY_DEFINITION('material property','density of part',#34584);
#9033=PROPERTY_DEFINITION('material property','material name',#34585);
#9034=PROPERTY_DEFINITION('material property','density of part',#34585);
#9035=PROPERTY_DEFINITION('material property','material name',#34587);
#9036=PROPERTY_DEFINITION('material property','density of part',#34587);
#9037=PROPERTY_DEFINITION('material property','material name',#34589);
#9038=PROPERTY_DEFINITION('material property','density of part',#34589);
#9039=PROPERTY_DEFINITION('material property','material name',#34591);
#9040=PROPERTY_DEFINITION('material property','density of part',#34591);
#9041=PROPERTY_DEFINITION('material property','material name',#34593);
#9042=PROPERTY_DEFINITION('material property','density of part',#34593);
#9043=AXIS2_PLACEMENT_3D('',#11706,#9725,#9726);
#9044=AXIS2_PLACEMENT_3D('',#11707,#9727,#9728);
#9045=AXIS2_PLACEMENT_3D('',#11708,#9729,#9730);
#9046=AXIS2_PLACEMENT_3D('',#11709,#9731,#9732);
#9047=AXIS2_PLACEMENT_3D('',#11711,#9733,#9734);
#9048=AXIS2_PLACEMENT_3D('',#11714,#9736,#9737);
#9049=AXIS2_PLACEMENT_3D('',#11715,#9738,#9739);
#9050=AXIS2_PLACEMENT_3D('',#11716,#9740,#9741);
#9051=AXIS2_PLACEMENT_3D('',#11718,#9742,#9743);
#9052=AXIS2_PLACEMENT_3D('',#11721,#9745,#9746);
#9053=AXIS2_PLACEMENT_3D('',#11722,#9747,#9748);
#9054=AXIS2_PLACEMENT_3D('',#11723,#9749,#9750);
#9055=AXIS2_PLACEMENT_3D('',#11725,#9751,#9752);
#9056=AXIS2_PLACEMENT_3D('',#11728,#9754,#9755);
#9057=AXIS2_PLACEMENT_3D('',#11729,#9756,#9757);
#9058=AXIS2_PLACEMENT_3D('',#11731,#9758,#9759);
#9059=AXIS2_PLACEMENT_3D('',#11734,#9761,#9762);
#9060=AXIS2_PLACEMENT_3D('',#11735,#9763,#9764);
#9061=AXIS2_PLACEMENT_3D('',#11737,#9765,#9766);
#9062=AXIS2_PLACEMENT_3D('',#11740,#9768,#9769);
#9063=AXIS2_PLACEMENT_3D('',#11741,#9770,#9771);
#9064=AXIS2_PLACEMENT_3D('',#11743,#9772,#9773);
#9065=AXIS2_PLACEMENT_3D('',#11746,#9775,#9776);
#9066=AXIS2_PLACEMENT_3D('',#11747,#9777,#9778);
#9067=AXIS2_PLACEMENT_3D('',#11756,#9783,#9784);
#9068=AXIS2_PLACEMENT_3D('',#11762,#9788,#9789);
#9069=AXIS2_PLACEMENT_3D('',#11768,#9793,#9794);
#9070=AXIS2_PLACEMENT_3D('',#11771,#9797,#9798);
#9071=AXIS2_PLACEMENT_3D('',#11772,#9799,#9800);
#9072=AXIS2_PLACEMENT_3D('',#11773,#9801,#9802);
#9073=AXIS2_PLACEMENT_3D('',#11774,#9803,#9804);
#9074=AXIS2_PLACEMENT_3D('',#11790,#9806,#9807);
#9075=AXIS2_PLACEMENT_3D('',#11801,#9808,#9809);
#9076=AXIS2_PLACEMENT_3D('',#11855,#9811,#9812);
#9077=AXIS2_PLACEMENT_3D('',#11915,#9814,#9815);
#9078=AXIS2_PLACEMENT_3D('',#11972,#9817,#9818);
#9079=AXIS2_PLACEMENT_3D('',#12032,#9820,#9821);
#9080=AXIS2_PLACEMENT_3D('',#12092,#9823,#9824);
#9081=AXIS2_PLACEMENT_3D('',#12149,#9826,#9827);
#9082=AXIS2_PLACEMENT_3D('',#12209,#9829,#9830);
#9083=AXIS2_PLACEMENT_3D('',#12269,#9832,#9833);
#9084=AXIS2_PLACEMENT_3D('',#12329,#9835,#9836);
#9085=AXIS2_PLACEMENT_3D('',#12389,#9838,#9839);
#9086=AXIS2_PLACEMENT_3D('',#12449,#9841,#9842);
#9087=AXIS2_PLACEMENT_3D('',#12506,#9844,#9845);
#9088=AXIS2_PLACEMENT_3D('',#12566,#9847,#9848);
#9089=AXIS2_PLACEMENT_3D('',#12626,#9850,#9851);
#9090=AXIS2_PLACEMENT_3D('',#12686,#9853,#9854);
#9091=AXIS2_PLACEMENT_3D('',#12746,#9856,#9857);
#9092=AXIS2_PLACEMENT_3D('',#12803,#9859,#9860);
#9093=AXIS2_PLACEMENT_3D('',#12863,#9862,#9863);
#9094=AXIS2_PLACEMENT_3D('',#12923,#9865,#9866);
#9095=AXIS2_PLACEMENT_3D('',#12983,#9868,#9869);
#9096=AXIS2_PLACEMENT_3D('',#13043,#9871,#9872);
#9097=AXIS2_PLACEMENT_3D('',#13097,#9874,#9875);
#9098=AXIS2_PLACEMENT_3D('',#13157,#9877,#9878);
#9099=AXIS2_PLACEMENT_3D('',#13217,#9880,#9881);
#9100=AXIS2_PLACEMENT_3D('',#13277,#9883,#9884);
#9101=AXIS2_PLACEMENT_3D('',#13334,#9886,#9887);
#9102=AXIS2_PLACEMENT_3D('',#13394,#9889,#9890);
#9103=AXIS2_PLACEMENT_3D('',#13454,#9892,#9893);
#9104=AXIS2_PLACEMENT_3D('',#13514,#9895,#9896);
#9105=AXIS2_PLACEMENT_3D('',#13574,#9898,#9899);
#9106=AXIS2_PLACEMENT_3D('',#13634,#9901,#9902);
#9107=AXIS2_PLACEMENT_3D('',#13694,#9904,#9905);
#9108=AXIS2_PLACEMENT_3D('',#13754,#9907,#9908);
#9109=AXIS2_PLACEMENT_3D('',#13814,#9910,#9911);
#9110=AXIS2_PLACEMENT_3D('',#13874,#9913,#9914);
#9111=AXIS2_PLACEMENT_3D('',#13931,#9916,#9917);
#9112=AXIS2_PLACEMENT_3D('',#13991,#9919,#9920);
#9113=AXIS2_PLACEMENT_3D('',#14051,#9922,#9923);
#9114=AXIS2_PLACEMENT_3D('',#14111,#9925,#9926);
#9115=AXIS2_PLACEMENT_3D('',#14171,#9928,#9929);
#9116=AXIS2_PLACEMENT_3D('',#14228,#9931,#9932);
#9117=AXIS2_PLACEMENT_3D('',#14288,#9934,#9935);
#9118=AXIS2_PLACEMENT_3D('',#14348,#9937,#9938);
#9119=AXIS2_PLACEMENT_3D('',#14408,#9940,#9941);
#9120=AXIS2_PLACEMENT_3D('',#14468,#9943,#9944);
#9121=AXIS2_PLACEMENT_3D('',#14528,#9946,#9947);
#9122=AXIS2_PLACEMENT_3D('',#14588,#9949,#9950);
#9123=AXIS2_PLACEMENT_3D('',#14645,#9952,#9953);
#9124=AXIS2_PLACEMENT_3D('',#14705,#9955,#9956);
#9125=AXIS2_PLACEMENT_3D('',#14765,#9958,#9959);
#9126=AXIS2_PLACEMENT_3D('',#14825,#9961,#9962);
#9127=AXIS2_PLACEMENT_3D('',#14885,#9964,#9965);
#9128=AXIS2_PLACEMENT_3D('',#14942,#9967,#9968);
#9129=AXIS2_PLACEMENT_3D('',#15002,#9970,#9971);
#9130=AXIS2_PLACEMENT_3D('',#15062,#9973,#9974);
#9131=AXIS2_PLACEMENT_3D('',#15122,#9976,#9977);
#9132=AXIS2_PLACEMENT_3D('',#15182,#9979,#9980);
#9133=AXIS2_PLACEMENT_3D('',#15242,#9982,#9983);
#9134=AXIS2_PLACEMENT_3D('',#15299,#9985,#9986);
#9135=AXIS2_PLACEMENT_3D('',#15359,#9988,#9989);
#9136=AXIS2_PLACEMENT_3D('',#15419,#9991,#9992);
#9137=AXIS2_PLACEMENT_3D('',#15479,#9994,#9995);
#9138=AXIS2_PLACEMENT_3D('',#15539,#9997,#9998);
#9139=AXIS2_PLACEMENT_3D('',#15596,#10000,#10001);
#9140=AXIS2_PLACEMENT_3D('',#15656,#10003,#10004);
#9141=AXIS2_PLACEMENT_3D('',#15716,#10006,#10007);
#9142=AXIS2_PLACEMENT_3D('',#15776,#10009,#10010);
#9143=AXIS2_PLACEMENT_3D('',#15833,#10012,#10013);
#9144=AXIS2_PLACEMENT_3D('',#15893,#10015,#10016);
#9145=AXIS2_PLACEMENT_3D('',#15953,#10018,#10019);
#9146=AXIS2_PLACEMENT_3D('',#16013,#10021,#10022);
#9147=AXIS2_PLACEMENT_3D('',#16073,#10024,#10025);
#9148=AXIS2_PLACEMENT_3D('',#16133,#10027,#10028);
#9149=AXIS2_PLACEMENT_3D('',#16193,#10030,#10031);
#9150=AXIS2_PLACEMENT_3D('',#16253,#10033,#10034);
#9151=AXIS2_PLACEMENT_3D('',#16313,#10036,#10037);
#9152=AXIS2_PLACEMENT_3D('',#16373,#10039,#10040);
#9153=AXIS2_PLACEMENT_3D('',#16430,#10042,#10043);
#9154=AXIS2_PLACEMENT_3D('',#16490,#10045,#10046);
#9155=AXIS2_PLACEMENT_3D('',#16550,#10048,#10049);
#9156=AXIS2_PLACEMENT_3D('',#16610,#10051,#10052);
#9157=AXIS2_PLACEMENT_3D('',#16670,#10054,#10055);
#9158=AXIS2_PLACEMENT_3D('',#16727,#10057,#10058);
#9159=AXIS2_PLACEMENT_3D('',#16787,#10060,#10061);
#9160=AXIS2_PLACEMENT_3D('',#16847,#10063,#10064);
#9161=AXIS2_PLACEMENT_3D('',#16907,#10066,#10067);
#9162=AXIS2_PLACEMENT_3D('',#16967,#10069,#10070);
#9163=AXIS2_PLACEMENT_3D('',#17027,#10072,#10073);
#9164=AXIS2_PLACEMENT_3D('',#17087,#10075,#10076);
#9165=AXIS2_PLACEMENT_3D('',#17147,#10078,#10079);
#9166=AXIS2_PLACEMENT_3D('',#17207,#10081,#10082);
#9167=AXIS2_PLACEMENT_3D('',#17267,#10084,#10085);
#9168=AXIS2_PLACEMENT_3D('',#17324,#10087,#10088);
#9169=AXIS2_PLACEMENT_3D('',#17340,#10090,#10091);
#9170=AXIS2_PLACEMENT_3D('',#17346,#10092,#10093);
#9171=AXIS2_PLACEMENT_3D('',#17406,#10095,#10096);
#9172=AXIS2_PLACEMENT_3D('',#17463,#10098,#10099);
#9173=AXIS2_PLACEMENT_3D('',#17523,#10101,#10102);
#9174=AXIS2_PLACEMENT_3D('',#17583,#10104,#10105);
#9175=AXIS2_PLACEMENT_3D('',#17626,#10107,#10108);
#9176=AXIS2_PLACEMENT_3D('',#17669,#10110,#10111);
#9177=AXIS2_PLACEMENT_3D('',#17711,#10113,#10114);
#9178=AXIS2_PLACEMENT_3D('',#17771,#10116,#10117);
#9179=AXIS2_PLACEMENT_3D('',#17831,#10119,#10120);
#9180=AXIS2_PLACEMENT_3D('',#17891,#10122,#10123);
#9181=AXIS2_PLACEMENT_3D('',#17951,#10125,#10126);
#9182=AXIS2_PLACEMENT_3D('',#17994,#10128,#10129);
#9183=AXIS2_PLACEMENT_3D('',#18054,#10131,#10132);
#9184=AXIS2_PLACEMENT_3D('',#18114,#10134,#10135);
#9185=AXIS2_PLACEMENT_3D('',#18174,#10137,#10138);
#9186=AXIS2_PLACEMENT_3D('',#18217,#10140,#10141);
#9187=AXIS2_PLACEMENT_3D('',#18277,#10143,#10144);
#9188=AXIS2_PLACEMENT_3D('',#18337,#10146,#10147);
#9189=AXIS2_PLACEMENT_3D('',#18397,#10149,#10150);
#9190=AXIS2_PLACEMENT_3D('',#18457,#10152,#10153);
#9191=AXIS2_PLACEMENT_3D('',#18500,#10155,#10156);
#9192=AXIS2_PLACEMENT_3D('',#18560,#10158,#10159);
#9193=AXIS2_PLACEMENT_3D('',#18620,#10161,#10162);
#9194=AXIS2_PLACEMENT_3D('',#18680,#10164,#10165);
#9195=AXIS2_PLACEMENT_3D('',#18740,#10167,#10168);
#9196=AXIS2_PLACEMENT_3D('',#18765,#10170,#10171);
#9197=AXIS2_PLACEMENT_3D('',#18809,#10173,#10174);
#9198=AXIS2_PLACEMENT_3D('',#18869,#10176,#10177);
#9199=AXIS2_PLACEMENT_3D('',#18929,#10179,#10180);
#9200=AXIS2_PLACEMENT_3D('',#18972,#10182,#10183);
#9201=AXIS2_PLACEMENT_3D('',#19015,#10185,#10186);
#9202=AXIS2_PLACEMENT_3D('',#19058,#10188,#10189);
#9203=AXIS2_PLACEMENT_3D('',#19118,#10191,#10192);
#9204=AXIS2_PLACEMENT_3D('',#19178,#10194,#10195);
#9205=AXIS2_PLACEMENT_3D('',#19221,#10197,#10198);
#9206=AXIS2_PLACEMENT_3D('',#19264,#10200,#10201);
#9207=AXIS2_PLACEMENT_3D('',#19324,#10203,#10204);
#9208=AXIS2_PLACEMENT_3D('',#19384,#10206,#10207);
#9209=AXIS2_PLACEMENT_3D('',#19444,#10209,#10210);
#9210=AXIS2_PLACEMENT_3D('',#19504,#10212,#10213);
#9211=AXIS2_PLACEMENT_3D('',#19547,#10215,#10216);
#9212=AXIS2_PLACEMENT_3D('',#19590,#10218,#10219);
#9213=AXIS2_PLACEMENT_3D('',#19650,#10221,#10222);
#9214=AXIS2_PLACEMENT_3D('',#19710,#10224,#10225);
#9215=AXIS2_PLACEMENT_3D('',#19753,#10227,#10228);
#9216=AXIS2_PLACEMENT_3D('',#19796,#10230,#10231);
#9217=AXIS2_PLACEMENT_3D('',#19839,#10233,#10234);
#9218=AXIS2_PLACEMENT_3D('',#19899,#10236,#10237);
#9219=AXIS2_PLACEMENT_3D('',#19942,#10239,#10240);
#9220=AXIS2_PLACEMENT_3D('',#20002,#10242,#10243);
#9221=AXIS2_PLACEMENT_3D('',#20062,#10245,#10246);
#9222=AXIS2_PLACEMENT_3D('',#20122,#10248,#10249);
#9223=AXIS2_PLACEMENT_3D('',#20182,#10251,#10252);
#9224=AXIS2_PLACEMENT_3D('',#20225,#10254,#10255);
#9225=AXIS2_PLACEMENT_3D('',#20285,#10257,#10258);
#9226=AXIS2_PLACEMENT_3D('',#20345,#10260,#10261);
#9227=AXIS2_PLACEMENT_3D('',#20405,#10263,#10264);
#9228=AXIS2_PLACEMENT_3D('',#20448,#10266,#10267);
#9229=AXIS2_PLACEMENT_3D('',#20508,#10269,#10270);
#9230=AXIS2_PLACEMENT_3D('',#20568,#10272,#10273);
#9231=AXIS2_PLACEMENT_3D('',#20628,#10275,#10276);
#9232=AXIS2_PLACEMENT_3D('',#20688,#10278,#10279);
#9233=AXIS2_PLACEMENT_3D('',#20730,#10281,#10282);
#9234=AXIS2_PLACEMENT_3D('',#20790,#10284,#10285);
#9235=AXIS2_PLACEMENT_3D('',#20833,#10287,#10288);
#9236=AXIS2_PLACEMENT_3D('',#20893,#10290,#10291);
#9237=AXIS2_PLACEMENT_3D('',#20953,#10293,#10294);
#9238=AXIS2_PLACEMENT_3D('',#20996,#10296,#10297);
#9239=AXIS2_PLACEMENT_3D('',#21040,#10299,#10300);
#9240=AXIS2_PLACEMENT_3D('',#21100,#10302,#10303);
#9241=AXIS2_PLACEMENT_3D('',#21160,#10305,#10306);
#9242=AXIS2_PLACEMENT_3D('',#21203,#10308,#10309);
#9243=AXIS2_PLACEMENT_3D('',#21246,#10311,#10312);
#9244=AXIS2_PLACEMENT_3D('',#21306,#10314,#10315);
#9245=AXIS2_PLACEMENT_3D('',#21366,#10317,#10318);
#9246=AXIS2_PLACEMENT_3D('',#21426,#10320,#10321);
#9247=AXIS2_PLACEMENT_3D('',#21469,#10323,#10324);
#9248=AXIS2_PLACEMENT_3D('',#21512,#10326,#10327);
#9249=AXIS2_PLACEMENT_3D('',#21572,#10329,#10330);
#9250=AXIS2_PLACEMENT_3D('',#21632,#10332,#10333);
#9251=AXIS2_PLACEMENT_3D('',#21692,#10335,#10336);
#9252=AXIS2_PLACEMENT_3D('',#21752,#10338,#10339);
#9253=AXIS2_PLACEMENT_3D('',#21795,#10341,#10342);
#9254=AXIS2_PLACEMENT_3D('',#21822,#10344,#10345);
#9255=AXIS2_PLACEMENT_3D('',#21882,#10347,#10348);
#9256=AXIS2_PLACEMENT_3D('',#21925,#10350,#10351);
#9257=AXIS2_PLACEMENT_3D('',#21968,#10353,#10354);
#9258=AXIS2_PLACEMENT_3D('',#22011,#10356,#10357);
#9259=AXIS2_PLACEMENT_3D('',#22054,#10359,#10360);
#9260=AXIS2_PLACEMENT_3D('',#22114,#10362,#10363);
#9261=AXIS2_PLACEMENT_3D('',#22174,#10365,#10366);
#9262=AXIS2_PLACEMENT_3D('',#22217,#10368,#10369);
#9263=AXIS2_PLACEMENT_3D('',#22243,#10371,#10372);
#9264=AXIS2_PLACEMENT_3D('',#22245,#10373,#10374);
#9265=AXIS2_PLACEMENT_3D('',#22248,#10376,#10377);
#9266=AXIS2_PLACEMENT_3D('',#22249,#10378,#10379);
#9267=AXIS2_PLACEMENT_3D('',#22251,#10380,#10381);
#9268=AXIS2_PLACEMENT_3D('',#22254,#10383,#10384);
#9269=AXIS2_PLACEMENT_3D('',#22255,#10385,#10386);
#9270=AXIS2_PLACEMENT_3D('',#22257,#10387,#10388);
#9271=AXIS2_PLACEMENT_3D('',#22260,#10390,#10391);
#9272=AXIS2_PLACEMENT_3D('',#22261,#10392,#10393);
#9273=AXIS2_PLACEMENT_3D('',#22263,#10394,#10395);
#9274=AXIS2_PLACEMENT_3D('',#22266,#10397,#10398);
#9275=AXIS2_PLACEMENT_3D('',#22267,#10399,#10400);
#9276=AXIS2_PLACEMENT_3D('',#22269,#10401,#10402);
#9277=AXIS2_PLACEMENT_3D('',#22272,#10404,#10405);
#9278=AXIS2_PLACEMENT_3D('',#22273,#10406,#10407);
#9279=AXIS2_PLACEMENT_3D('',#22275,#10408,#10409);
#9280=AXIS2_PLACEMENT_3D('',#22278,#10411,#10412);
#9281=AXIS2_PLACEMENT_3D('',#22279,#10413,#10414);
#9282=AXIS2_PLACEMENT_3D('',#22281,#10415,#10416);
#9283=AXIS2_PLACEMENT_3D('',#22380,#10417,#10418);
#9284=AXIS2_PLACEMENT_3D('',#22381,#10419,#10420);
#9285=AXIS2_PLACEMENT_3D('',#22384,#10422,#10423);
#9286=AXIS2_PLACEMENT_3D('',#22385,#10424,#10425);
#9287=AXIS2_PLACEMENT_3D('',#25229,#10426,#10427);
#9288=AXIS2_PLACEMENT_3D('',#28011,#10428,#10429);
#9289=AXIS2_PLACEMENT_3D('',#28012,#10430,#10431);
#9290=AXIS2_PLACEMENT_3D('',#28013,#10432,#10433);
#9291=AXIS2_PLACEMENT_3D('',#28014,#10434,#10435);
#9292=AXIS2_PLACEMENT_3D('',#28015,#10436,#10437);
#9293=AXIS2_PLACEMENT_3D('',#28017,#10438,#10439);
#9294=AXIS2_PLACEMENT_3D('',#28020,#10441,#10442);
#9295=AXIS2_PLACEMENT_3D('',#28021,#10443,#10444);
#9296=AXIS2_PLACEMENT_3D('',#28022,#10445,#10446);
#9297=AXIS2_PLACEMENT_3D('',#28023,#10447,#10448);
#9298=AXIS2_PLACEMENT_3D('',#28024,#10449,#10450);
#9299=AXIS2_PLACEMENT_3D('',#28026,#10451,#10452);
#9300=AXIS2_PLACEMENT_3D('',#28029,#10454,#10455);
#9301=AXIS2_PLACEMENT_3D('',#28030,#10456,#10457);
#9302=AXIS2_PLACEMENT_3D('',#28031,#10458,#10459);
#9303=AXIS2_PLACEMENT_3D('',#28032,#10460,#10461);
#9304=AXIS2_PLACEMENT_3D('',#28033,#10462,#10463);
#9305=AXIS2_PLACEMENT_3D('',#28036,#10464,#10465);
#9306=AXIS2_PLACEMENT_3D('',#28040,#10467,#10468);
#9307=AXIS2_PLACEMENT_3D('',#28042,#10470,#10471);
#9308=AXIS2_PLACEMENT_3D('',#28046,#10473,#10474);
#9309=AXIS2_PLACEMENT_3D('',#28054,#10478,#10479);
#9310=AXIS2_PLACEMENT_3D('',#28056,#10481,#10482);
#9311=AXIS2_PLACEMENT_3D('',#28060,#10485,#10486);
#9312=AXIS2_PLACEMENT_3D('',#28062,#10487,#10488);
#9313=AXIS2_PLACEMENT_3D('',#28065,#10490,#10491);
#9314=AXIS2_PLACEMENT_3D('',#28066,#10492,#10493);
#9315=AXIS2_PLACEMENT_3D('',#28071,#10495,#10496);
#9316=AXIS2_PLACEMENT_3D('',#28074,#10498,#10499);
#9317=AXIS2_PLACEMENT_3D('',#28075,#10500,#10501);
#9318=AXIS2_PLACEMENT_3D('',#28081,#10505,#10506);
#9319=AXIS2_PLACEMENT_3D('',#28091,#10512,#10513);
#9320=AXIS2_PLACEMENT_3D('',#28095,#10516,#10517);
#9321=AXIS2_PLACEMENT_3D('',#28099,#10520,#10521);
#9322=AXIS2_PLACEMENT_3D('',#28102,#10524,#10525);
#9323=AXIS2_PLACEMENT_3D('',#28106,#10528,#10529);
#9324=AXIS2_PLACEMENT_3D('',#28110,#10532,#10533);
#9325=AXIS2_PLACEMENT_3D('',#28113,#10535,#10536);
#9326=AXIS2_PLACEMENT_3D('',#28114,#10537,#10538);
#9327=AXIS2_PLACEMENT_3D('',#28115,#10539,#10540);
#9328=AXIS2_PLACEMENT_3D('',#28116,#10541,#10542);
#9329=AXIS2_PLACEMENT_3D('',#28118,#10544,#10545);
#9330=AXIS2_PLACEMENT_3D('',#28119,#10546,#10547);
#9331=AXIS2_PLACEMENT_3D('',#28121,#10548,#10549);
#9332=AXIS2_PLACEMENT_3D('',#28124,#10551,#10552);
#9333=AXIS2_PLACEMENT_3D('',#28125,#10553,#10554);
#9334=AXIS2_PLACEMENT_3D('',#28134,#10559,#10560);
#9335=AXIS2_PLACEMENT_3D('',#28140,#10564,#10565);
#9336=AXIS2_PLACEMENT_3D('',#28146,#10569,#10570);
#9337=AXIS2_PLACEMENT_3D('',#28149,#10573,#10574);
#9338=AXIS2_PLACEMENT_3D('',#28150,#10575,#10576);
#9339=AXIS2_PLACEMENT_3D('',#28151,#10577,#10578);
#9340=AXIS2_PLACEMENT_3D('',#28153,#10579,#10580);
#9341=AXIS2_PLACEMENT_3D('',#28156,#10582,#10583);
#9342=AXIS2_PLACEMENT_3D('',#28157,#10584,#10585);
#9343=AXIS2_PLACEMENT_3D('',#28166,#10590,#10591);
#9344=AXIS2_PLACEMENT_3D('',#28172,#10595,#10596);
#9345=AXIS2_PLACEMENT_3D('',#28178,#10600,#10601);
#9346=AXIS2_PLACEMENT_3D('',#28181,#10604,#10605);
#9347=AXIS2_PLACEMENT_3D('',#28182,#10606,#10607);
#9348=AXIS2_PLACEMENT_3D('',#28183,#10608,#10609);
#9349=AXIS2_PLACEMENT_3D('',#28184,#10610,#10611);
#9350=AXIS2_PLACEMENT_3D('',#28189,#10613,#10614);
#9351=AXIS2_PLACEMENT_3D('',#28192,#10616,#10617);
#9352=AXIS2_PLACEMENT_3D('',#28193,#10618,#10619);
#9353=AXIS2_PLACEMENT_3D('',#28197,#10621,#10622);
#9354=AXIS2_PLACEMENT_3D('',#28199,#10624,#10625);
#9355=AXIS2_PLACEMENT_3D('',#28203,#10628,#10629);
#9356=AXIS2_PLACEMENT_3D('',#28207,#10632,#10633);
#9357=AXIS2_PLACEMENT_3D('',#28208,#10634,#10635);
#9358=AXIS2_PLACEMENT_3D('',#28209,#10636,#10637);
#9359=AXIS2_PLACEMENT_3D('',#28210,#10638,#10639);
#9360=AXIS2_PLACEMENT_3D('',#28212,#10640,#10641);
#9361=AXIS2_PLACEMENT_3D('',#28215,#10643,#10644);
#9362=AXIS2_PLACEMENT_3D('',#28216,#10645,#10646);
#9363=AXIS2_PLACEMENT_3D('',#28225,#10651,#10652);
#9364=AXIS2_PLACEMENT_3D('',#28231,#10656,#10657);
#9365=AXIS2_PLACEMENT_3D('',#28237,#10661,#10662);
#9366=AXIS2_PLACEMENT_3D('',#28240,#10665,#10666);
#9367=AXIS2_PLACEMENT_3D('',#28241,#10667,#10668);
#9368=AXIS2_PLACEMENT_3D('',#28242,#10669,#10670);
#9369=AXIS2_PLACEMENT_3D('',#28244,#10671,#10672);
#9370=AXIS2_PLACEMENT_3D('',#28247,#10674,#10675);
#9371=AXIS2_PLACEMENT_3D('',#28248,#10676,#10677);
#9372=AXIS2_PLACEMENT_3D('',#28257,#10682,#10683);
#9373=AXIS2_PLACEMENT_3D('',#28263,#10687,#10688);
#9374=AXIS2_PLACEMENT_3D('',#28269,#10692,#10693);
#9375=AXIS2_PLACEMENT_3D('',#28272,#10696,#10697);
#9376=AXIS2_PLACEMENT_3D('',#28273,#10698,#10699);
#9377=AXIS2_PLACEMENT_3D('',#28274,#10700,#10701);
#9378=AXIS2_PLACEMENT_3D('',#28275,#10702,#10703);
#9379=AXIS2_PLACEMENT_3D('',#28284,#10708,#10709);
#9380=AXIS2_PLACEMENT_3D('',#28293,#10714,#10715);
#9381=AXIS2_PLACEMENT_3D('',#28294,#10716,#10717);
#9382=AXIS2_PLACEMENT_3D('',#28295,#10718,#10719);
#9383=AXIS2_PLACEMENT_3D('',#28296,#10720,#10721);
#9384=AXIS2_PLACEMENT_3D('',#28297,#10722,#10723);
#9385=AXIS2_PLACEMENT_3D('',#28298,#10724,#10725);
#9386=AXIS2_PLACEMENT_3D('',#28299,#10726,#10727);
#9387=AXIS2_PLACEMENT_3D('',#28300,#10728,#10729);
#9388=AXIS2_PLACEMENT_3D('',#28301,#10730,#10731);
#9389=AXIS2_PLACEMENT_3D('',#28302,#10732,#10733);
#9390=AXIS2_PLACEMENT_3D('',#28311,#10738,#10739);
#9391=AXIS2_PLACEMENT_3D('',#28320,#10744,#10745);
#9392=AXIS2_PLACEMENT_3D('',#28321,#10746,#10747);
#9393=AXIS2_PLACEMENT_3D('',#28322,#10748,#10749);
#9394=AXIS2_PLACEMENT_3D('',#28323,#10750,#10751);
#9395=AXIS2_PLACEMENT_3D('',#28324,#10752,#10753);
#9396=AXIS2_PLACEMENT_3D('',#28325,#10754,#10755);
#9397=AXIS2_PLACEMENT_3D('',#28326,#10756,#10757);
#9398=AXIS2_PLACEMENT_3D('',#28327,#10758,#10759);
#9399=AXIS2_PLACEMENT_3D('',#28328,#10760,#10761);
#9400=AXIS2_PLACEMENT_3D('',#28329,#10762,#10763);
#9401=AXIS2_PLACEMENT_3D('',#28334,#10765,#10766);
#9402=AXIS2_PLACEMENT_3D('',#28338,#10768,#10769);
#9403=AXIS2_PLACEMENT_3D('',#28342,#10771,#10772);
#9404=AXIS2_PLACEMENT_3D('',#28345,#10774,#10775);
#9405=AXIS2_PLACEMENT_3D('',#28346,#10776,#10777);
#9406=AXIS2_PLACEMENT_3D('',#28352,#10781,#10782);
#9407=AXIS2_PLACEMENT_3D('',#28356,#10784,#10785);
#9408=AXIS2_PLACEMENT_3D('',#28358,#10787,#10788);
#9409=AXIS2_PLACEMENT_3D('',#28362,#10791,#10792);
#9410=AXIS2_PLACEMENT_3D('',#28370,#10797,#10798);
#9411=AXIS2_PLACEMENT_3D('',#28372,#10799,#10800);
#9412=AXIS2_PLACEMENT_3D('',#28375,#10802,#10803);
#9413=AXIS2_PLACEMENT_3D('',#28376,#10804,#10805);
#9414=AXIS2_PLACEMENT_3D('',#28381,#10807,#10808);
#9415=AXIS2_PLACEMENT_3D('',#28384,#10810,#10811);
#9416=AXIS2_PLACEMENT_3D('',#28385,#10812,#10813);
#9417=AXIS2_PLACEMENT_3D('',#28388,#10816,#10817);
#9418=AXIS2_PLACEMENT_3D('',#28396,#10822,#10823);
#9419=AXIS2_PLACEMENT_3D('',#28400,#10826,#10827);
#9420=AXIS2_PLACEMENT_3D('',#28404,#10830,#10831);
#9421=AXIS2_PLACEMENT_3D('',#28406,#10833,#10834);
#9422=AXIS2_PLACEMENT_3D('',#28408,#10836,#10837);
#9423=AXIS2_PLACEMENT_3D('',#28412,#10840,#10841);
#9424=AXIS2_PLACEMENT_3D('',#28413,#10842,#10843);
#9425=AXIS2_PLACEMENT_3D('',#28414,#10844,#10845);
#9426=AXIS2_PLACEMENT_3D('',#28415,#10846,#10847);
#9427=AXIS2_PLACEMENT_3D('',#28417,#10848,#10849);
#9428=AXIS2_PLACEMENT_3D('',#28420,#10851,#10852);
#9429=AXIS2_PLACEMENT_3D('',#28421,#10853,#10854);
#9430=AXIS2_PLACEMENT_3D('',#28430,#10859,#10860);
#9431=AXIS2_PLACEMENT_3D('',#28436,#10864,#10865);
#9432=AXIS2_PLACEMENT_3D('',#28442,#10869,#10870);
#9433=AXIS2_PLACEMENT_3D('',#28445,#10873,#10874);
#9434=AXIS2_PLACEMENT_3D('',#28446,#10875,#10876);
#9435=AXIS2_PLACEMENT_3D('',#28447,#10877,#10878);
#9436=AXIS2_PLACEMENT_3D('',#28449,#10879,#10880);
#9437=AXIS2_PLACEMENT_3D('',#28452,#10882,#10883);
#9438=AXIS2_PLACEMENT_3D('',#28453,#10884,#10885);
#9439=AXIS2_PLACEMENT_3D('',#28462,#10890,#10891);
#9440=AXIS2_PLACEMENT_3D('',#28468,#10895,#10896);
#9441=AXIS2_PLACEMENT_3D('',#28474,#10900,#10901);
#9442=AXIS2_PLACEMENT_3D('',#28477,#10904,#10905);
#9443=AXIS2_PLACEMENT_3D('',#28478,#10906,#10907);
#9444=AXIS2_PLACEMENT_3D('',#28479,#10908,#10909);
#9445=AXIS2_PLACEMENT_3D('',#28480,#10910,#10911);
#9446=AXIS2_PLACEMENT_3D('',#28485,#10913,#10914);
#9447=AXIS2_PLACEMENT_3D('',#28488,#10916,#10917);
#9448=AXIS2_PLACEMENT_3D('',#28489,#10918,#10919);
#9449=AXIS2_PLACEMENT_3D('',#28493,#10921,#10922);
#9450=AXIS2_PLACEMENT_3D('',#28495,#10924,#10925);
#9451=AXIS2_PLACEMENT_3D('',#28499,#10928,#10929);
#9452=AXIS2_PLACEMENT_3D('',#28503,#10932,#10933);
#9453=AXIS2_PLACEMENT_3D('',#28504,#10934,#10935);
#9454=AXIS2_PLACEMENT_3D('',#28505,#10936,#10937);
#9455=AXIS2_PLACEMENT_3D('',#28506,#10938,#10939);
#9456=AXIS2_PLACEMENT_3D('',#28508,#10940,#10941);
#9457=AXIS2_PLACEMENT_3D('',#28511,#10943,#10944);
#9458=AXIS2_PLACEMENT_3D('',#28512,#10945,#10946);
#9459=AXIS2_PLACEMENT_3D('',#28521,#10951,#10952);
#9460=AXIS2_PLACEMENT_3D('',#28527,#10956,#10957);
#9461=AXIS2_PLACEMENT_3D('',#28533,#10961,#10962);
#9462=AXIS2_PLACEMENT_3D('',#28536,#10965,#10966);
#9463=AXIS2_PLACEMENT_3D('',#28537,#10967,#10968);
#9464=AXIS2_PLACEMENT_3D('',#28538,#10969,#10970);
#9465=AXIS2_PLACEMENT_3D('',#28540,#10971,#10972);
#9466=AXIS2_PLACEMENT_3D('',#28543,#10974,#10975);
#9467=AXIS2_PLACEMENT_3D('',#28544,#10976,#10977);
#9468=AXIS2_PLACEMENT_3D('',#28553,#10982,#10983);
#9469=AXIS2_PLACEMENT_3D('',#28559,#10987,#10988);
#9470=AXIS2_PLACEMENT_3D('',#28565,#10992,#10993);
#9471=AXIS2_PLACEMENT_3D('',#28568,#10996,#10997);
#9472=AXIS2_PLACEMENT_3D('',#28569,#10998,#10999);
#9473=AXIS2_PLACEMENT_3D('',#28570,#11000,#11001);
#9474=AXIS2_PLACEMENT_3D('',#28571,#11002,#11003);
#9475=AXIS2_PLACEMENT_3D('',#28580,#11008,#11009);
#9476=AXIS2_PLACEMENT_3D('',#28589,#11014,#11015);
#9477=AXIS2_PLACEMENT_3D('',#28590,#11016,#11017);
#9478=AXIS2_PLACEMENT_3D('',#28591,#11018,#11019);
#9479=AXIS2_PLACEMENT_3D('',#28592,#11020,#11021);
#9480=AXIS2_PLACEMENT_3D('',#28593,#11022,#11023);
#9481=AXIS2_PLACEMENT_3D('',#28594,#11024,#11025);
#9482=AXIS2_PLACEMENT_3D('',#28595,#11026,#11027);
#9483=AXIS2_PLACEMENT_3D('',#28596,#11028,#11029);
#9484=AXIS2_PLACEMENT_3D('',#28597,#11030,#11031);
#9485=AXIS2_PLACEMENT_3D('',#28598,#11032,#11033);
#9486=AXIS2_PLACEMENT_3D('',#28607,#11038,#11039);
#9487=AXIS2_PLACEMENT_3D('',#28616,#11044,#11045);
#9488=AXIS2_PLACEMENT_3D('',#28617,#11046,#11047);
#9489=AXIS2_PLACEMENT_3D('',#28618,#11048,#11049);
#9490=AXIS2_PLACEMENT_3D('',#28619,#11050,#11051);
#9491=AXIS2_PLACEMENT_3D('',#28620,#11052,#11053);
#9492=AXIS2_PLACEMENT_3D('',#28621,#11054,#11055);
#9493=AXIS2_PLACEMENT_3D('',#28622,#11056,#11057);
#9494=AXIS2_PLACEMENT_3D('',#28623,#11058,#11059);
#9495=AXIS2_PLACEMENT_3D('',#28624,#11060,#11061);
#9496=AXIS2_PLACEMENT_3D('',#28625,#11062,#11063);
#9497=AXIS2_PLACEMENT_3D('',#28634,#11068,#11069);
#9498=AXIS2_PLACEMENT_3D('',#28640,#11073,#11074);
#9499=AXIS2_PLACEMENT_3D('',#28646,#11078,#11079);
#9500=AXIS2_PLACEMENT_3D('',#28649,#11082,#11083);
#9501=AXIS2_PLACEMENT_3D('',#28650,#11084,#11085);
#9502=AXIS2_PLACEMENT_3D('',#28651,#11086,#11087);
#9503=AXIS2_PLACEMENT_3D('',#28652,#11088,#11089);
#9504=AXIS2_PLACEMENT_3D('',#28661,#11094,#11095);
#9505=AXIS2_PLACEMENT_3D('',#28667,#11099,#11100);
#9506=AXIS2_PLACEMENT_3D('',#28673,#11104,#11105);
#9507=AXIS2_PLACEMENT_3D('',#28676,#11108,#11109);
#9508=AXIS2_PLACEMENT_3D('',#28677,#11110,#11111);
#9509=AXIS2_PLACEMENT_3D('',#28678,#11112,#11113);
#9510=AXIS2_PLACEMENT_3D('',#28679,#11114,#11115);
#9511=AXIS2_PLACEMENT_3D('',#28688,#11120,#11121);
#9512=AXIS2_PLACEMENT_3D('',#28694,#11125,#11126);
#9513=AXIS2_PLACEMENT_3D('',#28700,#11130,#11131);
#9514=AXIS2_PLACEMENT_3D('',#28706,#11135,#11136);
#9515=AXIS2_PLACEMENT_3D('',#28712,#11140,#11141);
#9516=AXIS2_PLACEMENT_3D('',#28715,#11144,#11145);
#9517=AXIS2_PLACEMENT_3D('',#28716,#11146,#11147);
#9518=AXIS2_PLACEMENT_3D('',#28717,#11148,#11149);
#9519=AXIS2_PLACEMENT_3D('',#28719,#11150,#11151);
#9520=AXIS2_PLACEMENT_3D('',#28720,#11152,#11153);
#9521=AXIS2_PLACEMENT_3D('',#28722,#11154,#11155);
#9522=AXIS2_PLACEMENT_3D('',#28723,#11156,#11157);
#9523=AXIS2_PLACEMENT_3D('',#28725,#11158,#11159);
#9524=AXIS2_PLACEMENT_3D('',#28727,#11161,#11162);
#9525=AXIS2_PLACEMENT_3D('',#28729,#11163,#11164);
#9526=AXIS2_PLACEMENT_3D('',#28731,#11166,#11167);
#9527=AXIS2_PLACEMENT_3D('',#28733,#11168,#11169);
#9528=AXIS2_PLACEMENT_3D('',#28735,#11171,#11172);
#9529=AXIS2_PLACEMENT_3D('',#28737,#11173,#11174);
#9530=AXIS2_PLACEMENT_3D('',#28738,#11175,#11176);
#9531=AXIS2_PLACEMENT_3D('',#28740,#11177,#11178);
#9532=AXIS2_PLACEMENT_3D('',#28742,#11180,#11181);
#9533=AXIS2_PLACEMENT_3D('',#28744,#11183,#11184);
#9534=AXIS2_PLACEMENT_3D('',#28745,#11185,#11186);
#9535=AXIS2_PLACEMENT_3D('',#28754,#11191,#11192);
#9536=AXIS2_PLACEMENT_3D('',#28760,#11196,#11197);
#9537=AXIS2_PLACEMENT_3D('',#28766,#11201,#11202);
#9538=AXIS2_PLACEMENT_3D('',#28772,#11206,#11207);
#9539=AXIS2_PLACEMENT_3D('',#28778,#11211,#11212);
#9540=AXIS2_PLACEMENT_3D('',#28781,#11215,#11216);
#9541=AXIS2_PLACEMENT_3D('',#28782,#11217,#11218);
#9542=AXIS2_PLACEMENT_3D('',#28783,#11219,#11220);
#9543=AXIS2_PLACEMENT_3D('',#28785,#11221,#11222);
#9544=AXIS2_PLACEMENT_3D('',#28787,#11223,#11224);
#9545=AXIS2_PLACEMENT_3D('',#28788,#11225,#11226);
#9546=AXIS2_PLACEMENT_3D('',#28791,#11228,#11229);
#9547=AXIS2_PLACEMENT_3D('',#28792,#11230,#11231);
#9548=AXIS2_PLACEMENT_3D('',#28793,#11232,#11233);
#9549=AXIS2_PLACEMENT_3D('',#28795,#11234,#11235);
#9550=AXIS2_PLACEMENT_3D('',#28796,#11236,#11237);
#9551=AXIS2_PLACEMENT_3D('',#28798,#11238,#11239);
#9552=AXIS2_PLACEMENT_3D('',#28800,#11241,#11242);
#9553=AXIS2_PLACEMENT_3D('',#28802,#11243,#11244);
#9554=AXIS2_PLACEMENT_3D('',#28804,#11246,#11247);
#9555=AXIS2_PLACEMENT_3D('',#28806,#11248,#11249);
#9556=AXIS2_PLACEMENT_3D('',#28808,#11251,#11252);
#9557=AXIS2_PLACEMENT_3D('',#28810,#11253,#11254);
#9558=AXIS2_PLACEMENT_3D('',#28811,#11255,#11256);
#9559=AXIS2_PLACEMENT_3D('',#28813,#11257,#11258);
#9560=AXIS2_PLACEMENT_3D('',#28815,#11260,#11261);
#9561=AXIS2_PLACEMENT_3D('',#28817,#11263,#11264);
#9562=AXIS2_PLACEMENT_3D('',#28818,#11265,#11266);
#9563=AXIS2_PLACEMENT_3D('',#28820,#11267,#11268);
#9564=AXIS2_PLACEMENT_3D('',#28823,#11270,#11271);
#9565=AXIS2_PLACEMENT_3D('',#28824,#11272,#11273);
#9566=AXIS2_PLACEMENT_3D('',#28826,#11274,#11275);
#9567=AXIS2_PLACEMENT_3D('',#28829,#11277,#11278);
#9568=AXIS2_PLACEMENT_3D('',#28830,#11279,#11280);
#9569=AXIS2_PLACEMENT_3D('',#28831,#11281,#11282);
#9570=AXIS2_PLACEMENT_3D('',#28832,#11283,#11284);
#9571=AXIS2_PLACEMENT_3D('',#28833,#11285,#11286);
#9572=AXIS2_PLACEMENT_3D('',#28845,#11288,#11289);
#9573=AXIS2_PLACEMENT_3D('',#28861,#11290,#11291);
#9574=AXIS2_PLACEMENT_3D('',#28863,#11292,#11293);
#9575=AXIS2_PLACEMENT_3D('',#28889,#11295,#11296);
#9576=AXIS2_PLACEMENT_3D('',#28892,#11299,#11300);
#9577=AXIS2_PLACEMENT_3D('',#28894,#11302,#11303);
#9578=AXIS2_PLACEMENT_3D('',#28896,#11305,#11306);
#9579=AXIS2_PLACEMENT_3D('',#28898,#11307,#11308);
#9580=AXIS2_PLACEMENT_3D('',#28901,#11310,#11311);
#9581=AXIS2_PLACEMENT_3D('',#28902,#11312,#11313);
#9582=AXIS2_PLACEMENT_3D('',#28904,#11315,#11316);
#9583=AXIS2_PLACEMENT_3D('',#28906,#11318,#11319);
#9584=AXIS2_PLACEMENT_3D('',#28907,#11320,#11321);
#9585=AXIS2_PLACEMENT_3D('',#28908,#11322,#11323);
#9586=AXIS2_PLACEMENT_3D('',#28909,#11324,#11325);
#9587=AXIS2_PLACEMENT_3D('',#28910,#11326,#11327);
#9588=AXIS2_PLACEMENT_3D('',#28911,#11328,#11329);
#9589=AXIS2_PLACEMENT_3D('',#28912,#11330,#11331);
#9590=AXIS2_PLACEMENT_3D('',#28913,#11332,#11333);
#9591=AXIS2_PLACEMENT_3D('',#28914,#11334,#11335);
#9592=AXIS2_PLACEMENT_3D('',#28915,#11336,#11337);
#9593=AXIS2_PLACEMENT_3D('',#28916,#11338,#11339);
#9594=AXIS2_PLACEMENT_3D('',#28917,#11340,#11341);
#9595=AXIS2_PLACEMENT_3D('',#28918,#11342,#11343);
#9596=AXIS2_PLACEMENT_3D('',#28919,#11344,#11345);
#9597=AXIS2_PLACEMENT_3D('',#28920,#11346,#11347);
#9598=AXIS2_PLACEMENT_3D('',#28921,#11348,#11349);
#9599=AXIS2_PLACEMENT_3D('',#28922,#11350,#11351);
#9600=AXIS2_PLACEMENT_3D('',#28923,#11352,#11353);
#9601=AXIS2_PLACEMENT_3D('',#28924,#11354,#11355);
#9602=AXIS2_PLACEMENT_3D('',#28925,#11356,#11357);
#9603=AXIS2_PLACEMENT_3D('',#28926,#11358,#11359);
#9604=AXIS2_PLACEMENT_3D('',#28927,#11360,#11361);
#9605=AXIS2_PLACEMENT_3D('',#28928,#11362,#11363);
#9606=AXIS2_PLACEMENT_3D('',#28929,#11364,#11365);
#9607=AXIS2_PLACEMENT_3D('',#28930,#11366,#11367);
#9608=AXIS2_PLACEMENT_3D('',#28931,#11368,#11369);
#9609=AXIS2_PLACEMENT_3D('',#28932,#11370,#11371);
#9610=AXIS2_PLACEMENT_3D('',#28933,#11372,#11373);
#9611=AXIS2_PLACEMENT_3D('',#28934,#11374,#11375);
#9612=AXIS2_PLACEMENT_3D('',#28935,#11376,#11377);
#9613=AXIS2_PLACEMENT_3D('',#28936,#11378,#11379);
#9614=AXIS2_PLACEMENT_3D('',#28937,#11380,#11381);
#9615=AXIS2_PLACEMENT_3D('',#28938,#11382,#11383);
#9616=AXIS2_PLACEMENT_3D('',#28939,#11384,#11385);
#9617=AXIS2_PLACEMENT_3D('',#28940,#11386,#11387);
#9618=AXIS2_PLACEMENT_3D('',#28941,#11388,#11389);
#9619=AXIS2_PLACEMENT_3D('',#28942,#11390,#11391);
#9620=AXIS2_PLACEMENT_3D('',#28943,#11392,#11393);
#9621=AXIS2_PLACEMENT_3D('',#28944,#11394,#11395);
#9622=AXIS2_PLACEMENT_3D('',#28945,#11396,#11397);
#9623=AXIS2_PLACEMENT_3D('',#28958,#11399,#11400);
#9624=AXIS2_PLACEMENT_3D('',#28978,#11401,#11402);
#9625=AXIS2_PLACEMENT_3D('',#29068,#11404,#11405);
#9626=AXIS2_PLACEMENT_3D('',#29158,#11407,#11408);
#9627=AXIS2_PLACEMENT_3D('',#29189,#11410,#11411);
#9628=AXIS2_PLACEMENT_3D('',#29227,#11412,#11413);
#9629=AXIS2_PLACEMENT_3D('',#29246,#11415,#11416);
#9630=AXIS2_PLACEMENT_3D('',#29261,#11417,#11418);
#9631=AXIS2_PLACEMENT_3D('',#29299,#11420,#11421);
#9632=AXIS2_PLACEMENT_3D('',#29337,#11423,#11424);
#9633=AXIS2_PLACEMENT_3D('',#29349,#11426,#11427);
#9634=AXIS2_PLACEMENT_3D('',#29357,#11428,#11429);
#9635=AXIS2_PLACEMENT_3D('',#30260,#11430,#11431);
#9636=AXIS2_PLACEMENT_3D('',#30273,#11438,#11439);
#9637=AXIS2_PLACEMENT_3D('',#30274,#11440,#11441);
#9638=AXIS2_PLACEMENT_3D('',#30280,#11445,#11446);
#9639=AXIS2_PLACEMENT_3D('',#30284,#11449,#11450);
#9640=AXIS2_PLACEMENT_3D('',#30288,#11453,#11454);
#9641=AXIS2_PLACEMENT_3D('',#30292,#11457,#11458);
#9642=AXIS2_PLACEMENT_3D('',#30296,#11461,#11462);
#9643=AXIS2_PLACEMENT_3D('',#30298,#11464,#11465);
#9644=AXIS2_PLACEMENT_3D('',#30299,#11466,#11467);
#9645=AXIS2_PLACEMENT_3D('',#30300,#11468,#11469);
#9646=AXIS2_PLACEMENT_3D('',#30301,#11470,#11471);
#9647=AXIS2_PLACEMENT_3D('',#30302,#11472,#11473);
#9648=AXIS2_PLACEMENT_3D('',#30315,#11475,#11476);
#9649=AXIS2_PLACEMENT_3D('',#30335,#11477,#11478);
#9650=AXIS2_PLACEMENT_3D('',#30425,#11480,#11481);
#9651=AXIS2_PLACEMENT_3D('',#30515,#11483,#11484);
#9652=AXIS2_PLACEMENT_3D('',#30546,#11486,#11487);
#9653=AXIS2_PLACEMENT_3D('',#30584,#11488,#11489);
#9654=AXIS2_PLACEMENT_3D('',#30603,#11491,#11492);
#9655=AXIS2_PLACEMENT_3D('',#30618,#11493,#11494);
#9656=AXIS2_PLACEMENT_3D('',#30656,#11496,#11497);
#9657=AXIS2_PLACEMENT_3D('',#30694,#11499,#11500);
#9658=AXIS2_PLACEMENT_3D('',#30706,#11502,#11503);
#9659=AXIS2_PLACEMENT_3D('',#30714,#11504,#11505);
#9660=AXIS2_PLACEMENT_3D('',#31617,#11506,#11507);
#9661=AXIS2_PLACEMENT_3D('',#31630,#11514,#11515);
#9662=AXIS2_PLACEMENT_3D('',#31631,#11516,#11517);
#9663=AXIS2_PLACEMENT_3D('',#31637,#11521,#11522);
#9664=AXIS2_PLACEMENT_3D('',#31641,#11525,#11526);
#9665=AXIS2_PLACEMENT_3D('',#31645,#11529,#11530);
#9666=AXIS2_PLACEMENT_3D('',#31649,#11533,#11534);
#9667=AXIS2_PLACEMENT_3D('',#31653,#11537,#11538);
#9668=AXIS2_PLACEMENT_3D('',#31655,#11540,#11541);
#9669=AXIS2_PLACEMENT_3D('',#31656,#11542,#11543);
#9670=AXIS2_PLACEMENT_3D('',#31657,#11544,#11545);
#9671=AXIS2_PLACEMENT_3D('',#31658,#11546,#11547);
#9672=AXIS2_PLACEMENT_3D('',#31659,#11548,#11549);
#9673=AXIS2_PLACEMENT_3D('',#31672,#11551,#11552);
#9674=AXIS2_PLACEMENT_3D('',#31692,#11553,#11554);
#9675=AXIS2_PLACEMENT_3D('',#31782,#11556,#11557);
#9676=AXIS2_PLACEMENT_3D('',#31872,#11559,#11560);
#9677=AXIS2_PLACEMENT_3D('',#31903,#11562,#11563);
#9678=AXIS2_PLACEMENT_3D('',#31941,#11564,#11565);
#9679=AXIS2_PLACEMENT_3D('',#31960,#11567,#11568);
#9680=AXIS2_PLACEMENT_3D('',#31975,#11569,#11570);
#9681=AXIS2_PLACEMENT_3D('',#32013,#11572,#11573);
#9682=AXIS2_PLACEMENT_3D('',#32051,#11575,#11576);
#9683=AXIS2_PLACEMENT_3D('',#32063,#11578,#11579);
#9684=AXIS2_PLACEMENT_3D('',#32071,#11580,#11581);
#9685=AXIS2_PLACEMENT_3D('',#32974,#11582,#11583);
#9686=AXIS2_PLACEMENT_3D('',#32987,#11590,#11591);
#9687=AXIS2_PLACEMENT_3D('',#32988,#11592,#11593);
#9688=AXIS2_PLACEMENT_3D('',#32994,#11597,#11598);
#9689=AXIS2_PLACEMENT_3D('',#32998,#11601,#11602);
#9690=AXIS2_PLACEMENT_3D('',#33002,#11605,#11606);
#9691=AXIS2_PLACEMENT_3D('',#33006,#11609,#11610);
#9692=AXIS2_PLACEMENT_3D('',#33010,#11613,#11614);
#9693=AXIS2_PLACEMENT_3D('',#33012,#11616,#11617);
#9694=AXIS2_PLACEMENT_3D('',#33013,#11618,#11619);
#9695=AXIS2_PLACEMENT_3D('',#33014,#11620,#11621);
#9696=AXIS2_PLACEMENT_3D('',#33015,#11622,#11623);
#9697=AXIS2_PLACEMENT_3D('',#33016,#11624,#11625);
#9698=AXIS2_PLACEMENT_3D('',#33029,#11627,#11628);
#9699=AXIS2_PLACEMENT_3D('',#33049,#11629,#11630);
#9700=AXIS2_PLACEMENT_3D('',#33139,#11632,#11633);
#9701=AXIS2_PLACEMENT_3D('',#33229,#11635,#11636);
#9702=AXIS2_PLACEMENT_3D('',#33260,#11638,#11639);
#9703=AXIS2_PLACEMENT_3D('',#33298,#11640,#11641);
#9704=AXIS2_PLACEMENT_3D('',#33317,#11643,#11644);
#9705=AXIS2_PLACEMENT_3D('',#33332,#11645,#11646);
#9706=AXIS2_PLACEMENT_3D('',#33370,#11648,#11649);
#9707=AXIS2_PLACEMENT_3D('',#33408,#11651,#11652);
#9708=AXIS2_PLACEMENT_3D('',#33420,#11654,#11655);
#9709=AXIS2_PLACEMENT_3D('',#33428,#11656,#11657);
#9710=AXIS2_PLACEMENT_3D('',#34331,#11658,#11659);
#9711=AXIS2_PLACEMENT_3D('',#34344,#11666,#11667);
#9712=AXIS2_PLACEMENT_3D('',#34345,#11668,#11669);
#9713=AXIS2_PLACEMENT_3D('',#34351,#11673,#11674);
#9714=AXIS2_PLACEMENT_3D('',#34355,#11677,#11678);
#9715=AXIS2_PLACEMENT_3D('',#34359,#11681,#11682);
#9716=AXIS2_PLACEMENT_3D('',#34363,#11685,#11686);
#9717=AXIS2_PLACEMENT_3D('',#34367,#11689,#11690);
#9718=AXIS2_PLACEMENT_3D('',#34369,#11692,#11693);
#9719=AXIS2_PLACEMENT_3D('',#34370,#11694,#11695);
#9720=AXIS2_PLACEMENT_3D('',#34371,#11696,#11697);
#9721=AXIS2_PLACEMENT_3D('',#34372,#11698,#11699);
#9722=AXIS2_PLACEMENT_3D('',#34373,#11700,#11701);
#9723=AXIS2_PLACEMENT_3D('',#34374,#11702,#11703);
#9724=AXIS2_PLACEMENT_3D('',#34375,#11704,#11705);
#9725=DIRECTION('axis',(0.,0.,1.));
#9726=DIRECTION('refdir',(1.,0.,0.));
#9727=DIRECTION('axis',(0.,0.,1.));
#9728=DIRECTION('refdir',(1.,0.,0.));
#9729=DIRECTION('axis',(0.,0.,1.));
#9730=DIRECTION('refdir',(1.,0.,0.));
#9731=DIRECTION('center_axis',(0.,0.,1.));
#9732=DIRECTION('ref_axis',(1.,0.,0.));
#9733=DIRECTION('center_axis',(0.,0.,1.));
#9734=DIRECTION('ref_axis',(1.,0.,0.));
#9735=DIRECTION('',(0.,0.,1.));
#9736=DIRECTION('center_axis',(0.,0.,-1.));
#9737=DIRECTION('ref_axis',(1.,0.,0.));
#9738=DIRECTION('center_axis',(0.,0.,1.));
#9739=DIRECTION('ref_axis',(1.,0.,0.));
#9740=DIRECTION('center_axis',(0.,0.,1.));
#9741=DIRECTION('ref_axis',(1.,0.,0.));
#9742=DIRECTION('center_axis',(0.,0.,1.));
#9743=DIRECTION('ref_axis',(1.,0.,0.));
#9744=DIRECTION('',(0.,0.,1.));
#9745=DIRECTION('center_axis',(0.,0.,-1.));
#9746=DIRECTION('ref_axis',(1.,0.,0.));
#9747=DIRECTION('center_axis',(0.,0.,1.));
#9748=DIRECTION('ref_axis',(1.,0.,0.));
#9749=DIRECTION('center_axis',(0.,0.,1.));
#9750=DIRECTION('ref_axis',(1.,0.,0.));
#9751=DIRECTION('center_axis',(0.,0.,1.));
#9752=DIRECTION('ref_axis',(1.,0.,0.));
#9753=DIRECTION('',(0.,0.,1.));
#9754=DIRECTION('center_axis',(0.,0.,-1.));
#9755=DIRECTION('ref_axis',(1.,0.,0.));
#9756=DIRECTION('center_axis',(0.,0.,1.));
#9757=DIRECTION('ref_axis',(1.,0.,0.));
#9758=DIRECTION('center_axis',(0.,0.,1.));
#9759=DIRECTION('ref_axis',(1.,0.,0.));
#9760=DIRECTION('',(0.,0.,1.));
#9761=DIRECTION('center_axis',(0.,0.,-1.));
#9762=DIRECTION('ref_axis',(1.,0.,0.));
#9763=DIRECTION('center_axis',(0.,0.,1.));
#9764=DIRECTION('ref_axis',(1.,0.,0.));
#9765=DIRECTION('center_axis',(0.,0.,1.));
#9766=DIRECTION('ref_axis',(1.,0.,0.));
#9767=DIRECTION('',(0.,0.,1.));
#9768=DIRECTION('center_axis',(0.,0.,-1.));
#9769=DIRECTION('ref_axis',(1.,0.,0.));
#9770=DIRECTION('center_axis',(0.,0.,1.));
#9771=DIRECTION('ref_axis',(1.,0.,0.));
#9772=DIRECTION('center_axis',(0.,0.,1.));
#9773=DIRECTION('ref_axis',(1.,0.,0.));
#9774=DIRECTION('',(0.,0.,1.));
#9775=DIRECTION('center_axis',(0.,0.,-1.));
#9776=DIRECTION('ref_axis',(1.,0.,0.));
#9777=DIRECTION('center_axis',(0.,1.,0.));
#9778=DIRECTION('ref_axis',(-1.,0.,0.));
#9779=DIRECTION('',(-1.,0.,0.));
#9780=DIRECTION('',(0.,0.,1.));
#9781=DIRECTION('',(-1.,0.,0.));
#9782=DIRECTION('',(0.,0.,1.));
#9783=DIRECTION('center_axis',(1.,0.,0.));
#9784=DIRECTION('ref_axis',(0.,1.,0.));
#9785=DIRECTION('',(0.,1.,0.));
#9786=DIRECTION('',(0.,1.,0.));
#9787=DIRECTION('',(0.,0.,1.));
#9788=DIRECTION('center_axis',(0.,-1.,0.));
#9789=DIRECTION('ref_axis',(1.,0.,0.));
#9790=DIRECTION('',(1.,0.,0.));
#9791=DIRECTION('',(1.,0.,0.));
#9792=DIRECTION('',(0.,0.,1.));
#9793=DIRECTION('center_axis',(-1.,0.,0.));
#9794=DIRECTION('ref_axis',(0.,-1.,0.));
#9795=DIRECTION('',(0.,-1.,0.));
#9796=DIRECTION('',(0.,-1.,0.));
#9797=DIRECTION('center_axis',(0.,0.,1.));
#9798=DIRECTION('ref_axis',(1.,0.,0.));
#9799=DIRECTION('center_axis',(0.,0.,1.));
#9800=DIRECTION('ref_axis',(1.,0.,0.));
#9801=DIRECTION('axis',(0.,0.,1.));
#9802=DIRECTION('refdir',(1.,0.,0.));
#9803=DIRECTION('center_axis',(0.,0.,1.));
#9804=DIRECTION('ref_axis',(1.,0.,0.));
#9805=DIRECTION('',(0.,0.,-1.));
#9806=DIRECTION('center_axis',(0.,0.,-1.));
#9807=DIRECTION('ref_axis',(1.,0.,0.));
#9808=DIRECTION('center_axis',(0.,0.,1.));
#9809=DIRECTION('ref_axis',(1.,0.,0.));
#9810=DIRECTION('',(0.,0.,-1.));
#9811=DIRECTION('center_axis',(0.,0.,1.));
#9812=DIRECTION('ref_axis',(1.,0.,0.));
#9813=DIRECTION('',(0.,0.,-1.));
#9814=DIRECTION('center_axis',(0.,0.,1.));
#9815=DIRECTION('ref_axis',(1.,0.,0.));
#9816=DIRECTION('',(0.,0.,-1.));
#9817=DIRECTION('center_axis',(0.,0.,1.));
#9818=DIRECTION('ref_axis',(1.,0.,0.));
#9819=DIRECTION('',(0.,0.,-1.));
#9820=DIRECTION('center_axis',(0.,0.,1.));
#9821=DIRECTION('ref_axis',(1.,0.,0.));
#9822=DIRECTION('',(0.,0.,-1.));
#9823=DIRECTION('center_axis',(0.,0.,1.));
#9824=DIRECTION('ref_axis',(1.,0.,0.));
#9825=DIRECTION('',(0.,0.,-1.));
#9826=DIRECTION('center_axis',(0.,0.,1.));
#9827=DIRECTION('ref_axis',(1.,0.,0.));
#9828=DIRECTION('',(0.,0.,-1.));
#9829=DIRECTION('center_axis',(0.,0.,1.));
#9830=DIRECTION('ref_axis',(1.,0.,0.));
#9831=DIRECTION('',(0.,0.,-1.));
#9832=DIRECTION('center_axis',(0.,0.,1.));
#9833=DIRECTION('ref_axis',(1.,0.,0.));
#9834=DIRECTION('',(0.,0.,-1.));
#9835=DIRECTION('center_axis',(0.,0.,1.));
#9836=DIRECTION('ref_axis',(1.,0.,0.));
#9837=DIRECTION('',(0.,0.,-1.));
#9838=DIRECTION('center_axis',(0.,0.,1.));
#9839=DIRECTION('ref_axis',(1.,0.,0.));
#9840=DIRECTION('',(0.,0.,-1.));
#9841=DIRECTION('center_axis',(0.,0.,1.));
#9842=DIRECTION('ref_axis',(1.,0.,0.));
#9843=DIRECTION('',(0.,0.,-1.));
#9844=DIRECTION('center_axis',(0.,0.,1.));
#9845=DIRECTION('ref_axis',(1.,0.,0.));
#9846=DIRECTION('',(0.,0.,-1.));
#9847=DIRECTION('center_axis',(0.,0.,1.));
#9848=DIRECTION('ref_axis',(1.,0.,0.));
#9849=DIRECTION('',(0.,0.,-1.));
#9850=DIRECTION('center_axis',(0.,0.,1.));
#9851=DIRECTION('ref_axis',(1.,0.,0.));
#9852=DIRECTION('',(0.,0.,-1.));
#9853=DIRECTION('center_axis',(0.,0.,1.));
#9854=DIRECTION('ref_axis',(1.,0.,0.));
#9855=DIRECTION('',(0.,0.,-1.));
#9856=DIRECTION('center_axis',(0.,0.,1.));
#9857=DIRECTION('ref_axis',(1.,0.,0.));
#9858=DIRECTION('',(0.,0.,-1.));
#9859=DIRECTION('center_axis',(0.,0.,1.));
#9860=DIRECTION('ref_axis',(1.,0.,0.));
#9861=DIRECTION('',(0.,0.,-1.));
#9862=DIRECTION('center_axis',(0.,0.,1.));
#9863=DIRECTION('ref_axis',(1.,0.,0.));
#9864=DIRECTION('',(0.,0.,-1.));
#9865=DIRECTION('center_axis',(0.,0.,1.));
#9866=DIRECTION('ref_axis',(1.,0.,0.));
#9867=DIRECTION('',(0.,0.,-1.));
#9868=DIRECTION('center_axis',(0.,0.,1.));
#9869=DIRECTION('ref_axis',(1.,0.,0.));
#9870=DIRECTION('',(0.,0.,-1.));
#9871=DIRECTION('center_axis',(0.,0.,1.));
#9872=DIRECTION('ref_axis',(1.,0.,0.));
#9873=DIRECTION('',(0.,0.,-1.));
#9874=DIRECTION('center_axis',(0.,0.,1.));
#9875=DIRECTION('ref_axis',(1.,0.,0.));
#9876=DIRECTION('',(0.,0.,-1.));
#9877=DIRECTION('center_axis',(0.,0.,1.));
#9878=DIRECTION('ref_axis',(1.,0.,0.));
#9879=DIRECTION('',(0.,0.,-1.));
#9880=DIRECTION('center_axis',(0.,0.,1.));
#9881=DIRECTION('ref_axis',(1.,0.,0.));
#9882=DIRECTION('',(0.,0.,-1.));
#9883=DIRECTION('center_axis',(0.,0.,1.));
#9884=DIRECTION('ref_axis',(1.,0.,0.));
#9885=DIRECTION('',(0.,0.,-1.));
#9886=DIRECTION('center_axis',(0.,0.,1.));
#9887=DIRECTION('ref_axis',(1.,0.,0.));
#9888=DIRECTION('',(0.,0.,-1.));
#9889=DIRECTION('center_axis',(0.,0.,1.));
#9890=DIRECTION('ref_axis',(1.,0.,0.));
#9891=DIRECTION('',(0.,0.,-1.));
#9892=DIRECTION('center_axis',(0.,0.,1.));
#9893=DIRECTION('ref_axis',(1.,0.,0.));
#9894=DIRECTION('',(0.,0.,-1.));
#9895=DIRECTION('center_axis',(0.,0.,1.));
#9896=DIRECTION('ref_axis',(1.,0.,0.));
#9897=DIRECTION('',(0.,0.,-1.));
#9898=DIRECTION('center_axis',(0.,0.,1.));
#9899=DIRECTION('ref_axis',(1.,0.,0.));
#9900=DIRECTION('',(0.,0.,-1.));
#9901=DIRECTION('center_axis',(0.,0.,1.));
#9902=DIRECTION('ref_axis',(1.,0.,0.));
#9903=DIRECTION('',(0.,0.,-1.));
#9904=DIRECTION('center_axis',(0.,0.,1.));
#9905=DIRECTION('ref_axis',(1.,0.,0.));
#9906=DIRECTION('',(0.,0.,-1.));
#9907=DIRECTION('center_axis',(0.,0.,1.));
#9908=DIRECTION('ref_axis',(1.,0.,0.));
#9909=DIRECTION('',(0.,0.,-1.));
#9910=DIRECTION('center_axis',(0.,0.,1.));
#9911=DIRECTION('ref_axis',(1.,0.,0.));
#9912=DIRECTION('',(0.,0.,-1.));
#9913=DIRECTION('center_axis',(0.,0.,1.));
#9914=DIRECTION('ref_axis',(1.,0.,0.));
#9915=DIRECTION('',(0.,0.,-1.));
#9916=DIRECTION('center_axis',(0.,0.,1.));
#9917=DIRECTION('ref_axis',(1.,0.,0.));
#9918=DIRECTION('',(0.,0.,-1.));
#9919=DIRECTION('center_axis',(0.,0.,1.));
#9920=DIRECTION('ref_axis',(1.,0.,0.));
#9921=DIRECTION('',(0.,0.,-1.));
#9922=DIRECTION('center_axis',(0.,0.,1.));
#9923=DIRECTION('ref_axis',(1.,0.,0.));
#9924=DIRECTION('',(0.,0.,-1.));
#9925=DIRECTION('center_axis',(0.,0.,1.));
#9926=DIRECTION('ref_axis',(1.,0.,0.));
#9927=DIRECTION('',(0.,0.,-1.));
#9928=DIRECTION('center_axis',(0.,0.,1.));
#9929=DIRECTION('ref_axis',(1.,0.,0.));
#9930=DIRECTION('',(0.,0.,-1.));
#9931=DIRECTION('center_axis',(0.,0.,1.));
#9932=DIRECTION('ref_axis',(1.,0.,0.));
#9933=DIRECTION('',(0.,0.,-1.));
#9934=DIRECTION('center_axis',(0.,0.,1.));
#9935=DIRECTION('ref_axis',(1.,0.,0.));
#9936=DIRECTION('',(0.,0.,-1.));
#9937=DIRECTION('center_axis',(0.,0.,1.));
#9938=DIRECTION('ref_axis',(1.,0.,0.));
#9939=DIRECTION('',(0.,0.,-1.));
#9940=DIRECTION('center_axis',(0.,0.,1.));
#9941=DIRECTION('ref_axis',(1.,0.,0.));
#9942=DIRECTION('',(0.,0.,-1.));
#9943=DIRECTION('center_axis',(0.,0.,1.));
#9944=DIRECTION('ref_axis',(1.,0.,0.));
#9945=DIRECTION('',(0.,0.,-1.));
#9946=DIRECTION('center_axis',(0.,0.,1.));
#9947=DIRECTION('ref_axis',(1.,0.,0.));
#9948=DIRECTION('',(0.,0.,-1.));
#9949=DIRECTION('center_axis',(0.,0.,1.));
#9950=DIRECTION('ref_axis',(1.,0.,0.));
#9951=DIRECTION('',(0.,0.,-1.));
#9952=DIRECTION('center_axis',(0.,0.,1.));
#9953=DIRECTION('ref_axis',(1.,0.,0.));
#9954=DIRECTION('',(0.,0.,-1.));
#9955=DIRECTION('center_axis',(0.,0.,1.));
#9956=DIRECTION('ref_axis',(1.,0.,0.));
#9957=DIRECTION('',(0.,0.,-1.));
#9958=DIRECTION('center_axis',(0.,0.,1.));
#9959=DIRECTION('ref_axis',(1.,0.,0.));
#9960=DIRECTION('',(0.,0.,-1.));
#9961=DIRECTION('center_axis',(0.,0.,1.));
#9962=DIRECTION('ref_axis',(1.,0.,0.));
#9963=DIRECTION('',(0.,0.,-1.));
#9964=DIRECTION('center_axis',(0.,0.,1.));
#9965=DIRECTION('ref_axis',(1.,0.,0.));
#9966=DIRECTION('',(0.,0.,-1.));
#9967=DIRECTION('center_axis',(0.,0.,1.));
#9968=DIRECTION('ref_axis',(1.,0.,0.));
#9969=DIRECTION('',(0.,0.,-1.));
#9970=DIRECTION('center_axis',(0.,0.,1.));
#9971=DIRECTION('ref_axis',(1.,0.,0.));
#9972=DIRECTION('',(0.,0.,-1.));
#9973=DIRECTION('center_axis',(0.,0.,1.));
#9974=DIRECTION('ref_axis',(1.,0.,0.));
#9975=DIRECTION('',(0.,0.,-1.));
#9976=DIRECTION('center_axis',(0.,0.,1.));
#9977=DIRECTION('ref_axis',(1.,0.,0.));
#9978=DIRECTION('',(0.,0.,-1.));
#9979=DIRECTION('center_axis',(0.,0.,1.));
#9980=DIRECTION('ref_axis',(1.,0.,0.));
#9981=DIRECTION('',(0.,0.,-1.));
#9982=DIRECTION('center_axis',(0.,0.,1.));
#9983=DIRECTION('ref_axis',(1.,0.,0.));
#9984=DIRECTION('',(0.,0.,-1.));
#9985=DIRECTION('center_axis',(0.,0.,1.));
#9986=DIRECTION('ref_axis',(1.,0.,0.));
#9987=DIRECTION('',(0.,0.,-1.));
#9988=DIRECTION('center_axis',(0.,0.,1.));
#9989=DIRECTION('ref_axis',(1.,0.,0.));
#9990=DIRECTION('',(0.,0.,-1.));
#9991=DIRECTION('center_axis',(0.,0.,1.));
#9992=DIRECTION('ref_axis',(1.,0.,0.));
#9993=DIRECTION('',(0.,0.,-1.));
#9994=DIRECTION('center_axis',(0.,0.,1.));
#9995=DIRECTION('ref_axis',(1.,0.,0.));
#9996=DIRECTION('',(0.,0.,-1.));
#9997=DIRECTION('center_axis',(0.,0.,1.));
#9998=DIRECTION('ref_axis',(1.,0.,0.));
#9999=DIRECTION('',(0.,0.,-1.));
#10000=DIRECTION('center_axis',(0.,0.,1.));
#10001=DIRECTION('ref_axis',(1.,0.,0.));
#10002=DIRECTION('',(0.,0.,-1.));
#10003=DIRECTION('center_axis',(0.,0.,1.));
#10004=DIRECTION('ref_axis',(1.,0.,0.));
#10005=DIRECTION('',(0.,0.,-1.));
#10006=DIRECTION('center_axis',(0.,0.,1.));
#10007=DIRECTION('ref_axis',(1.,0.,0.));
#10008=DIRECTION('',(0.,0.,-1.));
#10009=DIRECTION('center_axis',(0.,0.,1.));
#10010=DIRECTION('ref_axis',(1.,0.,0.));
#10011=DIRECTION('',(0.,0.,-1.));
#10012=DIRECTION('center_axis',(0.,0.,1.));
#10013=DIRECTION('ref_axis',(1.,0.,0.));
#10014=DIRECTION('',(0.,0.,-1.));
#10015=DIRECTION('center_axis',(0.,0.,1.));
#10016=DIRECTION('ref_axis',(1.,0.,0.));
#10017=DIRECTION('',(0.,0.,-1.));
#10018=DIRECTION('center_axis',(0.,0.,1.));
#10019=DIRECTION('ref_axis',(1.,0.,0.));
#10020=DIRECTION('',(0.,0.,-1.));
#10021=DIRECTION('center_axis',(0.,0.,1.));
#10022=DIRECTION('ref_axis',(1.,0.,0.));
#10023=DIRECTION('',(0.,0.,-1.));
#10024=DIRECTION('center_axis',(0.,0.,1.));
#10025=DIRECTION('ref_axis',(1.,0.,0.));
#10026=DIRECTION('',(0.,0.,-1.));
#10027=DIRECTION('center_axis',(0.,0.,1.));
#10028=DIRECTION('ref_axis',(1.,0.,0.));
#10029=DIRECTION('',(0.,0.,-1.));
#10030=DIRECTION('center_axis',(0.,0.,1.));
#10031=DIRECTION('ref_axis',(1.,0.,0.));
#10032=DIRECTION('',(0.,0.,-1.));
#10033=DIRECTION('center_axis',(0.,0.,1.));
#10034=DIRECTION('ref_axis',(1.,0.,0.));
#10035=DIRECTION('',(0.,0.,-1.));
#10036=DIRECTION('center_axis',(0.,0.,1.));
#10037=DIRECTION('ref_axis',(1.,0.,0.));
#10038=DIRECTION('',(0.,0.,-1.));
#10039=DIRECTION('center_axis',(0.,0.,1.));
#10040=DIRECTION('ref_axis',(1.,0.,0.));
#10041=DIRECTION('',(0.,0.,-1.));
#10042=DIRECTION('center_axis',(0.,0.,1.));
#10043=DIRECTION('ref_axis',(1.,0.,0.));
#10044=DIRECTION('',(0.,0.,-1.));
#10045=DIRECTION('center_axis',(0.,0.,1.));
#10046=DIRECTION('ref_axis',(1.,0.,0.));
#10047=DIRECTION('',(0.,0.,-1.));
#10048=DIRECTION('center_axis',(0.,0.,1.));
#10049=DIRECTION('ref_axis',(1.,0.,0.));
#10050=DIRECTION('',(0.,0.,-1.));
#10051=DIRECTION('center_axis',(0.,0.,1.));
#10052=DIRECTION('ref_axis',(1.,0.,0.));
#10053=DIRECTION('',(0.,0.,-1.));
#10054=DIRECTION('center_axis',(0.,0.,1.));
#10055=DIRECTION('ref_axis',(1.,0.,0.));
#10056=DIRECTION('',(0.,0.,-1.));
#10057=DIRECTION('center_axis',(0.,0.,1.));
#10058=DIRECTION('ref_axis',(1.,0.,0.));
#10059=DIRECTION('',(0.,0.,-1.));
#10060=DIRECTION('center_axis',(0.,0.,1.));
#10061=DIRECTION('ref_axis',(1.,0.,0.));
#10062=DIRECTION('',(0.,0.,-1.));
#10063=DIRECTION('center_axis',(0.,0.,1.));
#10064=DIRECTION('ref_axis',(1.,0.,0.));
#10065=DIRECTION('',(0.,0.,-1.));
#10066=DIRECTION('center_axis',(0.,0.,1.));
#10067=DIRECTION('ref_axis',(1.,0.,0.));
#10068=DIRECTION('',(0.,0.,-1.));
#10069=DIRECTION('center_axis',(0.,0.,1.));
#10070=DIRECTION('ref_axis',(1.,0.,0.));
#10071=DIRECTION('',(0.,0.,-1.));
#10072=DIRECTION('center_axis',(0.,0.,1.));
#10073=DIRECTION('ref_axis',(1.,0.,0.));
#10074=DIRECTION('',(0.,0.,-1.));
#10075=DIRECTION('center_axis',(0.,0.,1.));
#10076=DIRECTION('ref_axis',(1.,0.,0.));
#10077=DIRECTION('',(0.,0.,-1.));
#10078=DIRECTION('center_axis',(0.,0.,1.));
#10079=DIRECTION('ref_axis',(1.,0.,0.));
#10080=DIRECTION('',(0.,0.,-1.));
#10081=DIRECTION('center_axis',(0.,0.,1.));
#10082=DIRECTION('ref_axis',(1.,0.,0.));
#10083=DIRECTION('',(0.,0.,-1.));
#10084=DIRECTION('center_axis',(0.,0.,1.));
#10085=DIRECTION('ref_axis',(1.,0.,0.));
#10086=DIRECTION('',(0.,0.,-1.));
#10087=DIRECTION('center_axis',(0.,0.,1.));
#10088=DIRECTION('ref_axis',(-0.457993717575288,-0.888955428951063,0.));
#10089=DIRECTION('',(0.,0.,1.));
#10090=DIRECTION('center_axis',(0.,0.,1.));
#10091=DIRECTION('ref_axis',(1.,-1.75643374117547E-12,0.));
#10092=DIRECTION('center_axis',(0.,0.,1.));
#10093=DIRECTION('ref_axis',(1.,-1.75643374117547E-12,0.));
#10094=DIRECTION('',(0.,0.,1.));
#10095=DIRECTION('center_axis',(0.,0.,1.));
#10096=DIRECTION('ref_axis',(1.,-1.75643374117547E-12,0.));
#10097=DIRECTION('',(0.,0.,1.));
#10098=DIRECTION('center_axis',(0.,0.,1.));
#10099=DIRECTION('ref_axis',(1.,-1.75643374117547E-12,0.));
#10100=DIRECTION('',(0.,0.,1.));
#10101=DIRECTION('center_axis',(0.,0.,1.));
#10102=DIRECTION('ref_axis',(1.,-1.75643374117547E-12,0.));
#10103=DIRECTION('',(0.,0.,1.));
#10104=DIRECTION('center_axis',(0.,0.,1.));
#10105=DIRECTION('ref_axis',(1.,-1.75643374117547E-12,0.));
#10106=DIRECTION('',(0.,0.,1.));
#10107=DIRECTION('center_axis',(0.,0.,1.));
#10108=DIRECTION('ref_axis',(1.,-1.75643374117547E-12,0.));
#10109=DIRECTION('',(0.,0.,1.));
#10110=DIRECTION('center_axis',(0.,0.,1.));
#10111=DIRECTION('ref_axis',(1.,-1.75643374117547E-12,0.));
#10112=DIRECTION('',(0.,0.,1.));
#10113=DIRECTION('center_axis',(0.,0.,1.));
#10114=DIRECTION('ref_axis',(1.,-1.75643374117547E-12,0.));
#10115=DIRECTION('',(0.,0.,1.));
#10116=DIRECTION('center_axis',(0.,0.,1.));
#10117=DIRECTION('ref_axis',(1.,-1.75643374117547E-12,0.));
#10118=DIRECTION('',(0.,0.,1.));
#10119=DIRECTION('center_axis',(0.,0.,1.));
#10120=DIRECTION('ref_axis',(1.,-1.75643374117547E-12,0.));
#10121=DIRECTION('',(0.,0.,1.));
#10122=DIRECTION('center_axis',(0.,0.,1.));
#10123=DIRECTION('ref_axis',(1.,-1.75643374117547E-12,0.));
#10124=DIRECTION('',(0.,0.,1.));
#10125=DIRECTION('center_axis',(0.,0.,1.));
#10126=DIRECTION('ref_axis',(1.,-1.75643374117547E-12,0.));
#10127=DIRECTION('',(0.,0.,1.));
#10128=DIRECTION('center_axis',(0.,0.,1.));
#10129=DIRECTION('ref_axis',(1.,-1.75643374117547E-12,0.));
#10130=DIRECTION('',(0.,0.,1.));
#10131=DIRECTION('center_axis',(0.,0.,1.));
#10132=DIRECTION('ref_axis',(1.,-1.75643374117547E-12,0.));
#10133=DIRECTION('',(0.,0.,1.));
#10134=DIRECTION('center_axis',(0.,0.,1.));
#10135=DIRECTION('ref_axis',(1.,-1.75643374117547E-12,0.));
#10136=DIRECTION('',(0.,0.,1.));
#10137=DIRECTION('center_axis',(0.,0.,1.));
#10138=DIRECTION('ref_axis',(1.,-1.75643374117547E-12,0.));
#10139=DIRECTION('',(0.,0.,1.));
#10140=DIRECTION('center_axis',(0.,0.,1.));
#10141=DIRECTION('ref_axis',(1.,-1.75643374117547E-12,0.));
#10142=DIRECTION('',(0.,0.,1.));
#10143=DIRECTION('center_axis',(0.,0.,1.));
#10144=DIRECTION('ref_axis',(1.,-1.75643374117547E-12,0.));
#10145=DIRECTION('',(0.,0.,1.));
#10146=DIRECTION('center_axis',(0.,0.,1.));
#10147=DIRECTION('ref_axis',(1.,-1.75643374117547E-12,0.));
#10148=DIRECTION('',(0.,0.,1.));
#10149=DIRECTION('center_axis',(0.,0.,1.));
#10150=DIRECTION('ref_axis',(1.,-1.75643374117547E-12,0.));
#10151=DIRECTION('',(0.,0.,1.));
#10152=DIRECTION('center_axis',(0.,0.,1.));
#10153=DIRECTION('ref_axis',(1.,-1.75643374117547E-12,0.));
#10154=DIRECTION('',(0.,0.,1.));
#10155=DIRECTION('center_axis',(0.,0.,1.));
#10156=DIRECTION('ref_axis',(1.,-1.75643374117547E-12,0.));
#10157=DIRECTION('',(0.,0.,1.));
#10158=DIRECTION('center_axis',(0.,0.,1.));
#10159=DIRECTION('ref_axis',(1.,-1.75643374117547E-12,0.));
#10160=DIRECTION('',(0.,0.,1.));
#10161=DIRECTION('center_axis',(0.,0.,1.));
#10162=DIRECTION('ref_axis',(1.,-1.75643374117547E-12,0.));
#10163=DIRECTION('',(0.,0.,1.));
#10164=DIRECTION('center_axis',(0.,0.,1.));
#10165=DIRECTION('ref_axis',(1.,-1.75643374117547E-12,0.));
#10166=DIRECTION('',(0.,0.,1.));
#10167=DIRECTION('center_axis',(0.,0.,1.));
#10168=DIRECTION('ref_axis',(1.,-1.75643374117547E-12,0.));
#10169=DIRECTION('',(0.,0.,1.));
#10170=DIRECTION('center_axis',(0.,0.,1.));
#10171=DIRECTION('ref_axis',(1.,-1.75643374117547E-12,0.));
#10172=DIRECTION('',(0.,0.,1.));
#10173=DIRECTION('center_axis',(0.,0.,1.));
#10174=DIRECTION('ref_axis',(1.,-1.75643374117547E-12,0.));
#10175=DIRECTION('',(0.,0.,1.));
#10176=DIRECTION('center_axis',(0.,0.,1.));
#10177=DIRECTION('ref_axis',(1.,-1.75643374117547E-12,0.));
#10178=DIRECTION('',(0.,0.,1.));
#10179=DIRECTION('center_axis',(0.,0.,1.));
#10180=DIRECTION('ref_axis',(1.,-1.75643374117547E-12,0.));
#10181=DIRECTION('',(0.,0.,1.));
#10182=DIRECTION('center_axis',(0.,0.,1.));
#10183=DIRECTION('ref_axis',(1.,-1.75643374117547E-12,0.));
#10184=DIRECTION('',(0.,0.,1.));
#10185=DIRECTION('center_axis',(0.,0.,1.));
#10186=DIRECTION('ref_axis',(1.,-1.75643374117547E-12,0.));
#10187=DIRECTION('',(0.,0.,1.));
#10188=DIRECTION('center_axis',(0.,0.,1.));
#10189=DIRECTION('ref_axis',(1.,-1.75643374117547E-12,0.));
#10190=DIRECTION('',(0.,0.,1.));
#10191=DIRECTION('center_axis',(0.,0.,1.));
#10192=DIRECTION('ref_axis',(1.,-1.75643374117547E-12,0.));
#10193=DIRECTION('',(0.,0.,1.));
#10194=DIRECTION('center_axis',(0.,0.,1.));
#10195=DIRECTION('ref_axis',(1.,-1.75643374117547E-12,0.));
#10196=DIRECTION('',(0.,0.,1.));
#10197=DIRECTION('center_axis',(0.,0.,1.));
#10198=DIRECTION('ref_axis',(1.,-1.75643374117547E-12,0.));
#10199=DIRECTION('',(0.,0.,1.));
#10200=DIRECTION('center_axis',(0.,0.,1.));
#10201=DIRECTION('ref_axis',(1.,-1.75643374117547E-12,0.));
#10202=DIRECTION('',(0.,0.,1.));
#10203=DIRECTION('center_axis',(0.,0.,1.));
#10204=DIRECTION('ref_axis',(1.,-1.75643374117547E-12,0.));
#10205=DIRECTION('',(0.,0.,1.));
#10206=DIRECTION('center_axis',(0.,0.,1.));
#10207=DIRECTION('ref_axis',(1.,-1.75643374117547E-12,0.));
#10208=DIRECTION('',(0.,0.,1.));
#10209=DIRECTION('center_axis',(0.,0.,1.));
#10210=DIRECTION('ref_axis',(1.,-1.75643374117547E-12,0.));
#10211=DIRECTION('',(0.,0.,1.));
#10212=DIRECTION('center_axis',(0.,0.,1.));
#10213=DIRECTION('ref_axis',(1.,-1.75643374117547E-12,0.));
#10214=DIRECTION('',(0.,0.,1.));
#10215=DIRECTION('center_axis',(0.,0.,1.));
#10216=DIRECTION('ref_axis',(1.,-1.75643374117547E-12,0.));
#10217=DIRECTION('',(0.,0.,1.));
#10218=DIRECTION('center_axis',(0.,0.,1.));
#10219=DIRECTION('ref_axis',(1.,-1.75643374117547E-12,0.));
#10220=DIRECTION('',(0.,0.,1.));
#10221=DIRECTION('center_axis',(0.,0.,1.));
#10222=DIRECTION('ref_axis',(1.,-1.75643374117547E-12,0.));
#10223=DIRECTION('',(0.,0.,1.));
#10224=DIRECTION('center_axis',(0.,0.,1.));
#10225=DIRECTION('ref_axis',(1.,-1.75643374117547E-12,0.));
#10226=DIRECTION('',(0.,0.,1.));
#10227=DIRECTION('center_axis',(0.,0.,1.));
#10228=DIRECTION('ref_axis',(1.,-1.75643374117547E-12,0.));
#10229=DIRECTION('',(0.,0.,1.));
#10230=DIRECTION('center_axis',(0.,0.,1.));
#10231=DIRECTION('ref_axis',(1.,-1.75643374117547E-12,0.));
#10232=DIRECTION('',(0.,0.,1.));
#10233=DIRECTION('center_axis',(0.,0.,1.));
#10234=DIRECTION('ref_axis',(1.,-1.75643374117547E-12,0.));
#10235=DIRECTION('',(0.,0.,1.));
#10236=DIRECTION('center_axis',(0.,0.,1.));
#10237=DIRECTION('ref_axis',(1.,-1.75643374117547E-12,0.));
#10238=DIRECTION('',(0.,0.,1.));
#10239=DIRECTION('center_axis',(0.,0.,1.));
#10240=DIRECTION('ref_axis',(1.,-1.75643374117547E-12,0.));
#10241=DIRECTION('',(0.,0.,1.));
#10242=DIRECTION('center_axis',(0.,0.,1.));
#10243=DIRECTION('ref_axis',(1.,-1.75643374117547E-12,0.));
#10244=DIRECTION('',(0.,0.,1.));
#10245=DIRECTION('center_axis',(0.,0.,1.));
#10246=DIRECTION('ref_axis',(1.,-1.75643374117547E-12,0.));
#10247=DIRECTION('',(0.,0.,1.));
#10248=DIRECTION('center_axis',(0.,0.,1.));
#10249=DIRECTION('ref_axis',(1.,-1.75643374117547E-12,0.));
#10250=DIRECTION('',(0.,0.,1.));
#10251=DIRECTION('center_axis',(0.,0.,1.));
#10252=DIRECTION('ref_axis',(1.,-1.75643374117547E-12,0.));
#10253=DIRECTION('',(0.,0.,1.));
#10254=DIRECTION('center_axis',(0.,0.,1.));
#10255=DIRECTION('ref_axis',(1.,-1.75643374117547E-12,0.));
#10256=DIRECTION('',(0.,0.,1.));
#10257=DIRECTION('center_axis',(0.,0.,1.));
#10258=DIRECTION('ref_axis',(1.,-1.75643374117547E-12,0.));
#10259=DIRECTION('',(0.,0.,1.));
#10260=DIRECTION('center_axis',(0.,0.,1.));
#10261=DIRECTION('ref_axis',(1.,-1.75643374117547E-12,0.));
#10262=DIRECTION('',(0.,0.,1.));
#10263=DIRECTION('center_axis',(0.,0.,1.));
#10264=DIRECTION('ref_axis',(1.,-1.75643374117547E-12,0.));
#10265=DIRECTION('',(0.,0.,1.));
#10266=DIRECTION('center_axis',(0.,0.,1.));
#10267=DIRECTION('ref_axis',(1.,-1.75643374117547E-12,0.));
#10268=DIRECTION('',(0.,0.,1.));
#10269=DIRECTION('center_axis',(0.,0.,1.));
#10270=DIRECTION('ref_axis',(1.,-1.75643374117547E-12,0.));
#10271=DIRECTION('',(0.,0.,1.));
#10272=DIRECTION('center_axis',(0.,0.,1.));
#10273=DIRECTION('ref_axis',(1.,-1.75643374117547E-12,0.));
#10274=DIRECTION('',(0.,0.,1.));
#10275=DIRECTION('center_axis',(0.,0.,1.));
#10276=DIRECTION('ref_axis',(1.,-1.75643374117547E-12,0.));
#10277=DIRECTION('',(0.,0.,1.));
#10278=DIRECTION('center_axis',(0.,0.,1.));
#10279=DIRECTION('ref_axis',(1.,-1.75643374117547E-12,0.));
#10280=DIRECTION('',(0.,0.,1.));
#10281=DIRECTION('center_axis',(0.,0.,1.));
#10282=DIRECTION('ref_axis',(1.,-1.75643374117547E-12,0.));
#10283=DIRECTION('',(0.,0.,1.));
#10284=DIRECTION('center_axis',(0.,0.,1.));
#10285=DIRECTION('ref_axis',(1.,-1.75643374117547E-12,0.));
#10286=DIRECTION('',(0.,0.,1.));
#10287=DIRECTION('center_axis',(0.,0.,1.));
#10288=DIRECTION('ref_axis',(1.,-1.75643374117547E-12,0.));
#10289=DIRECTION('',(0.,0.,1.));
#10290=DIRECTION('center_axis',(0.,0.,1.));
#10291=DIRECTION('ref_axis',(1.,-1.75643374117547E-12,0.));
#10292=DIRECTION('',(0.,0.,1.));
#10293=DIRECTION('center_axis',(0.,0.,1.));
#10294=DIRECTION('ref_axis',(1.,-1.75643374117547E-12,0.));
#10295=DIRECTION('',(0.,0.,1.));
#10296=DIRECTION('center_axis',(0.,0.,1.));
#10297=DIRECTION('ref_axis',(1.,-1.75643374117547E-12,0.));
#10298=DIRECTION('',(0.,0.,1.));
#10299=DIRECTION('center_axis',(0.,0.,1.));
#10300=DIRECTION('ref_axis',(1.,-1.75643374117547E-12,0.));
#10301=DIRECTION('',(0.,0.,1.));
#10302=DIRECTION('center_axis',(0.,0.,1.));
#10303=DIRECTION('ref_axis',(1.,-1.75643374117547E-12,0.));
#10304=DIRECTION('',(0.,0.,1.));
#10305=DIRECTION('center_axis',(0.,0.,1.));
#10306=DIRECTION('ref_axis',(1.,-1.75643374117547E-12,0.));
#10307=DIRECTION('',(0.,0.,1.));
#10308=DIRECTION('center_axis',(0.,0.,1.));
#10309=DIRECTION('ref_axis',(1.,-1.75643374117547E-12,0.));
#10310=DIRECTION('',(0.,0.,1.));
#10311=DIRECTION('center_axis',(0.,0.,1.));
#10312=DIRECTION('ref_axis',(1.,-1.75643374117547E-12,0.));
#10313=DIRECTION('',(0.,0.,1.));
#10314=DIRECTION('center_axis',(0.,0.,1.));
#10315=DIRECTION('ref_axis',(1.,-1.75643374117547E-12,0.));
#10316=DIRECTION('',(0.,0.,1.));
#10317=DIRECTION('center_axis',(0.,0.,1.));
#10318=DIRECTION('ref_axis',(1.,-1.75643374117547E-12,0.));
#10319=DIRECTION('',(0.,0.,1.));
#10320=DIRECTION('center_axis',(0.,0.,1.));
#10321=DIRECTION('ref_axis',(1.,-1.75643374117547E-12,0.));
#10322=DIRECTION('',(0.,0.,1.));
#10323=DIRECTION('center_axis',(0.,0.,1.));
#10324=DIRECTION('ref_axis',(1.,-1.75643374117547E-12,0.));
#10325=DIRECTION('',(0.,0.,1.));
#10326=DIRECTION('center_axis',(0.,0.,1.));
#10327=DIRECTION('ref_axis',(1.,-1.75643374117547E-12,0.));
#10328=DIRECTION('',(0.,0.,1.));
#10329=DIRECTION('center_axis',(0.,0.,1.));
#10330=DIRECTION('ref_axis',(1.,-1.75643374117547E-12,0.));
#10331=DIRECTION('',(0.,0.,1.));
#10332=DIRECTION('center_axis',(0.,0.,1.));
#10333=DIRECTION('ref_axis',(1.,-1.75643374117547E-12,0.));
#10334=DIRECTION('',(0.,0.,1.));
#10335=DIRECTION('center_axis',(0.,0.,1.));
#10336=DIRECTION('ref_axis',(1.,-1.75643374117547E-12,0.));
#10337=DIRECTION('',(0.,0.,1.));
#10338=DIRECTION('center_axis',(0.,0.,1.));
#10339=DIRECTION('ref_axis',(1.,-1.75643374117547E-12,0.));
#10340=DIRECTION('',(0.,0.,1.));
#10341=DIRECTION('center_axis',(0.,0.,1.));
#10342=DIRECTION('ref_axis',(1.,-1.75643374117547E-12,0.));
#10343=DIRECTION('',(0.,0.,1.));
#10344=DIRECTION('center_axis',(0.,0.,1.));
#10345=DIRECTION('ref_axis',(1.,-1.75643374117547E-12,0.));
#10346=DIRECTION('',(0.,0.,1.));
#10347=DIRECTION('center_axis',(0.,0.,1.));
#10348=DIRECTION('ref_axis',(1.,-1.75643374117547E-12,0.));
#10349=DIRECTION('',(0.,0.,1.));
#10350=DIRECTION('center_axis',(0.,0.,1.));
#10351=DIRECTION('ref_axis',(1.,-1.75643374117547E-12,0.));
#10352=DIRECTION('',(0.,0.,1.));
#10353=DIRECTION('center_axis',(0.,0.,1.));
#10354=DIRECTION('ref_axis',(1.,-1.75643374117547E-12,0.));
#10355=DIRECTION('',(0.,0.,1.));
#10356=DIRECTION('center_axis',(0.,0.,1.));
#10357=DIRECTION('ref_axis',(1.,-1.75643374117547E-12,0.));
#10358=DIRECTION('',(0.,0.,1.));
#10359=DIRECTION('center_axis',(0.,0.,1.));
#10360=DIRECTION('ref_axis',(1.,-1.75643374117547E-12,0.));
#10361=DIRECTION('',(0.,0.,1.));
#10362=DIRECTION('center_axis',(0.,0.,1.));
#10363=DIRECTION('ref_axis',(1.,-1.75643374117547E-12,0.));
#10364=DIRECTION('',(0.,0.,1.));
#10365=DIRECTION('center_axis',(0.,0.,1.));
#10366=DIRECTION('ref_axis',(1.,-1.75643374117547E-12,0.));
#10367=DIRECTION('',(0.,0.,1.));
#10368=DIRECTION('center_axis',(0.,0.,1.));
#10369=DIRECTION('ref_axis',(1.,-1.75643374117547E-12,0.));
#10370=DIRECTION('',(0.,0.,1.));
#10371=DIRECTION('center_axis',(0.,0.,1.));
#10372=DIRECTION('ref_axis',(1.,0.,0.));
#10373=DIRECTION('center_axis',(0.,0.,1.));
#10374=DIRECTION('ref_axis',(1.,0.,0.));
#10375=DIRECTION('',(0.,0.,1.));
#10376=DIRECTION('center_axis',(0.,0.,-1.));
#10377=DIRECTION('ref_axis',(1.,0.,0.));
#10378=DIRECTION('center_axis',(0.,0.,1.));
#10379=DIRECTION('ref_axis',(1.,0.,0.));
#10380=DIRECTION('center_axis',(0.,0.,1.));
#10381=DIRECTION('ref_axis',(1.,0.,0.));
#10382=DIRECTION('',(0.,0.,1.));
#10383=DIRECTION('center_axis',(0.,0.,-1.));
#10384=DIRECTION('ref_axis',(1.,0.,0.));
#10385=DIRECTION('center_axis',(0.,0.,1.));
#10386=DIRECTION('ref_axis',(1.,0.,0.));
#10387=DIRECTION('center_axis',(0.,0.,1.));
#10388=DIRECTION('ref_axis',(1.,0.,0.));
#10389=DIRECTION('',(0.,0.,1.));
#10390=DIRECTION('center_axis',(0.,0.,-1.));
#10391=DIRECTION('ref_axis',(1.,0.,0.));
#10392=DIRECTION('center_axis',(0.,0.,1.));
#10393=DIRECTION('ref_axis',(1.,0.,0.));
#10394=DIRECTION('center_axis',(0.,0.,1.));
#10395=DIRECTION('ref_axis',(1.,0.,0.));
#10396=DIRECTION('',(0.,0.,1.));
#10397=DIRECTION('center_axis',(0.,0.,-1.));
#10398=DIRECTION('ref_axis',(1.,0.,0.));
#10399=DIRECTION('center_axis',(0.,0.,1.));
#10400=DIRECTION('ref_axis',(1.,0.,0.));
#10401=DIRECTION('center_axis',(0.,0.,1.));
#10402=DIRECTION('ref_axis',(1.,0.,0.));
#10403=DIRECTION('',(0.,0.,1.));
#10404=DIRECTION('center_axis',(0.,0.,-1.));
#10405=DIRECTION('ref_axis',(1.,0.,0.));
#10406=DIRECTION('center_axis',(0.,0.,1.));
#10407=DIRECTION('ref_axis',(1.,0.,0.));
#10408=DIRECTION('center_axis',(0.,0.,1.));
#10409=DIRECTION('ref_axis',(1.,0.,0.));
#10410=DIRECTION('',(0.,0.,1.));
#10411=DIRECTION('center_axis',(0.,0.,-1.));
#10412=DIRECTION('ref_axis',(1.,0.,0.));
#10413=DIRECTION('center_axis',(0.,0.,1.));
#10414=DIRECTION('ref_axis',(1.,0.,0.));
#10415=DIRECTION('center_axis',(0.,0.,1.));
#10416=DIRECTION('ref_axis',(1.,0.,0.));
#10417=DIRECTION('center_axis',(0.,0.,-1.));
#10418=DIRECTION('ref_axis',(1.,-1.75643374117547E-12,0.));
#10419=DIRECTION('center_axis',(0.,0.,1.));
#10420=DIRECTION('ref_axis',(1.,0.,0.));
#10421=DIRECTION('',(0.,0.,-1.));
#10422=DIRECTION('center_axis',(0.,0.,1.));
#10423=DIRECTION('ref_axis',(1.,0.,0.));
#10424=DIRECTION('center_axis',(0.,0.,1.));
#10425=DIRECTION('ref_axis',(1.,0.,0.));
#10426=DIRECTION('center_axis',(0.,0.,1.));
#10427=DIRECTION('ref_axis',(1.,-1.75643374117547E-12,0.));
#10428=DIRECTION('center_axis',(0.,0.,1.));
#10429=DIRECTION('ref_axis',(1.,0.,0.));
#10430=DIRECTION('center_axis',(0.,0.,-1.));
#10431=DIRECTION('ref_axis',(1.,0.,0.));
#10432=DIRECTION('center_axis',(0.,0.,1.));
#10433=DIRECTION('ref_axis',(1.,0.,0.));
#10434=DIRECTION('axis',(0.,0.,1.));
#10435=DIRECTION('refdir',(1.,0.,0.));
#10436=DIRECTION('center_axis',(0.,0.,1.));
#10437=DIRECTION('ref_axis',(1.,0.,0.));
#10438=DIRECTION('center_axis',(0.,0.,1.));
#10439=DIRECTION('ref_axis',(1.,0.,0.));
#10440=DIRECTION('',(0.,0.,-1.));
#10441=DIRECTION('center_axis',(0.,0.,1.));
#10442=DIRECTION('ref_axis',(1.,0.,0.));
#10443=DIRECTION('center_axis',(0.,0.,1.));
#10444=DIRECTION('ref_axis',(1.,0.,0.));
#10445=DIRECTION('center_axis',(0.,0.,1.));
#10446=DIRECTION('ref_axis',(1.,0.,0.));
#10447=DIRECTION('axis',(0.,0.,1.));
#10448=DIRECTION('refdir',(1.,0.,0.));
#10449=DIRECTION('center_axis',(0.,0.,1.));
#10450=DIRECTION('ref_axis',(1.,0.,0.));
#10451=DIRECTION('center_axis',(0.,0.,1.));
#10452=DIRECTION('ref_axis',(1.,0.,0.));
#10453=DIRECTION('',(0.,0.,-1.));
#10454=DIRECTION('center_axis',(0.,0.,1.));
#10455=DIRECTION('ref_axis',(1.,0.,0.));
#10456=DIRECTION('center_axis',(0.,0.,1.));
#10457=DIRECTION('ref_axis',(1.,0.,0.));
#10458=DIRECTION('center_axis',(0.,0.,1.));
#10459=DIRECTION('ref_axis',(1.,0.,0.));
#10460=DIRECTION('axis',(0.,0.,1.));
#10461=DIRECTION('refdir',(1.,0.,0.));
#10462=DIRECTION('center_axis',(0.,1.,0.));
#10463=DIRECTION('ref_axis',(1.,0.,0.));
#10464=DIRECTION('center_axis',(0.,1.,0.));
#10465=DIRECTION('ref_axis',(1.,0.,0.));
#10466=DIRECTION('',(0.,-1.,0.));
#10467=DIRECTION('center_axis',(0.,-1.,0.));
#10468=DIRECTION('ref_axis',(1.,0.,0.));
#10469=DIRECTION('',(0.,1.,0.));
#10470=DIRECTION('center_axis',(0.,1.,0.));
#10471=DIRECTION('ref_axis',(1.,0.,0.));
#10472=DIRECTION('',(1.,0.,0.));
#10473=DIRECTION('center_axis',(0.,1.,0.));
#10474=DIRECTION('ref_axis',(1.,0.,0.));
#10475=DIRECTION('',(0.,0.,1.));
#10476=DIRECTION('',(-1.,0.,0.));
#10477=DIRECTION('',(0.,0.,-1.));
#10478=DIRECTION('center_axis',(0.,1.,0.));
#10479=DIRECTION('ref_axis',(1.,0.,0.));
#10480=DIRECTION('',(1.,0.,0.));
#10481=DIRECTION('center_axis',(0.,0.,-1.));
#10482=DIRECTION('ref_axis',(-1.,0.,0.));
#10483=DIRECTION('',(-1.,0.,0.));
#10484=DIRECTION('',(0.,-1.,0.));
#10485=DIRECTION('center_axis',(0.,0.,1.));
#10486=DIRECTION('ref_axis',(1.,0.,0.));
#10487=DIRECTION('center_axis',(0.,0.,1.));
#10488=DIRECTION('ref_axis',(1.,0.,0.));
#10489=DIRECTION('',(0.,0.,1.));
#10490=DIRECTION('center_axis',(0.,0.,-1.));
#10491=DIRECTION('ref_axis',(1.,0.,0.));
#10492=DIRECTION('center_axis',(0.,0.,1.));
#10493=DIRECTION('ref_axis',(-0.447213595499958,-0.894427190999916,0.));
#10494=DIRECTION('',(0.,0.,-1.));
#10495=DIRECTION('center_axis',(0.,0.,1.));
#10496=DIRECTION('ref_axis',(1.,0.,0.));
#10497=DIRECTION('',(0.,0.,1.));
#10498=DIRECTION('center_axis',(0.,0.,1.));
#10499=DIRECTION('ref_axis',(1.,0.,0.));
#10500=DIRECTION('center_axis',(0.,1.,0.));
#10501=DIRECTION('ref_axis',(1.,0.,0.));
#10502=DIRECTION('',(1.,0.,0.));
#10503=DIRECTION('',(0.,0.,-1.));
#10504=DIRECTION('',(-1.,0.,0.));
#10505=DIRECTION('center_axis',(0.,0.,-1.));
#10506=DIRECTION('ref_axis',(-1.,0.,0.));
#10507=DIRECTION('',(0.,1.,0.));
#10508=DIRECTION('',(-1.,0.,0.));
#10509=DIRECTION('',(0.,1.,0.));
#10510=DIRECTION('',(1.,0.,0.));
#10511=DIRECTION('',(0.,1.,0.));
#10512=DIRECTION('center_axis',(-1.,0.,0.));
#10513=DIRECTION('ref_axis',(0.,0.,1.));
#10514=DIRECTION('',(0.,1.,0.));
#10515=DIRECTION('',(0.,0.,1.));
#10516=DIRECTION('center_axis',(0.,1.,0.));
#10517=DIRECTION('ref_axis',(0.,0.,1.));
#10518=DIRECTION('',(1.,0.,0.));
#10519=DIRECTION('',(0.,0.,-1.));
#10520=DIRECTION('center_axis',(0.,0.,1.));
#10521=DIRECTION('ref_axis',(1.,0.,0.));
#10522=DIRECTION('',(0.,1.,0.));
#10523=DIRECTION('',(0.,1.,0.));
#10524=DIRECTION('center_axis',(-1.,0.,0.));
#10525=DIRECTION('ref_axis',(0.,0.,1.));
#10526=DIRECTION('',(0.,0.,-1.));
#10527=DIRECTION('',(0.,-1.,0.));
#10528=DIRECTION('center_axis',(1.,0.,0.));
#10529=DIRECTION('ref_axis',(0.,0.,-1.));
#10530=DIRECTION('',(0.,1.,0.));
#10531=DIRECTION('',(0.,0.,1.));
#10532=DIRECTION('center_axis',(0.,1.,0.));
#10533=DIRECTION('ref_axis',(1.,0.,0.));
#10534=DIRECTION('',(-1.,0.,0.));
#10535=DIRECTION('center_axis',(0.,1.,0.));
#10536=DIRECTION('ref_axis',(1.,0.,0.));
#10537=DIRECTION('center_axis',(0.,1.,0.));
#10538=DIRECTION('ref_axis',(1.,0.,0.));
#10539=DIRECTION('center_axis',(0.,1.,0.));
#10540=DIRECTION('ref_axis',(1.,0.,0.));
#10541=DIRECTION('center_axis',(0.,1.,0.));
#10542=DIRECTION('ref_axis',(1.,0.,0.));
#10543=DIRECTION('',(0.,1.,0.));
#10544=DIRECTION('center_axis',(0.,0.,-1.));
#10545=DIRECTION('ref_axis',(-1.,0.,0.));
#10546=DIRECTION('center_axis',(0.,0.,1.));
#10547=DIRECTION('ref_axis',(1.,0.,0.));
#10548=DIRECTION('center_axis',(0.,0.,1.));
#10549=DIRECTION('ref_axis',(1.,0.,0.));
#10550=DIRECTION('',(0.,0.,1.));
#10551=DIRECTION('center_axis',(0.,0.,-1.));
#10552=DIRECTION('ref_axis',(1.,0.,0.));
#10553=DIRECTION('center_axis',(-1.,0.,0.));
#10554=DIRECTION('ref_axis',(0.,0.,1.));
#10555=DIRECTION('',(0.,0.,-1.));
#10556=DIRECTION('',(0.,1.,0.));
#10557=DIRECTION('',(0.,0.,1.));
#10558=DIRECTION('',(0.,1.,0.));
#10559=DIRECTION('center_axis',(0.,0.,-1.));
#10560=DIRECTION('ref_axis',(-1.,0.,0.));
#10561=DIRECTION('',(1.,0.,0.));
#10562=DIRECTION('',(-1.,0.,0.));
#10563=DIRECTION('',(0.,1.,0.));
#10564=DIRECTION('center_axis',(1.,0.,0.));
#10565=DIRECTION('ref_axis',(0.,0.,-1.));
#10566=DIRECTION('',(0.,0.,1.));
#10567=DIRECTION('',(0.,0.,-1.));
#10568=DIRECTION('',(0.,1.,0.));
#10569=DIRECTION('center_axis',(0.,0.,1.));
#10570=DIRECTION('ref_axis',(1.,0.,0.));
#10571=DIRECTION('',(-1.,0.,0.));
#10572=DIRECTION('',(1.,0.,0.));
#10573=DIRECTION('center_axis',(0.,1.,0.));
#10574=DIRECTION('ref_axis',(0.,0.,1.));
#10575=DIRECTION('center_axis',(0.,1.,0.));
#10576=DIRECTION('ref_axis',(1.,0.,0.));
#10577=DIRECTION('center_axis',(0.,0.,1.));
#10578=DIRECTION('ref_axis',(1.,0.,0.));
#10579=DIRECTION('center_axis',(0.,0.,1.));
#10580=DIRECTION('ref_axis',(1.,0.,0.));
#10581=DIRECTION('',(0.,0.,1.));
#10582=DIRECTION('center_axis',(0.,0.,-1.));
#10583=DIRECTION('ref_axis',(1.,0.,0.));
#10584=DIRECTION('center_axis',(-1.,0.,0.));
#10585=DIRECTION('ref_axis',(0.,0.,1.));
#10586=DIRECTION('',(0.,0.,-1.));
#10587=DIRECTION('',(0.,1.,0.));
#10588=DIRECTION('',(0.,0.,1.));
#10589=DIRECTION('',(0.,1.,0.));
#10590=DIRECTION('center_axis',(0.,0.,-1.));
#10591=DIRECTION('ref_axis',(-1.,0.,0.));
#10592=DIRECTION('',(1.,0.,0.));
#10593=DIRECTION('',(-1.,0.,0.));
#10594=DIRECTION('',(0.,1.,0.));
#10595=DIRECTION('center_axis',(1.,0.,0.));
#10596=DIRECTION('ref_axis',(0.,0.,-1.));
#10597=DIRECTION('',(0.,0.,1.));
#10598=DIRECTION('',(0.,0.,-1.));
#10599=DIRECTION('',(0.,1.,0.));
#10600=DIRECTION('center_axis',(0.,0.,1.));
#10601=DIRECTION('ref_axis',(1.,0.,0.));
#10602=DIRECTION('',(-1.,0.,0.));
#10603=DIRECTION('',(1.,0.,0.));
#10604=DIRECTION('center_axis',(0.,1.,0.));
#10605=DIRECTION('ref_axis',(0.,0.,1.));
#10606=DIRECTION('center_axis',(0.,1.,0.));
#10607=DIRECTION('ref_axis',(1.,0.,0.));
#10608=DIRECTION('axis',(0.,0.,1.));
#10609=DIRECTION('refdir',(1.,0.,0.));
#10610=DIRECTION('center_axis',(0.,1.,0.));
#10611=DIRECTION('ref_axis',(1.,0.,0.));
#10612=DIRECTION('',(0.,-1.,0.));
#10613=DIRECTION('center_axis',(0.,-1.,0.));
#10614=DIRECTION('ref_axis',(1.,0.,0.));
#10615=DIRECTION('',(0.,1.,0.));
#10616=DIRECTION('center_axis',(0.,1.,0.));
#10617=DIRECTION('ref_axis',(1.,0.,0.));
#10618=DIRECTION('center_axis',(0.,1.,0.));
#10619=DIRECTION('ref_axis',(1.,0.,0.));
#10620=DIRECTION('',(-1.,0.,0.));
#10621=DIRECTION('center_axis',(0.,1.,0.));
#10622=DIRECTION('ref_axis',(1.,0.,0.));
#10623=DIRECTION('',(-1.,0.,0.));
#10624=DIRECTION('center_axis',(0.,0.,1.));
#10625=DIRECTION('ref_axis',(1.,0.,0.));
#10626=DIRECTION('',(1.,0.,0.));
#10627=DIRECTION('',(0.,-1.,0.));
#10628=DIRECTION('center_axis',(0.,0.,1.));
#10629=DIRECTION('ref_axis',(1.,0.,0.));
#10630=DIRECTION('',(0.,1.,0.));
#10631=DIRECTION('',(1.,0.,0.));
#10632=DIRECTION('center_axis',(0.,1.,0.));
#10633=DIRECTION('ref_axis',(1.,0.,0.));
#10634=DIRECTION('center_axis',(0.,1.,0.));
#10635=DIRECTION('ref_axis',(1.,0.,0.));
#10636=DIRECTION('center_axis',(0.,1.,0.));
#10637=DIRECTION('ref_axis',(1.,0.,0.));
#10638=DIRECTION('center_axis',(0.,0.,1.));
#10639=DIRECTION('ref_axis',(1.,0.,0.));
#10640=DIRECTION('center_axis',(0.,0.,1.));
#10641=DIRECTION('ref_axis',(1.,0.,0.));
#10642=DIRECTION('',(0.,0.,1.));
#10643=DIRECTION('center_axis',(0.,0.,-1.));
#10644=DIRECTION('ref_axis',(1.,0.,0.));
#10645=DIRECTION('center_axis',(-1.,0.,0.));
#10646=DIRECTION('ref_axis',(0.,0.,1.));
#10647=DIRECTION('',(0.,0.,-1.));
#10648=DIRECTION('',(0.,1.,0.));
#10649=DIRECTION('',(0.,0.,1.));
#10650=DIRECTION('',(0.,1.,0.));
#10651=DIRECTION('center_axis',(0.,0.,-1.));
#10652=DIRECTION('ref_axis',(-1.,0.,0.));
#10653=DIRECTION('',(1.,0.,0.));
#10654=DIRECTION('',(-1.,0.,0.));
#10655=DIRECTION('',(0.,1.,0.));
#10656=DIRECTION('center_axis',(1.,0.,0.));
#10657=DIRECTION('ref_axis',(0.,0.,-1.));
#10658=DIRECTION('',(0.,0.,1.));
#10659=DIRECTION('',(0.,0.,-1.));
#10660=DIRECTION('',(0.,1.,0.));
#10661=DIRECTION('center_axis',(0.,0.,1.));
#10662=DIRECTION('ref_axis',(1.,0.,0.));
#10663=DIRECTION('',(-1.,0.,0.));
#10664=DIRECTION('',(1.,0.,0.));
#10665=DIRECTION('center_axis',(0.,1.,0.));
#10666=DIRECTION('ref_axis',(0.,0.,1.));
#10667=DIRECTION('center_axis',(0.,1.,0.));
#10668=DIRECTION('ref_axis',(1.,0.,0.));
#10669=DIRECTION('center_axis',(0.,0.,1.));
#10670=DIRECTION('ref_axis',(1.,0.,0.));
#10671=DIRECTION('center_axis',(0.,0.,1.));
#10672=DIRECTION('ref_axis',(1.,0.,0.));
#10673=DIRECTION('',(0.,0.,1.));
#10674=DIRECTION('center_axis',(0.,0.,-1.));
#10675=DIRECTION('ref_axis',(1.,0.,0.));
#10676=DIRECTION('center_axis',(-1.,0.,0.));
#10677=DIRECTION('ref_axis',(0.,0.,1.));
#10678=DIRECTION('',(0.,0.,-1.));
#10679=DIRECTION('',(0.,1.,0.));
#10680=DIRECTION('',(0.,0.,1.));
#10681=DIRECTION('',(0.,1.,0.));
#10682=DIRECTION('center_axis',(0.,0.,-1.));
#10683=DIRECTION('ref_axis',(-1.,0.,0.));
#10684=DIRECTION('',(1.,0.,0.));
#10685=DIRECTION('',(-1.,0.,0.));
#10686=DIRECTION('',(0.,1.,0.));
#10687=DIRECTION('center_axis',(1.,0.,0.));
#10688=DIRECTION('ref_axis',(0.,0.,-1.));
#10689=DIRECTION('',(0.,0.,1.));
#10690=DIRECTION('',(0.,0.,-1.));
#10691=DIRECTION('',(0.,1.,0.));
#10692=DIRECTION('center_axis',(0.,0.,1.));
#10693=DIRECTION('ref_axis',(1.,0.,0.));
#10694=DIRECTION('',(-1.,0.,0.));
#10695=DIRECTION('',(1.,0.,0.));
#10696=DIRECTION('center_axis',(0.,1.,0.));
#10697=DIRECTION('ref_axis',(0.,0.,1.));
#10698=DIRECTION('center_axis',(0.,1.,0.));
#10699=DIRECTION('ref_axis',(1.,0.,0.));
#10700=DIRECTION('axis',(0.,0.,1.));
#10701=DIRECTION('refdir',(1.,0.,0.));
#10702=DIRECTION('center_axis',(0.,0.,-1.));
#10703=DIRECTION('ref_axis',(-1.,0.,0.));
#10704=DIRECTION('',(0.,-1.,0.));
#10705=DIRECTION('',(1.,0.,0.));
#10706=DIRECTION('',(0.,1.,0.));
#10707=DIRECTION('',(-1.,0.,0.));
#10708=DIRECTION('center_axis',(0.,0.,-1.));
#10709=DIRECTION('ref_axis',(-1.,0.,0.));
#10710=DIRECTION('',(0.,1.,0.));
#10711=DIRECTION('',(-1.,0.,0.));
#10712=DIRECTION('',(0.,-1.,0.));
#10713=DIRECTION('',(1.,0.,0.));
#10714=DIRECTION('center_axis',(0.,1.,0.));
#10715=DIRECTION('ref_axis',(1.,0.,0.));
#10716=DIRECTION('center_axis',(0.,1.,0.));
#10717=DIRECTION('ref_axis',(1.,0.,0.));
#10718=DIRECTION('center_axis',(0.,-1.,0.));
#10719=DIRECTION('ref_axis',(1.,0.,0.));
#10720=DIRECTION('center_axis',(0.,1.,0.));
#10721=DIRECTION('ref_axis',(1.,0.,0.));
#10722=DIRECTION('center_axis',(0.,-1.,0.));
#10723=DIRECTION('ref_axis',(1.,0.,0.));
#10724=DIRECTION('center_axis',(0.,1.,0.));
#10725=DIRECTION('ref_axis',(1.,0.,0.));
#10726=DIRECTION('center_axis',(0.,1.,0.));
#10727=DIRECTION('ref_axis',(1.,0.,0.));
#10728=DIRECTION('center_axis',(0.,1.,0.));
#10729=DIRECTION('ref_axis',(1.,0.,0.));
#10730=DIRECTION('axis',(0.,0.,1.));
#10731=DIRECTION('refdir',(1.,0.,0.));
#10732=DIRECTION('center_axis',(0.,0.,1.));
#10733=DIRECTION('ref_axis',(1.,0.,0.));
#10734=DIRECTION('',(0.,-1.,0.));
#10735=DIRECTION('',(-1.,0.,0.));
#10736=DIRECTION('',(0.,1.,0.));
#10737=DIRECTION('',(1.,0.,0.));
#10738=DIRECTION('center_axis',(0.,0.,1.));
#10739=DIRECTION('ref_axis',(1.,0.,0.));
#10740=DIRECTION('',(0.,1.,0.));
#10741=DIRECTION('',(1.,0.,0.));
#10742=DIRECTION('',(0.,-1.,0.));
#10743=DIRECTION('',(-1.,0.,0.));
#10744=DIRECTION('center_axis',(0.,1.,0.));
#10745=DIRECTION('ref_axis',(1.,0.,0.));
#10746=DIRECTION('center_axis',(0.,1.,0.));
#10747=DIRECTION('ref_axis',(1.,0.,0.));
#10748=DIRECTION('center_axis',(0.,-1.,0.));
#10749=DIRECTION('ref_axis',(1.,0.,0.));
#10750=DIRECTION('center_axis',(0.,1.,0.));
#10751=DIRECTION('ref_axis',(1.,0.,0.));
#10752=DIRECTION('center_axis',(0.,-1.,0.));
#10753=DIRECTION('ref_axis',(1.,0.,0.));
#10754=DIRECTION('center_axis',(0.,1.,0.));
#10755=DIRECTION('ref_axis',(1.,0.,0.));
#10756=DIRECTION('center_axis',(0.,1.,0.));
#10757=DIRECTION('ref_axis',(1.,0.,0.));
#10758=DIRECTION('center_axis',(0.,1.,0.));
#10759=DIRECTION('ref_axis',(1.,0.,0.));
#10760=DIRECTION('axis',(0.,0.,1.));
#10761=DIRECTION('refdir',(1.,0.,0.));
#10762=DIRECTION('center_axis',(0.,1.,0.));
#10763=DIRECTION('ref_axis',(1.,0.,0.));
#10764=DIRECTION('',(0.,-1.,0.));
#10765=DIRECTION('center_axis',(0.,1.,0.));
#10766=DIRECTION('ref_axis',(1.,0.,0.));
#10767=DIRECTION('',(0.,1.,0.));
#10768=DIRECTION('center_axis',(0.,-1.,0.));
#10769=DIRECTION('ref_axis',(1.,0.,0.));
#10770=DIRECTION('',(0.,1.,0.));
#10771=DIRECTION('center_axis',(0.,1.,0.));
#10772=DIRECTION('ref_axis',(1.,0.,0.));
#10773=DIRECTION('',(0.,-1.,0.));
#10774=DIRECTION('center_axis',(0.,-1.,0.));
#10775=DIRECTION('ref_axis',(1.,0.,0.));
#10776=DIRECTION('center_axis',(0.,1.,0.));
#10777=DIRECTION('ref_axis',(1.,0.,0.));
#10778=DIRECTION('',(0.,0.,-1.));
#10779=DIRECTION('',(1.,0.,0.));
#10780=DIRECTION('',(0.,0.,1.));
#10781=DIRECTION('center_axis',(0.,1.,0.));
#10782=DIRECTION('ref_axis',(1.,0.,0.));
#10783=DIRECTION('',(-1.,0.,0.));
#10784=DIRECTION('center_axis',(0.,1.,0.));
#10785=DIRECTION('ref_axis',(1.,0.,0.));
#10786=DIRECTION('',(-1.,0.,0.));
#10787=DIRECTION('center_axis',(0.,0.,-1.));
#10788=DIRECTION('ref_axis',(-1.,0.,0.));
#10789=DIRECTION('',(1.,0.,0.));
#10790=DIRECTION('',(0.,1.,0.));
#10791=DIRECTION('center_axis',(-1.,0.,0.));
#10792=DIRECTION('ref_axis',(0.,0.,1.));
#10793=DIRECTION('',(0.,1.,0.));
#10794=DIRECTION('',(0.,0.,-1.));
#10795=DIRECTION('',(0.,1.,0.));
#10796=DIRECTION('',(0.,0.,-1.));
#10797=DIRECTION('center_axis',(0.,0.,1.));
#10798=DIRECTION('ref_axis',(1.,0.,0.));
#10799=DIRECTION('center_axis',(0.,0.,1.));
#10800=DIRECTION('ref_axis',(1.,0.,0.));
#10801=DIRECTION('',(0.,0.,1.));
#10802=DIRECTION('center_axis',(0.,0.,-1.));
#10803=DIRECTION('ref_axis',(1.,0.,0.));
#10804=DIRECTION('center_axis',(0.,0.,1.));
#10805=DIRECTION('ref_axis',(-0.447213595499958,-0.894427190999916,0.));
#10806=DIRECTION('',(0.,0.,-1.));
#10807=DIRECTION('center_axis',(0.,0.,1.));
#10808=DIRECTION('ref_axis',(1.,0.,0.));
#10809=DIRECTION('',(0.,0.,1.));
#10810=DIRECTION('center_axis',(0.,0.,1.));
#10811=DIRECTION('ref_axis',(1.,0.,0.));
#10812=DIRECTION('center_axis',(0.,1.,0.));
#10813=DIRECTION('ref_axis',(1.,0.,0.));
#10814=DIRECTION('',(1.,0.,0.));
#10815=DIRECTION('',(-1.,0.,0.));
#10816=DIRECTION('center_axis',(0.,0.,-1.));
#10817=DIRECTION('ref_axis',(-1.,0.,0.));
#10818=DIRECTION('',(0.,1.,0.));
#10819=DIRECTION('',(-1.,0.,0.));
#10820=DIRECTION('',(0.,1.,0.));
#10821=DIRECTION('',(1.,0.,0.));
#10822=DIRECTION('center_axis',(-1.,0.,0.));
#10823=DIRECTION('ref_axis',(0.,0.,1.));
#10824=DIRECTION('',(0.,1.,0.));
#10825=DIRECTION('',(0.,0.,1.));
#10826=DIRECTION('center_axis',(0.,1.,0.));
#10827=DIRECTION('ref_axis',(0.,0.,1.));
#10828=DIRECTION('',(1.,0.,0.));
#10829=DIRECTION('',(0.,0.,-1.));
#10830=DIRECTION('center_axis',(0.,0.,1.));
#10831=DIRECTION('ref_axis',(1.,0.,0.));
#10832=DIRECTION('',(0.,1.,0.));
#10833=DIRECTION('center_axis',(1.,0.,0.));
#10834=DIRECTION('ref_axis',(0.,0.,-1.));
#10835=DIRECTION('',(0.,0.,1.));
#10836=DIRECTION('center_axis',(0.,0.,-1.));
#10837=DIRECTION('ref_axis',(-1.,0.,0.));
#10838=DIRECTION('',(0.,-1.,0.));
#10839=DIRECTION('',(1.,0.,0.));
#10840=DIRECTION('center_axis',(0.,1.,0.));
#10841=DIRECTION('ref_axis',(1.,0.,0.));
#10842=DIRECTION('center_axis',(0.,1.,0.));
#10843=DIRECTION('ref_axis',(1.,0.,0.));
#10844=DIRECTION('center_axis',(0.,1.,0.));
#10845=DIRECTION('ref_axis',(1.,0.,0.));
#10846=DIRECTION('center_axis',(0.,0.,1.));
#10847=DIRECTION('ref_axis',(1.,0.,0.));
#10848=DIRECTION('center_axis',(0.,0.,1.));
#10849=DIRECTION('ref_axis',(1.,0.,0.));
#10850=DIRECTION('',(0.,0.,1.));
#10851=DIRECTION('center_axis',(0.,0.,-1.));
#10852=DIRECTION('ref_axis',(1.,0.,0.));
#10853=DIRECTION('center_axis',(-1.,0.,0.));
#10854=DIRECTION('ref_axis',(0.,0.,1.));
#10855=DIRECTION('',(0.,0.,-1.));
#10856=DIRECTION('',(0.,1.,0.));
#10857=DIRECTION('',(0.,0.,1.));
#10858=DIRECTION('',(0.,1.,0.));
#10859=DIRECTION('center_axis',(0.,0.,-1.));
#10860=DIRECTION('ref_axis',(-1.,0.,0.));
#10861=DIRECTION('',(1.,0.,0.));
#10862=DIRECTION('',(-1.,0.,0.));
#10863=DIRECTION('',(0.,1.,0.));
#10864=DIRECTION('center_axis',(1.,0.,0.));
#10865=DIRECTION('ref_axis',(0.,0.,-1.));
#10866=DIRECTION('',(0.,0.,1.));
#10867=DIRECTION('',(0.,0.,-1.));
#10868=DIRECTION('',(0.,1.,0.));
#10869=DIRECTION('center_axis',(0.,0.,1.));
#10870=DIRECTION('ref_axis',(1.,0.,0.));
#10871=DIRECTION('',(-1.,0.,0.));
#10872=DIRECTION('',(1.,0.,0.));
#10873=DIRECTION('center_axis',(0.,1.,0.));
#10874=DIRECTION('ref_axis',(0.,0.,1.));
#10875=DIRECTION('center_axis',(0.,1.,0.));
#10876=DIRECTION('ref_axis',(1.,0.,0.));
#10877=DIRECTION('center_axis',(0.,0.,1.));
#10878=DIRECTION('ref_axis',(1.,0.,0.));
#10879=DIRECTION('center_axis',(0.,0.,1.));
#10880=DIRECTION('ref_axis',(1.,0.,0.));
#10881=DIRECTION('',(0.,0.,1.));
#10882=DIRECTION('center_axis',(0.,0.,-1.));
#10883=DIRECTION('ref_axis',(1.,0.,0.));
#10884=DIRECTION('center_axis',(-1.,0.,0.));
#10885=DIRECTION('ref_axis',(0.,0.,1.));
#10886=DIRECTION('',(0.,0.,-1.));
#10887=DIRECTION('',(0.,1.,0.));
#10888=DIRECTION('',(0.,0.,1.));
#10889=DIRECTION('',(0.,1.,0.));
#10890=DIRECTION('center_axis',(0.,0.,-1.));
#10891=DIRECTION('ref_axis',(-1.,0.,0.));
#10892=DIRECTION('',(1.,0.,0.));
#10893=DIRECTION('',(-1.,0.,0.));
#10894=DIRECTION('',(0.,1.,0.));
#10895=DIRECTION('center_axis',(1.,0.,0.));
#10896=DIRECTION('ref_axis',(0.,0.,-1.));
#10897=DIRECTION('',(0.,0.,1.));
#10898=DIRECTION('',(0.,0.,-1.));
#10899=DIRECTION('',(0.,1.,0.));
#10900=DIRECTION('center_axis',(0.,0.,1.));
#10901=DIRECTION('ref_axis',(1.,0.,0.));
#10902=DIRECTION('',(-1.,0.,0.));
#10903=DIRECTION('',(1.,0.,0.));
#10904=DIRECTION('center_axis',(0.,1.,0.));
#10905=DIRECTION('ref_axis',(0.,0.,1.));
#10906=DIRECTION('center_axis',(0.,1.,0.));
#10907=DIRECTION('ref_axis',(1.,0.,0.));
#10908=DIRECTION('axis',(0.,0.,1.));
#10909=DIRECTION('refdir',(1.,0.,0.));
#10910=DIRECTION('center_axis',(0.,1.,0.));
#10911=DIRECTION('ref_axis',(1.,0.,0.));
#10912=DIRECTION('',(0.,-1.,0.));
#10913=DIRECTION('center_axis',(0.,-1.,0.));
#10914=DIRECTION('ref_axis',(1.,0.,0.));
#10915=DIRECTION('',(0.,1.,0.));
#10916=DIRECTION('center_axis',(0.,1.,0.));
#10917=DIRECTION('ref_axis',(1.,0.,0.));
#10918=DIRECTION('center_axis',(0.,1.,0.));
#10919=DIRECTION('ref_axis',(1.,0.,0.));
#10920=DIRECTION('',(-1.,0.,0.));
#10921=DIRECTION('center_axis',(0.,1.,0.));
#10922=DIRECTION('ref_axis',(1.,0.,0.));
#10923=DIRECTION('',(-1.,0.,0.));
#10924=DIRECTION('center_axis',(0.,0.,1.));
#10925=DIRECTION('ref_axis',(1.,0.,0.));
#10926=DIRECTION('',(1.,0.,0.));
#10927=DIRECTION('',(0.,-1.,0.));
#10928=DIRECTION('center_axis',(0.,0.,1.));
#10929=DIRECTION('ref_axis',(1.,0.,0.));
#10930=DIRECTION('',(0.,1.,0.));
#10931=DIRECTION('',(1.,0.,0.));
#10932=DIRECTION('center_axis',(0.,1.,0.));
#10933=DIRECTION('ref_axis',(1.,0.,0.));
#10934=DIRECTION('center_axis',(0.,1.,0.));
#10935=DIRECTION('ref_axis',(1.,0.,0.));
#10936=DIRECTION('center_axis',(0.,1.,0.));
#10937=DIRECTION('ref_axis',(1.,0.,0.));
#10938=DIRECTION('center_axis',(0.,0.,1.));
#10939=DIRECTION('ref_axis',(1.,0.,0.));
#10940=DIRECTION('center_axis',(0.,0.,1.));
#10941=DIRECTION('ref_axis',(1.,0.,0.));
#10942=DIRECTION('',(0.,0.,1.));
#10943=DIRECTION('center_axis',(0.,0.,-1.));
#10944=DIRECTION('ref_axis',(1.,0.,0.));
#10945=DIRECTION('center_axis',(-1.,0.,0.));
#10946=DIRECTION('ref_axis',(0.,0.,1.));
#10947=DIRECTION('',(0.,0.,-1.));
#10948=DIRECTION('',(0.,1.,0.));
#10949=DIRECTION('',(0.,0.,1.));
#10950=DIRECTION('',(0.,1.,0.));
#10951=DIRECTION('center_axis',(0.,0.,-1.));
#10952=DIRECTION('ref_axis',(-1.,0.,0.));
#10953=DIRECTION('',(1.,0.,0.));
#10954=DIRECTION('',(-1.,0.,0.));
#10955=DIRECTION('',(0.,1.,0.));
#10956=DIRECTION('center_axis',(1.,0.,0.));
#10957=DIRECTION('ref_axis',(0.,0.,-1.));
#10958=DIRECTION('',(0.,0.,1.));
#10959=DIRECTION('',(0.,0.,-1.));
#10960=DIRECTION('',(0.,1.,0.));
#10961=DIRECTION('center_axis',(0.,0.,1.));
#10962=DIRECTION('ref_axis',(1.,0.,0.));
#10963=DIRECTION('',(-1.,0.,0.));
#10964=DIRECTION('',(1.,0.,0.));
#10965=DIRECTION('center_axis',(0.,1.,0.));
#10966=DIRECTION('ref_axis',(0.,0.,1.));
#10967=DIRECTION('center_axis',(0.,1.,0.));
#10968=DIRECTION('ref_axis',(1.,0.,0.));
#10969=DIRECTION('center_axis',(0.,0.,1.));
#10970=DIRECTION('ref_axis',(1.,0.,0.));
#10971=DIRECTION('center_axis',(0.,0.,1.));
#10972=DIRECTION('ref_axis',(1.,0.,0.));
#10973=DIRECTION('',(0.,0.,1.));
#10974=DIRECTION('center_axis',(0.,0.,-1.));
#10975=DIRECTION('ref_axis',(1.,0.,0.));
#10976=DIRECTION('center_axis',(-1.,0.,0.));
#10977=DIRECTION('ref_axis',(0.,0.,1.));
#10978=DIRECTION('',(0.,0.,-1.));
#10979=DIRECTION('',(0.,1.,0.));
#10980=DIRECTION('',(0.,0.,1.));
#10981=DIRECTION('',(0.,1.,0.));
#10982=DIRECTION('center_axis',(0.,0.,-1.));
#10983=DIRECTION('ref_axis',(-1.,0.,0.));
#10984=DIRECTION('',(1.,0.,0.));
#10985=DIRECTION('',(-1.,0.,0.));
#10986=DIRECTION('',(0.,1.,0.));
#10987=DIRECTION('center_axis',(1.,0.,0.));
#10988=DIRECTION('ref_axis',(0.,0.,-1.));
#10989=DIRECTION('',(0.,0.,1.));
#10990=DIRECTION('',(0.,0.,-1.));
#10991=DIRECTION('',(0.,1.,0.));
#10992=DIRECTION('center_axis',(0.,0.,1.));
#10993=DIRECTION('ref_axis',(1.,0.,0.));
#10994=DIRECTION('',(-1.,0.,0.));
#10995=DIRECTION('',(1.,0.,0.));
#10996=DIRECTION('center_axis',(0.,1.,0.));
#10997=DIRECTION('ref_axis',(0.,0.,1.));
#10998=DIRECTION('center_axis',(0.,1.,0.));
#10999=DIRECTION('ref_axis',(1.,0.,0.));
#11000=DIRECTION('axis',(0.,0.,1.));
#11001=DIRECTION('refdir',(1.,0.,0.));
#11002=DIRECTION('center_axis',(0.,0.,-1.));
#11003=DIRECTION('ref_axis',(-1.,0.,0.));
#11004=DIRECTION('',(0.,-1.,0.));
#11005=DIRECTION('',(1.,0.,0.));
#11006=DIRECTION('',(0.,1.,0.));
#11007=DIRECTION('',(-1.,0.,0.));
#11008=DIRECTION('center_axis',(0.,0.,-1.));
#11009=DIRECTION('ref_axis',(-1.,0.,0.));
#11010=DIRECTION('',(0.,1.,0.));
#11011=DIRECTION('',(-1.,0.,0.));
#11012=DIRECTION('',(0.,-1.,0.));
#11013=DIRECTION('',(1.,0.,0.));
#11014=DIRECTION('center_axis',(0.,1.,0.));
#11015=DIRECTION('ref_axis',(1.,0.,0.));
#11016=DIRECTION('center_axis',(0.,1.,0.));
#11017=DIRECTION('ref_axis',(1.,0.,0.));
#11018=DIRECTION('center_axis',(0.,-1.,0.));
#11019=DIRECTION('ref_axis',(1.,0.,0.));
#11020=DIRECTION('center_axis',(0.,1.,0.));
#11021=DIRECTION('ref_axis',(1.,0.,0.));
#11022=DIRECTION('center_axis',(0.,-1.,0.));
#11023=DIRECTION('ref_axis',(1.,0.,0.));
#11024=DIRECTION('center_axis',(0.,1.,0.));
#11025=DIRECTION('ref_axis',(1.,0.,0.));
#11026=DIRECTION('center_axis',(0.,1.,0.));
#11027=DIRECTION('ref_axis',(1.,0.,0.));
#11028=DIRECTION('center_axis',(0.,1.,0.));
#11029=DIRECTION('ref_axis',(1.,0.,0.));
#11030=DIRECTION('axis',(0.,0.,1.));
#11031=DIRECTION('refdir',(1.,0.,0.));
#11032=DIRECTION('center_axis',(0.,0.,1.));
#11033=DIRECTION('ref_axis',(1.,0.,0.));
#11034=DIRECTION('',(0.,-1.,0.));
#11035=DIRECTION('',(-1.,0.,0.));
#11036=DIRECTION('',(0.,1.,0.));
#11037=DIRECTION('',(1.,0.,0.));
#11038=DIRECTION('center_axis',(0.,0.,1.));
#11039=DIRECTION('ref_axis',(1.,0.,0.));
#11040=DIRECTION('',(0.,1.,0.));
#11041=DIRECTION('',(1.,0.,0.));
#11042=DIRECTION('',(0.,-1.,0.));
#11043=DIRECTION('',(-1.,0.,0.));
#11044=DIRECTION('center_axis',(0.,1.,0.));
#11045=DIRECTION('ref_axis',(1.,0.,0.));
#11046=DIRECTION('center_axis',(0.,1.,0.));
#11047=DIRECTION('ref_axis',(1.,0.,0.));
#11048=DIRECTION('center_axis',(0.,-1.,0.));
#11049=DIRECTION('ref_axis',(1.,0.,0.));
#11050=DIRECTION('center_axis',(0.,1.,0.));
#11051=DIRECTION('ref_axis',(1.,0.,0.));
#11052=DIRECTION('center_axis',(0.,-1.,0.));
#11053=DIRECTION('ref_axis',(1.,0.,0.));
#11054=DIRECTION('center_axis',(0.,1.,0.));
#11055=DIRECTION('ref_axis',(1.,0.,0.));
#11056=DIRECTION('center_axis',(0.,1.,0.));
#11057=DIRECTION('ref_axis',(1.,0.,0.));
#11058=DIRECTION('center_axis',(0.,1.,0.));
#11059=DIRECTION('ref_axis',(1.,0.,0.));
#11060=DIRECTION('axis',(0.,0.,1.));
#11061=DIRECTION('refdir',(1.,0.,0.));
#11062=DIRECTION('center_axis',(0.,1.,0.));
#11063=DIRECTION('ref_axis',(-1.,0.,0.));
#11064=DIRECTION('',(-1.,0.,0.));
#11065=DIRECTION('',(0.,0.,1.));
#11066=DIRECTION('',(-1.,0.,0.));
#11067=DIRECTION('',(0.,0.,1.));
#11068=DIRECTION('center_axis',(1.,0.,0.));
#11069=DIRECTION('ref_axis',(0.,1.,0.));
#11070=DIRECTION('',(0.,1.,0.));
#11071=DIRECTION('',(0.,1.,0.));
#11072=DIRECTION('',(0.,0.,1.));
#11073=DIRECTION('center_axis',(0.,-1.,0.));
#11074=DIRECTION('ref_axis',(1.,0.,0.));
#11075=DIRECTION('',(1.,0.,0.));
#11076=DIRECTION('',(1.,0.,0.));
#11077=DIRECTION('',(0.,0.,1.));
#11078=DIRECTION('center_axis',(-1.,0.,0.));
#11079=DIRECTION('ref_axis',(0.,-1.,0.));
#11080=DIRECTION('',(0.,-1.,0.));
#11081=DIRECTION('',(0.,-1.,0.));
#11082=DIRECTION('center_axis',(0.,0.,1.));
#11083=DIRECTION('ref_axis',(1.,0.,0.));
#11084=DIRECTION('center_axis',(0.,0.,1.));
#11085=DIRECTION('ref_axis',(1.,0.,0.));
#11086=DIRECTION('axis',(0.,0.,1.));
#11087=DIRECTION('refdir',(1.,0.,0.));
#11088=DIRECTION('center_axis',(0.,1.,0.));
#11089=DIRECTION('ref_axis',(-1.,0.,0.));
#11090=DIRECTION('',(-1.,0.,0.));
#11091=DIRECTION('',(0.,0.,1.));
#11092=DIRECTION('',(-1.,0.,0.));
#11093=DIRECTION('',(0.,0.,1.));
#11094=DIRECTION('center_axis',(1.,0.,0.));
#11095=DIRECTION('ref_axis',(0.,1.,0.));
#11096=DIRECTION('',(0.,1.,0.));
#11097=DIRECTION('',(0.,1.,0.));
#11098=DIRECTION('',(0.,0.,1.));
#11099=DIRECTION('center_axis',(0.,-1.,0.));
#11100=DIRECTION('ref_axis',(1.,0.,0.));
#11101=DIRECTION('',(1.,0.,0.));
#11102=DIRECTION('',(1.,0.,0.));
#11103=DIRECTION('',(0.,0.,1.));
#11104=DIRECTION('center_axis',(-1.,0.,0.));
#11105=DIRECTION('ref_axis',(0.,-1.,0.));
#11106=DIRECTION('',(0.,-1.,0.));
#11107=DIRECTION('',(0.,-1.,0.));
#11108=DIRECTION('center_axis',(0.,0.,1.));
#11109=DIRECTION('ref_axis',(1.,0.,0.));
#11110=DIRECTION('center_axis',(0.,0.,1.));
#11111=DIRECTION('ref_axis',(1.,0.,0.));
#11112=DIRECTION('axis',(0.,0.,1.));
#11113=DIRECTION('refdir',(1.,0.,0.));
#11114=DIRECTION('center_axis',(0.866025403784439,0.,-0.5));
#11115=DIRECTION('ref_axis',(0.5,0.,0.866025403784439));
#11116=DIRECTION('',(-0.5,0.,-0.866025403784439));
#11117=DIRECTION('',(0.,-1.,0.));
#11118=DIRECTION('',(0.5,0.,0.866025403784439));
#11119=DIRECTION('',(0.,-1.,0.));
#11120=DIRECTION('center_axis',(1.92296268638356E-16,0.,-1.));
#11121=DIRECTION('ref_axis',(1.,0.,1.92296268638356E-16));
#11122=DIRECTION('',(-1.,0.,-1.92296268638356E-16));
#11123=DIRECTION('',(0.,-1.,0.));
#11124=DIRECTION('',(1.,0.,1.92296268638356E-16));
#11125=DIRECTION('center_axis',(-0.866025403784439,0.,-0.5));
#11126=DIRECTION('ref_axis',(0.5,0.,-0.866025403784439));
#11127=DIRECTION('',(-0.5,0.,0.866025403784438));
#11128=DIRECTION('',(0.,-1.,0.));
#11129=DIRECTION('',(0.5,0.,-0.866025403784438));
#11130=DIRECTION('center_axis',(-0.866025403784439,0.,0.5));
#11131=DIRECTION('ref_axis',(-0.5,0.,-0.866025403784439));
#11132=DIRECTION('',(0.5,0.,0.866025403784439));
#11133=DIRECTION('',(0.,-1.,0.));
#11134=DIRECTION('',(-0.5,0.,-0.866025403784439));
#11135=DIRECTION('center_axis',(-1.92296268638356E-16,0.,1.));
#11136=DIRECTION('ref_axis',(-1.,0.,-1.92296268638356E-16));
#11137=DIRECTION('',(1.,0.,1.92296268638356E-16));
#11138=DIRECTION('',(0.,-1.,0.));
#11139=DIRECTION('',(-1.,0.,-1.92296268638356E-16));
#11140=DIRECTION('center_axis',(0.866025403784439,0.,0.5));
#11141=DIRECTION('ref_axis',(-0.5,0.,0.866025403784439));
#11142=DIRECTION('',(0.5,0.,-0.866025403784439));
#11143=DIRECTION('',(-0.5,0.,0.866025403784439));
#11144=DIRECTION('center_axis',(0.,1.,0.));
#11145=DIRECTION('ref_axis',(1.,0.,0.));
#11146=DIRECTION('center_axis',(0.,-1.,0.));
#11147=DIRECTION('ref_axis',(0.,0.,-1.));
#11148=DIRECTION('center_axis',(0.,1.,0.));
#11149=DIRECTION('ref_axis',(1.,0.,0.));
#11150=DIRECTION('center_axis',(0.,1.,0.));
#11151=DIRECTION('ref_axis',(1.,0.,0.));
#11152=DIRECTION('center_axis',(0.,1.,0.));
#11153=DIRECTION('ref_axis',(0.,0.,1.));
#11154=DIRECTION('center_axis',(0.,-1.,0.));
#11155=DIRECTION('ref_axis',(1.,0.,0.));
#11156=DIRECTION('center_axis',(0.,-1.,0.));
#11157=DIRECTION('ref_axis',(1.,0.,0.));
#11158=DIRECTION('center_axis',(0.,-1.,0.));
#11159=DIRECTION('ref_axis',(1.,0.,0.));
#11160=DIRECTION('',(0.707106781186548,0.707106781186547,8.65956056235494E-17));
#11161=DIRECTION('center_axis',(0.,-1.,0.));
#11162=DIRECTION('ref_axis',(1.,0.,0.));
#11163=DIRECTION('center_axis',(0.,-1.,0.));
#11164=DIRECTION('ref_axis',(1.,0.,0.));
#11165=DIRECTION('',(0.,1.,0.));
#11166=DIRECTION('center_axis',(0.,1.,0.));
#11167=DIRECTION('ref_axis',(1.,0.,0.));
#11168=DIRECTION('center_axis',(0.,-1.,0.));
#11169=DIRECTION('ref_axis',(1.,0.,0.));
#11170=DIRECTION('',(-0.707106781186547,0.707106781186548,-8.65956056235493E-17));
#11171=DIRECTION('center_axis',(0.,-1.,0.));
#11172=DIRECTION('ref_axis',(0.,0.,-1.));
#11173=DIRECTION('center_axis',(0.,-1.,0.));
#11174=DIRECTION('ref_axis',(1.,0.,0.));
#11175=DIRECTION('center_axis',(0.,1.,0.));
#11176=DIRECTION('ref_axis',(1.,0.,0.));
#11177=DIRECTION('center_axis',(0.,1.,0.));
#11178=DIRECTION('ref_axis',(1.,0.,0.));
#11179=DIRECTION('',(-0.447213595499958,0.894427190999916,-5.47678698264203E-17));
#11180=DIRECTION('center_axis',(0.,-1.,0.));
#11181=DIRECTION('ref_axis',(1.,0.,0.));
#11182=DIRECTION('',(0.,1.,0.));
#11183=DIRECTION('axis',(0.,0.,1.));
#11184=DIRECTION('refdir',(1.,0.,0.));
#11185=DIRECTION('center_axis',(0.866025403784439,0.,-0.5));
#11186=DIRECTION('ref_axis',(0.5,0.,0.866025403784439));
#11187=DIRECTION('',(-0.5,0.,-0.866025403784439));
#11188=DIRECTION('',(0.,-1.,0.));
#11189=DIRECTION('',(0.5,0.,0.866025403784439));
#11190=DIRECTION('',(0.,-1.,0.));
#11191=DIRECTION('center_axis',(1.60246890531964E-16,0.,-1.));
#11192=DIRECTION('ref_axis',(1.,0.,1.60246890531964E-16));
#11193=DIRECTION('',(-1.,0.,-1.60246890531964E-16));
#11194=DIRECTION('',(0.,-1.,0.));
#11195=DIRECTION('',(1.,0.,1.60246890531964E-16));
#11196=DIRECTION('center_axis',(-0.866025403784439,0.,-0.5));
#11197=DIRECTION('ref_axis',(0.5,0.,-0.866025403784439));
#11198=DIRECTION('',(-0.5,0.,0.866025403784439));
#11199=DIRECTION('',(0.,-1.,0.));
#11200=DIRECTION('',(0.5,0.,-0.866025403784439));
#11201=DIRECTION('center_axis',(-0.866025403784439,0.,0.5));
#11202=DIRECTION('ref_axis',(-0.5,0.,-0.866025403784439));
#11203=DIRECTION('',(0.5,0.,0.866025403784439));
#11204=DIRECTION('',(0.,-1.,0.));
#11205=DIRECTION('',(-0.5,0.,-0.866025403784439));
#11206=DIRECTION('center_axis',(-1.60246890531964E-16,0.,1.));
#11207=DIRECTION('ref_axis',(-1.,0.,-1.60246890531964E-16));
#11208=DIRECTION('',(1.,0.,1.60246890531964E-16));
#11209=DIRECTION('',(0.,-1.,0.));
#11210=DIRECTION('',(-1.,0.,-1.60246890531964E-16));
#11211=DIRECTION('center_axis',(0.866025403784439,0.,0.5));
#11212=DIRECTION('ref_axis',(-0.5,0.,0.866025403784439));
#11213=DIRECTION('',(0.5,0.,-0.866025403784439));
#11214=DIRECTION('',(-0.5,0.,0.866025403784439));
#11215=DIRECTION('center_axis',(0.,1.,0.));
#11216=DIRECTION('ref_axis',(1.,0.,0.));
#11217=DIRECTION('center_axis',(0.,-1.,0.));
#11218=DIRECTION('ref_axis',(0.,0.,-1.));
#11219=DIRECTION('center_axis',(0.,1.,0.));
#11220=DIRECTION('ref_axis',(1.,0.,0.));
#11221=DIRECTION('center_axis',(0.,1.,0.));
#11222=DIRECTION('ref_axis',(1.,0.,0.));
#11223=DIRECTION('center_axis',(0.,1.,0.));
#11224=DIRECTION('ref_axis',(1.,0.,0.));
#11225=DIRECTION('center_axis',(0.,1.,0.));
#11226=DIRECTION('ref_axis',(1.,0.,0.));
#11227=DIRECTION('',(0.,-1.,0.));
#11228=DIRECTION('center_axis',(0.,1.,0.));
#11229=DIRECTION('ref_axis',(1.,0.,0.));
#11230=DIRECTION('center_axis',(0.,1.,0.));
#11231=DIRECTION('ref_axis',(1.,0.,0.));
#11232=DIRECTION('center_axis',(0.,1.,0.));
#11233=DIRECTION('ref_axis',(0.,0.,1.));
#11234=DIRECTION('center_axis',(0.,-1.,0.));
#11235=DIRECTION('ref_axis',(1.,0.,0.));
#11236=DIRECTION('center_axis',(0.,-1.,0.));
#11237=DIRECTION('ref_axis',(1.,0.,0.));
#11238=DIRECTION('center_axis',(0.,-1.,0.));
#11239=DIRECTION('ref_axis',(1.,0.,0.));
#11240=DIRECTION('',(0.707106781186548,0.707106781186547,8.65956056235493E-17));
#11241=DIRECTION('center_axis',(0.,-1.,0.));
#11242=DIRECTION('ref_axis',(1.,0.,0.));
#11243=DIRECTION('center_axis',(0.,-1.,0.));
#11244=DIRECTION('ref_axis',(1.,0.,0.));
#11245=DIRECTION('',(0.,1.,0.));
#11246=DIRECTION('center_axis',(0.,1.,0.));
#11247=DIRECTION('ref_axis',(1.,0.,0.));
#11248=DIRECTION('center_axis',(0.,-1.,0.));
#11249=DIRECTION('ref_axis',(1.,0.,0.));
#11250=DIRECTION('',(-0.707106781186548,0.707106781186547,-8.65956056235494E-17));
#11251=DIRECTION('center_axis',(0.,-1.,0.));
#11252=DIRECTION('ref_axis',(0.,0.,-1.));
#11253=DIRECTION('center_axis',(0.,-1.,0.));
#11254=DIRECTION('ref_axis',(1.,0.,0.));
#11255=DIRECTION('center_axis',(0.,1.,0.));
#11256=DIRECTION('ref_axis',(1.,0.,0.));
#11257=DIRECTION('center_axis',(0.,1.,0.));
#11258=DIRECTION('ref_axis',(1.,0.,0.));
#11259=DIRECTION('',(-0.447213595499958,0.894427190999916,-5.47678698264203E-17));
#11260=DIRECTION('center_axis',(0.,-1.,0.));
#11261=DIRECTION('ref_axis',(1.,0.,0.));
#11262=DIRECTION('',(0.,1.,0.));
#11263=DIRECTION('axis',(0.,0.,1.));
#11264=DIRECTION('refdir',(1.,0.,0.));
#11265=DIRECTION('center_axis',(0.,1.,0.));
#11266=DIRECTION('ref_axis',(1.,0.,0.));
#11267=DIRECTION('center_axis',(0.,-1.,0.));
#11268=DIRECTION('ref_axis',(1.,0.,0.));
#11269=DIRECTION('',(0.,-1.,0.));
#11270=DIRECTION('center_axis',(0.,-1.,0.));
#11271=DIRECTION('ref_axis',(1.,0.,0.));
#11272=DIRECTION('center_axis',(0.,1.,0.));
#11273=DIRECTION('ref_axis',(1.,0.,0.));
#11274=DIRECTION('center_axis',(0.,1.,0.));
#11275=DIRECTION('ref_axis',(1.,0.,0.));
#11276=DIRECTION('',(0.,-1.,0.));
#11277=DIRECTION('center_axis',(0.,1.,0.));
#11278=DIRECTION('ref_axis',(1.,0.,0.));
#11279=DIRECTION('center_axis',(0.,1.,0.));
#11280=DIRECTION('ref_axis',(1.,0.,0.));
#11281=DIRECTION('center_axis',(0.,1.,0.));
#11282=DIRECTION('ref_axis',(1.,0.,0.));
#11283=DIRECTION('axis',(0.,0.,1.));
#11284=DIRECTION('refdir',(1.,0.,0.));
#11285=DIRECTION('center_axis',(0.,1.,0.));
#11286=DIRECTION('ref_axis',(1.,0.,0.));
#11287=DIRECTION('',(0.866025403784439,-0.5,1.06057523872491E-16));
#11288=DIRECTION('center_axis',(0.,-1.,0.));
#11289=DIRECTION('ref_axis',(1.,0.,0.));
#11290=DIRECTION('center_axis',(0.,-1.,0.));
#11291=DIRECTION('ref_axis',(1.,0.,0.));
#11292=DIRECTION('center_axis',(0.,1.,0.));
#11293=DIRECTION('ref_axis',(1.,0.,0.));
#11294=DIRECTION('',(-0.866025403784439,-0.5,-1.06057523872491E-16));
#11295=DIRECTION('center_axis',(1.4792020664489E-16,0.,-1.));
#11296=DIRECTION('ref_axis',(-1.,0.,-1.4792020664489E-16));
#11297=DIRECTION('',(0.,1.,0.));
#11298=DIRECTION('',(0.,1.,0.));
#11299=DIRECTION('center_axis',(-0.866025403784439,0.,-0.5));
#11300=DIRECTION('ref_axis',(-0.5,0.,0.866025403784439));
#11301=DIRECTION('',(0.,1.,0.));
#11302=DIRECTION('center_axis',(-0.866025403784439,0.,0.5));
#11303=DIRECTION('ref_axis',(0.5,0.,0.866025403784439));
#11304=DIRECTION('',(0.,1.,0.));
#11305=DIRECTION('center_axis',(0.,1.,0.));
#11306=DIRECTION('ref_axis',(1.,0.,0.));
#11307=DIRECTION('center_axis',(0.,1.,0.));
#11308=DIRECTION('ref_axis',(1.,0.,0.));
#11309=DIRECTION('',(0.,-1.,0.));
#11310=DIRECTION('center_axis',(0.,1.,0.));
#11311=DIRECTION('ref_axis',(1.,0.,0.));
#11312=DIRECTION('center_axis',(-2.95840413289779E-16,0.,1.));
#11313=DIRECTION('ref_axis',(1.,0.,2.95840413289779E-16));
#11314=DIRECTION('',(0.,1.,0.));
#11315=DIRECTION('center_axis',(0.866025403784439,0.,-0.5));
#11316=DIRECTION('ref_axis',(-0.5,0.,-0.866025403784439));
#11317=DIRECTION('',(0.,1.,0.));
#11318=DIRECTION('center_axis',(0.866025403784439,0.,0.5));
#11319=DIRECTION('ref_axis',(0.5,0.,-0.866025403784439));
#11320=DIRECTION('center_axis',(0.,1.,0.));
#11321=DIRECTION('ref_axis',(1.,0.,0.));
#11322=DIRECTION('center_axis',(0.,1.,0.));
#11323=DIRECTION('ref_axis',(1.,0.,0.));
#11324=DIRECTION('',(0.,0.,1.));
#11325=DIRECTION('',(1.,0.,0.));
#11326=DIRECTION('',(0.,0.,1.));
#11327=DIRECTION('',(1.,0.,0.));
#11328=DIRECTION('',(0.,0.,1.));
#11329=DIRECTION('',(1.,0.,0.));
#11330=DIRECTION('',(0.,0.,1.));
#11331=DIRECTION('',(1.,0.,0.));
#11332=DIRECTION('',(0.,0.,1.));
#11333=DIRECTION('',(1.,0.,0.));
#11334=DIRECTION('',(0.,0.,1.));
#11335=DIRECTION('',(1.,0.,0.));
#11336=DIRECTION('',(0.,0.,1.));
#11337=DIRECTION('',(1.,0.,0.));
#11338=DIRECTION('',(0.,0.,1.));
#11339=DIRECTION('',(1.,0.,0.));
#11340=DIRECTION('',(0.,0.,1.));
#11341=DIRECTION('',(1.,0.,0.));
#11342=DIRECTION('',(0.,0.,1.));
#11343=DIRECTION('',(1.,0.,0.));
#11344=DIRECTION('',(0.,0.,1.));
#11345=DIRECTION('',(1.,0.,0.));
#11346=DIRECTION('',(0.,0.,1.));
#11347=DIRECTION('',(1.,0.,0.));
#11348=DIRECTION('',(0.,0.,1.));
#11349=DIRECTION('',(1.,0.,0.));
#11350=DIRECTION('',(0.,0.,1.));
#11351=DIRECTION('',(1.,0.,0.));
#11352=DIRECTION('',(0.,-1.,2.22044604925031E-16));
#11353=DIRECTION('',(1.,0.,0.));
#11354=DIRECTION('',(0.,-1.,2.22044604925031E-16));
#11355=DIRECTION('',(1.,0.,0.));
#11356=DIRECTION('',(0.,-1.,2.22044604925031E-16));
#11357=DIRECTION('',(1.,0.,0.));
#11358=DIRECTION('',(0.,-1.,2.22044604925031E-16));
#11359=DIRECTION('',(1.,0.,0.));
#11360=DIRECTION('',(0.,-1.,2.22044604925031E-16));
#11361=DIRECTION('',(1.,0.,0.));
#11362=DIRECTION('',(0.,-1.,2.22044604925031E-16));
#11363=DIRECTION('',(1.,0.,0.));
#11364=DIRECTION('',(0.,1.,2.22044604925031E-16));
#11365=DIRECTION('',(1.,0.,0.));
#11366=DIRECTION('',(0.,1.,2.22044604925031E-16));
#11367=DIRECTION('',(1.,0.,0.));
#11368=DIRECTION('',(0.,-1.,2.22044604925031E-16));
#11369=DIRECTION('',(1.,0.,0.));
#11370=DIRECTION('',(0.,-1.,2.22044604925031E-16));
#11371=DIRECTION('',(1.,0.,0.));
#11372=DIRECTION('',(0.,1.,2.22044604925031E-16));
#11373=DIRECTION('',(1.,0.,0.));
#11374=DIRECTION('',(0.,1.,2.22044604925031E-16));
#11375=DIRECTION('',(1.,0.,0.));
#11376=DIRECTION('',(0.,-1.,2.22044604925031E-16));
#11377=DIRECTION('',(1.,0.,0.));
#11378=DIRECTION('',(0.,-1.,2.22044604925031E-16));
#11379=DIRECTION('',(1.,0.,0.));
#11380=DIRECTION('',(0.,1.,2.22044604925031E-16));
#11381=DIRECTION('',(1.,0.,0.));
#11382=DIRECTION('',(0.,1.,2.22044604925031E-16));
#11383=DIRECTION('',(1.,0.,0.));
#11384=DIRECTION('',(0.,-1.,2.22044604925031E-16));
#11385=DIRECTION('',(1.,0.,0.));
#11386=DIRECTION('',(0.,-1.,2.22044604925031E-16));
#11387=DIRECTION('',(1.,0.,0.));
#11388=DIRECTION('',(0.,1.,2.22044604925031E-16));
#11389=DIRECTION('',(1.,0.,0.));
#11390=DIRECTION('',(0.,1.,2.22044604925031E-16));
#11391=DIRECTION('',(1.,0.,0.));
#11392=DIRECTION('axis',(0.,0.,1.));
#11393=DIRECTION('refdir',(1.,0.,0.));
#11394=DIRECTION('axis',(0.,0.,1.));
#11395=DIRECTION('refdir',(1.,0.,0.));
#11396=DIRECTION('center_axis',(0.,0.,1.));
#11397=DIRECTION('ref_axis',(1.,0.,0.));
#11398=DIRECTION('',(0.,0.,1.));
#11399=DIRECTION('center_axis',(0.,0.,-1.));
#11400=DIRECTION('ref_axis',(1.,0.,0.));
#11401=DIRECTION('center_axis',(0.,0.,1.));
#11402=DIRECTION('ref_axis',(1.,0.,0.));
#11403=DIRECTION('',(0.,0.,1.));
#11404=DIRECTION('center_axis',(0.,0.,1.));
#11405=DIRECTION('ref_axis',(1.,0.,0.));
#11406=DIRECTION('',(0.,0.,1.));
#11407=DIRECTION('center_axis',(0.,0.,1.));
#11408=DIRECTION('ref_axis',(0.936891289691661,0.349620810736282,0.));
#11409=DIRECTION('',(0.,0.,1.));
#11410=DIRECTION('center_axis',(0.,0.,-1.));
#11411=DIRECTION('ref_axis',(1.,0.,0.));
#11412=DIRECTION('center_axis',(0.,0.,1.));
#11413=DIRECTION('ref_axis',(1.,-1.39727864928002E-15,0.));
#11414=DIRECTION('',(1.22464679914735E-16,-1.56119684709152E-31,1.));
#11415=DIRECTION('center_axis',(0.,0.,-1.));
#11416=DIRECTION('ref_axis',(1.,-1.39727864928002E-15,0.));
#11417=DIRECTION('center_axis',(0.,0.,1.));
#11418=DIRECTION('ref_axis',(1.,-1.39727864928002E-15,0.));
#11419=DIRECTION('',(1.22464679914735E-16,-1.56119684709152E-31,1.));
#11420=DIRECTION('center_axis',(0.,0.,1.));
#11421=DIRECTION('ref_axis',(1.,-1.39727864928002E-15,0.));
#11422=DIRECTION('',(1.22464679914735E-16,-1.56119684709152E-31,1.));
#11423=DIRECTION('center_axis',(0.,0.,1.));
#11424=DIRECTION('ref_axis',(-0.608867739087164,0.79327175438111,0.));
#11425=DIRECTION('',(1.22464679914735E-16,-1.56119684709152E-31,1.));
#11426=DIRECTION('center_axis',(0.,0.,1.));
#11427=DIRECTION('ref_axis',(1.,-1.39727864928002E-15,0.));
#11428=DIRECTION('center_axis',(0.,0.,1.));
#11429=DIRECTION('ref_axis',(1.,-1.39727864928002E-15,0.));
#11430=DIRECTION('center_axis',(0.,0.,1.));
#11431=DIRECTION('ref_axis',(1.,0.,0.));
#11432=DIRECTION('',(0.5,0.866025403784439,0.));
#11433=DIRECTION('',(-0.5,0.866025403784439,0.));
#11434=DIRECTION('',(-1.,0.,0.));
#11435=DIRECTION('',(-0.5,-0.866025403784439,0.));
#11436=DIRECTION('',(0.499999999999999,-0.866025403784439,0.));
#11437=DIRECTION('',(1.,-2.13662520709285E-16,0.));
#11438=DIRECTION('center_axis',(0.,0.,1.));
#11439=DIRECTION('ref_axis',(1.,0.,0.));
#11440=DIRECTION('center_axis',(-2.13662520709285E-16,-1.,0.));
#11441=DIRECTION('ref_axis',(1.,-2.13662520709285E-16,0.));
#11442=DIRECTION('',(1.,-2.13662520709285E-16,0.));
#11443=DIRECTION('',(0.,0.,1.));
#11444=DIRECTION('',(0.,0.,1.));
#11445=DIRECTION('center_axis',(-0.866025403784439,-0.499999999999999,0.));
#11446=DIRECTION('ref_axis',(0.499999999999999,-0.866025403784439,0.));
#11447=DIRECTION('',(0.499999999999999,-0.866025403784439,0.));
#11448=DIRECTION('',(0.,0.,1.));
#11449=DIRECTION('center_axis',(-0.866025403784439,0.5,0.));
#11450=DIRECTION('ref_axis',(-0.5,-0.866025403784439,0.));
#11451=DIRECTION('',(-0.5,-0.866025403784439,0.));
#11452=DIRECTION('',(0.,0.,1.));
#11453=DIRECTION('center_axis',(0.,1.,0.));
#11454=DIRECTION('ref_axis',(-1.,0.,0.));
#11455=DIRECTION('',(-1.,0.,0.));
#11456=DIRECTION('',(0.,0.,1.));
#11457=DIRECTION('center_axis',(0.866025403784439,0.5,0.));
#11458=DIRECTION('ref_axis',(-0.5,0.866025403784439,0.));
#11459=DIRECTION('',(-0.5,0.866025403784439,0.));
#11460=DIRECTION('',(0.,0.,1.));
#11461=DIRECTION('center_axis',(0.866025403784439,-0.5,0.));
#11462=DIRECTION('ref_axis',(0.5,0.866025403784439,0.));
#11463=DIRECTION('',(0.5,0.866025403784439,0.));
#11464=DIRECTION('center_axis',(0.,0.,1.));
#11465=DIRECTION('ref_axis',(1.,0.,0.));
#11466=DIRECTION('',(0.,0.,1.));
#11467=DIRECTION('',(1.,0.,0.));
#11468=DIRECTION('axis',(0.,0.,1.));
#11469=DIRECTION('refdir',(1.,0.,0.));
#11470=DIRECTION('axis',(0.,0.,1.));
#11471=DIRECTION('refdir',(1.,0.,0.));
#11472=DIRECTION('center_axis',(0.,0.,1.));
#11473=DIRECTION('ref_axis',(1.,0.,0.));
#11474=DIRECTION('',(0.,0.,1.));
#11475=DIRECTION('center_axis',(0.,0.,-1.));
#11476=DIRECTION('ref_axis',(1.,0.,0.));
#11477=DIRECTION('center_axis',(0.,0.,1.));
#11478=DIRECTION('ref_axis',(1.,0.,0.));
#11479=DIRECTION('',(0.,0.,1.));
#11480=DIRECTION('center_axis',(0.,0.,1.));
#11481=DIRECTION('ref_axis',(1.,0.,0.));
#11482=DIRECTION('',(0.,0.,1.));
#11483=DIRECTION('center_axis',(0.,0.,1.));
#11484=DIRECTION('ref_axis',(0.936891279057678,0.349620839232545,0.));
#11485=DIRECTION('',(0.,0.,1.));
#11486=DIRECTION('center_axis',(0.,0.,-1.));
#11487=DIRECTION('ref_axis',(1.,0.,0.));
#11488=DIRECTION('center_axis',(0.,0.,1.));
#11489=DIRECTION('ref_axis',(1.,-1.48847114380753E-15,0.));
#11490=DIRECTION('',(1.22464679914735E-16,-1.6728754436209E-31,1.));
#11491=DIRECTION('center_axis',(0.,0.,-1.));
#11492=DIRECTION('ref_axis',(1.,-1.48847114380753E-15,0.));
#11493=DIRECTION('center_axis',(0.,0.,1.));
#11494=DIRECTION('ref_axis',(1.,-1.48847114380753E-15,0.));
#11495=DIRECTION('',(1.22464679914735E-16,-1.6728754436209E-31,1.));
#11496=DIRECTION('center_axis',(0.,0.,1.));
#11497=DIRECTION('ref_axis',(1.,-1.48847114380753E-15,0.));
#11498=DIRECTION('',(1.22464679914735E-16,-1.6728754436209E-31,1.));
#11499=DIRECTION('center_axis',(0.,0.,1.));
#11500=DIRECTION('ref_axis',(-0.608867914098284,0.793271620053059,0.));
#11501=DIRECTION('',(1.22464679914735E-16,-1.6728754436209E-31,1.));
#11502=DIRECTION('center_axis',(0.,0.,1.));
#11503=DIRECTION('ref_axis',(1.,-1.48847114380753E-15,0.));
#11504=DIRECTION('center_axis',(0.,0.,1.));
#11505=DIRECTION('ref_axis',(1.,-1.48847114380753E-15,0.));
#11506=DIRECTION('center_axis',(0.,0.,1.));
#11507=DIRECTION('ref_axis',(1.,0.,0.));
#11508=DIRECTION('',(0.5,0.866025403784439,0.));
#11509=DIRECTION('',(-0.5,0.866025403784439,0.));
#11510=DIRECTION('',(-1.,0.,0.));
#11511=DIRECTION('',(-0.5,-0.866025403784439,0.));
#11512=DIRECTION('',(0.499999999999999,-0.866025403784439,0.));
#11513=DIRECTION('',(1.,-2.13662520709285E-16,0.));
#11514=DIRECTION('center_axis',(0.,0.,1.));
#11515=DIRECTION('ref_axis',(1.,0.,0.));
#11516=DIRECTION('center_axis',(-2.13662520709285E-16,-1.,0.));
#11517=DIRECTION('ref_axis',(1.,-2.13662520709285E-16,0.));
#11518=DIRECTION('',(1.,-2.13662520709285E-16,0.));
#11519=DIRECTION('',(0.,0.,1.));
#11520=DIRECTION('',(0.,0.,1.));
#11521=DIRECTION('center_axis',(-0.866025403784439,-0.499999999999999,0.));
#11522=DIRECTION('ref_axis',(0.499999999999999,-0.866025403784439,0.));
#11523=DIRECTION('',(0.499999999999999,-0.866025403784439,0.));
#11524=DIRECTION('',(0.,0.,1.));
#11525=DIRECTION('center_axis',(-0.866025403784439,0.5,0.));
#11526=DIRECTION('ref_axis',(-0.5,-0.866025403784439,0.));
#11527=DIRECTION('',(-0.5,-0.866025403784439,0.));
#11528=DIRECTION('',(0.,0.,1.));
#11529=DIRECTION('center_axis',(0.,1.,0.));
#11530=DIRECTION('ref_axis',(-1.,0.,0.));
#11531=DIRECTION('',(-1.,0.,0.));
#11532=DIRECTION('',(0.,0.,1.));
#11533=DIRECTION('center_axis',(0.866025403784439,0.5,0.));
#11534=DIRECTION('ref_axis',(-0.5,0.866025403784439,0.));
#11535=DIRECTION('',(-0.5,0.866025403784439,0.));
#11536=DIRECTION('',(0.,0.,1.));
#11537=DIRECTION('center_axis',(0.866025403784439,-0.5,0.));
#11538=DIRECTION('ref_axis',(0.5,0.866025403784439,0.));
#11539=DIRECTION('',(0.5,0.866025403784439,0.));
#11540=DIRECTION('center_axis',(0.,0.,1.));
#11541=DIRECTION('ref_axis',(1.,0.,0.));
#11542=DIRECTION('',(0.,0.,1.));
#11543=DIRECTION('',(1.,0.,0.));
#11544=DIRECTION('axis',(0.,0.,1.));
#11545=DIRECTION('refdir',(1.,0.,0.));
#11546=DIRECTION('axis',(0.,0.,1.));
#11547=DIRECTION('refdir',(1.,0.,0.));
#11548=DIRECTION('center_axis',(0.,0.,1.));
#11549=DIRECTION('ref_axis',(-0.349612887919324,-0.936894246220303,0.));
#11550=DIRECTION('',(0.,0.,1.));
#11551=DIRECTION('center_axis',(0.,0.,-1.));
#11552=DIRECTION('ref_axis',(1.,0.,0.));
#11553=DIRECTION('center_axis',(0.,0.,1.));
#11554=DIRECTION('ref_axis',(1.,0.,0.));
#11555=DIRECTION('',(0.,0.,1.));
#11556=DIRECTION('center_axis',(0.,0.,1.));
#11557=DIRECTION('ref_axis',(1.,0.,0.));
#11558=DIRECTION('',(0.,0.,1.));
#11559=DIRECTION('center_axis',(0.,0.,1.));
#11560=DIRECTION('ref_axis',(0.936891240421608,0.349620942766964,0.));
#11561=DIRECTION('',(0.,0.,1.));
#11562=DIRECTION('center_axis',(0.,0.,-1.));
#11563=DIRECTION('ref_axis',(1.,0.,0.));
#11564=DIRECTION('center_axis',(0.,0.,1.));
#11565=DIRECTION('ref_axis',(1.,3.79078190120237E-16,0.));
#11566=DIRECTION('',(1.22464679914735E-16,6.14212870423506E-32,1.));
#11567=DIRECTION('center_axis',(0.,0.,-1.));
#11568=DIRECTION('ref_axis',(1.,3.79078190120237E-16,0.));
#11569=DIRECTION('center_axis',(0.,0.,1.));
#11570=DIRECTION('ref_axis',(1.,3.79078190120237E-16,0.));
#11571=DIRECTION('',(1.22464679914735E-16,6.14212870423506E-32,1.));
#11572=DIRECTION('center_axis',(0.,0.,1.));
#11573=DIRECTION('ref_axis',(1.,3.79078190120237E-16,0.));
#11574=DIRECTION('',(1.22464679914735E-16,6.14212870423506E-32,1.));
#11575=DIRECTION('center_axis',(0.,0.,1.));
#11576=DIRECTION('ref_axis',(-0.608868431756822,0.793271222729016,0.));
#11577=DIRECTION('',(1.22464679914735E-16,6.14212870423506E-32,1.));
#11578=DIRECTION('center_axis',(0.,0.,1.));
#11579=DIRECTION('ref_axis',(1.,3.79078190120237E-16,0.));
#11580=DIRECTION('center_axis',(0.,0.,1.));
#11581=DIRECTION('ref_axis',(1.,3.79078190120237E-16,0.));
#11582=DIRECTION('center_axis',(0.,0.,1.));
#11583=DIRECTION('ref_axis',(1.,0.,0.));
#11584=DIRECTION('',(0.5,0.866025403784439,0.));
#11585=DIRECTION('',(-0.5,0.866025403784439,0.));
#11586=DIRECTION('',(-1.,0.,0.));
#11587=DIRECTION('',(-0.5,-0.866025403784439,0.));
#11588=DIRECTION('',(0.499999999999999,-0.866025403784439,0.));
#11589=DIRECTION('',(1.,-2.13662520709285E-16,0.));
#11590=DIRECTION('center_axis',(0.,0.,1.));
#11591=DIRECTION('ref_axis',(1.,0.,0.));
#11592=DIRECTION('center_axis',(-2.13662520709285E-16,-1.,0.));
#11593=DIRECTION('ref_axis',(1.,-2.13662520709285E-16,0.));
#11594=DIRECTION('',(1.,-2.13662520709285E-16,0.));
#11595=DIRECTION('',(0.,0.,1.));
#11596=DIRECTION('',(0.,0.,1.));
#11597=DIRECTION('center_axis',(-0.866025403784439,-0.499999999999999,0.));
#11598=DIRECTION('ref_axis',(0.499999999999999,-0.866025403784439,0.));
#11599=DIRECTION('',(0.499999999999999,-0.866025403784439,0.));
#11600=DIRECTION('',(0.,0.,1.));
#11601=DIRECTION('center_axis',(-0.866025403784439,0.5,0.));
#11602=DIRECTION('ref_axis',(-0.5,-0.866025403784439,0.));
#11603=DIRECTION('',(-0.5,-0.866025403784439,0.));
#11604=DIRECTION('',(0.,0.,1.));
#11605=DIRECTION('center_axis',(0.,1.,0.));
#11606=DIRECTION('ref_axis',(-1.,0.,0.));
#11607=DIRECTION('',(-1.,0.,0.));
#11608=DIRECTION('',(0.,0.,1.));
#11609=DIRECTION('center_axis',(0.866025403784439,0.5,0.));
#11610=DIRECTION('ref_axis',(-0.5,0.866025403784439,0.));
#11611=DIRECTION('',(-0.5,0.866025403784439,0.));
#11612=DIRECTION('',(0.,0.,1.));
#11613=DIRECTION('center_axis',(0.866025403784439,-0.5,0.));
#11614=DIRECTION('ref_axis',(0.5,0.866025403784439,0.));
#11615=DIRECTION('',(0.5,0.866025403784439,0.));
#11616=DIRECTION('center_axis',(0.,0.,1.));
#11617=DIRECTION('ref_axis',(1.,0.,0.));
#11618=DIRECTION('',(0.,0.,1.));
#11619=DIRECTION('',(1.,0.,0.));
#11620=DIRECTION('axis',(0.,0.,1.));
#11621=DIRECTION('refdir',(1.,0.,0.));
#11622=DIRECTION('axis',(0.,0.,1.));
#11623=DIRECTION('refdir',(1.,0.,0.));
#11624=DIRECTION('center_axis',(0.,0.,1.));
#11625=DIRECTION('ref_axis',(-0.349613253226052,-0.936894109901805,0.));
#11626=DIRECTION('',(0.,0.,1.));
#11627=DIRECTION('center_axis',(0.,0.,-1.));
#11628=DIRECTION('ref_axis',(1.,0.,0.));
#11629=DIRECTION('center_axis',(0.,0.,1.));
#11630=DIRECTION('ref_axis',(1.,0.,0.));
#11631=DIRECTION('',(0.,0.,1.));
#11632=DIRECTION('center_axis',(0.,0.,1.));
#11633=DIRECTION('ref_axis',(1.,0.,0.));
#11634=DIRECTION('',(0.,0.,1.));
#11635=DIRECTION('center_axis',(0.,0.,1.));
#11636=DIRECTION('ref_axis',(0.936891223524395,0.349620988047003,0.));
#11637=DIRECTION('',(0.,0.,1.));
#11638=DIRECTION('center_axis',(0.,0.,-1.));
#11639=DIRECTION('ref_axis',(1.,0.,0.));
#11640=DIRECTION('center_axis',(0.,0.,1.));
#11641=DIRECTION('ref_axis',(1.,3.79078190120237E-16,0.));
#11642=DIRECTION('',(1.22464679914735E-16,6.14212870423506E-32,1.));
#11643=DIRECTION('center_axis',(0.,0.,-1.));
#11644=DIRECTION('ref_axis',(1.,3.79078190120237E-16,0.));
#11645=DIRECTION('center_axis',(0.,0.,1.));
#11646=DIRECTION('ref_axis',(1.,3.79078190120237E-16,0.));
#11647=DIRECTION('',(1.22464679914735E-16,6.14212870423506E-32,1.));
#11648=DIRECTION('center_axis',(0.,0.,1.));
#11649=DIRECTION('ref_axis',(1.,3.79078190120237E-16,0.));
#11650=DIRECTION('',(1.22464679914735E-16,6.14212870423506E-32,1.));
#11651=DIRECTION('center_axis',(0.,0.,1.));
#11652=DIRECTION('ref_axis',(-0.608868629140097,0.79327107122916,0.));
#11653=DIRECTION('',(1.22464679914735E-16,6.14212870423506E-32,1.));
#11654=DIRECTION('center_axis',(0.,0.,1.));
#11655=DIRECTION('ref_axis',(1.,3.79078190120237E-16,0.));
#11656=DIRECTION('center_axis',(0.,0.,1.));
#11657=DIRECTION('ref_axis',(1.,3.79078190120237E-16,0.));
#11658=DIRECTION('center_axis',(0.,0.,1.));
#11659=DIRECTION('ref_axis',(1.,0.,0.));
#11660=DIRECTION('',(0.5,0.866025403784439,0.));
#11661=DIRECTION('',(-0.5,0.866025403784439,0.));
#11662=DIRECTION('',(-1.,0.,0.));
#11663=DIRECTION('',(-0.5,-0.866025403784439,0.));
#11664=DIRECTION('',(0.499999999999999,-0.866025403784439,0.));
#11665=DIRECTION('',(1.,-2.13662520709285E-16,0.));
#11666=DIRECTION('center_axis',(0.,0.,1.));
#11667=DIRECTION('ref_axis',(1.,0.,0.));
#11668=DIRECTION('center_axis',(-2.13662520709285E-16,-1.,0.));
#11669=DIRECTION('ref_axis',(1.,-2.13662520709285E-16,0.));
#11670=DIRECTION('',(1.,-2.13662520709285E-16,0.));
#11671=DIRECTION('',(0.,0.,1.));
#11672=DIRECTION('',(0.,0.,1.));
#11673=DIRECTION('center_axis',(-0.866025403784439,-0.499999999999999,0.));
#11674=DIRECTION('ref_axis',(0.499999999999999,-0.866025403784439,0.));
#11675=DIRECTION('',(0.499999999999999,-0.866025403784439,0.));
#11676=DIRECTION('',(0.,0.,1.));
#11677=DIRECTION('center_axis',(-0.866025403784439,0.5,0.));
#11678=DIRECTION('ref_axis',(-0.5,-0.866025403784439,0.));
#11679=DIRECTION('',(-0.5,-0.866025403784439,0.));
#11680=DIRECTION('',(0.,0.,1.));
#11681=DIRECTION('center_axis',(0.,1.,0.));
#11682=DIRECTION('ref_axis',(-1.,0.,0.));
#11683=DIRECTION('',(-1.,0.,0.));
#11684=DIRECTION('',(0.,0.,1.));
#11685=DIRECTION('center_axis',(0.866025403784439,0.5,0.));
#11686=DIRECTION('ref_axis',(-0.5,0.866025403784439,0.));
#11687=DIRECTION('',(-0.5,0.866025403784439,0.));
#11688=DIRECTION('',(0.,0.,1.));
#11689=DIRECTION('center_axis',(0.866025403784439,-0.5,0.));
#11690=DIRECTION('ref_axis',(0.5,0.866025403784439,0.));
#11691=DIRECTION('',(0.5,0.866025403784439,0.));
#11692=DIRECTION('center_axis',(0.,0.,1.));
#11693=DIRECTION('ref_axis',(1.,0.,0.));
#11694=DIRECTION('',(0.,0.,1.));
#11695=DIRECTION('',(1.,0.,0.));
#11696=DIRECTION('',(0.,0.,1.));
#11697=DIRECTION('',(1.,0.,0.));
#11698=DIRECTION('',(0.,0.,1.));
#11699=DIRECTION('',(1.,0.,0.));
#11700=DIRECTION('',(0.,0.,1.));
#11701=DIRECTION('',(1.,0.,0.));
#11702=DIRECTION('',(0.,0.,1.));
#11703=DIRECTION('',(1.,0.,0.));
#11704=DIRECTION('',(0.,0.,1.));
#11705=DIRECTION('',(1.,0.,0.));
#11706=CARTESIAN_POINT('',(0.,0.,0.));
#11707=CARTESIAN_POINT('',(0.,0.,0.));
#11708=CARTESIAN_POINT('',(0.,0.,0.));
#11709=CARTESIAN_POINT('Origin',(-6.3,-1.5,0.6));
#11710=CARTESIAN_POINT('',(-6.45,-1.5,0.6));
#11711=CARTESIAN_POINT('Origin',(-6.3,-1.5,0.6));
#11712=CARTESIAN_POINT('',(-6.45,-1.5,1.2));
#11713=CARTESIAN_POINT('',(-6.45,-1.5,0.6));
#11714=CARTESIAN_POINT('Origin',(-6.3,-1.5,1.2));
#11715=CARTESIAN_POINT('Origin',(-6.3,-1.5,0.6));
#11716=CARTESIAN_POINT('Origin',(-10.7,1.5,0.6));
#11717=CARTESIAN_POINT('',(-10.85,1.5,0.6));
#11718=CARTESIAN_POINT('Origin',(-10.7,1.5,0.6));
#11719=CARTESIAN_POINT('',(-10.85,1.5,1.2));
#11720=CARTESIAN_POINT('',(-10.85,1.5,0.6));
#11721=CARTESIAN_POINT('Origin',(-10.7,1.5,1.2));
#11722=CARTESIAN_POINT('Origin',(-10.7,1.5,0.6));
#11723=CARTESIAN_POINT('Origin',(-11.5,3.67394039744206E-16,-0.1));
#11724=CARTESIAN_POINT('',(-11.75,3.36777869765522E-16,0.));
#11725=CARTESIAN_POINT('Origin',(-11.5,3.67394039744206E-16,0.));
#11726=CARTESIAN_POINT('',(-11.75,3.9801020972289E-16,1.2));
#11727=CARTESIAN_POINT('',(-11.75,3.36777869765522E-16,-0.1));
#11728=CARTESIAN_POINT('Origin',(-11.5,3.67394039744206E-16,1.2));
#11729=CARTESIAN_POINT('Origin',(-8.5,3.,-0.1));
#11730=CARTESIAN_POINT('',(-8.75,3.,0.));
#11731=CARTESIAN_POINT('Origin',(-8.5,3.,0.));
#11732=CARTESIAN_POINT('',(-8.75,3.,1.2));
#11733=CARTESIAN_POINT('',(-8.75,3.,-0.1));
#11734=CARTESIAN_POINT('Origin',(-8.5,3.,1.2));
#11735=CARTESIAN_POINT('Origin',(-5.5,0.,-0.1));
#11736=CARTESIAN_POINT('',(-5.75,-3.06161699786838E-17,0.));
#11737=CARTESIAN_POINT('Origin',(-5.5,0.,0.));
#11738=CARTESIAN_POINT('',(-5.75,3.06161699786838E-17,1.2));
#11739=CARTESIAN_POINT('',(-5.75,-3.06161699786838E-17,-0.1));
#11740=CARTESIAN_POINT('Origin',(-5.5,0.,1.2));
#11741=CARTESIAN_POINT('Origin',(-8.5,-3.,-0.1));
#11742=CARTESIAN_POINT('',(-8.75,-3.,0.));
#11743=CARTESIAN_POINT('Origin',(-8.5,-3.,0.));
#11744=CARTESIAN_POINT('',(-8.75,-3.,1.2));
#11745=CARTESIAN_POINT('',(-8.75,-3.,-0.1));
#11746=CARTESIAN_POINT('Origin',(-8.5,-3.,1.2));
#11747=CARTESIAN_POINT('Origin',(6.5,7.,0.));
#11748=CARTESIAN_POINT('',(6.5,7.,0.));
#11749=CARTESIAN_POINT('',(-13.5,7.,0.));
#11750=CARTESIAN_POINT('',(6.5,7.,0.));
#11751=CARTESIAN_POINT('',(-13.5,7.,1.2));
#11752=CARTESIAN_POINT('',(-13.5,7.,0.));
#11753=CARTESIAN_POINT('',(6.5,7.,1.2));
#11754=CARTESIAN_POINT('',(6.5,7.,1.2));
#11755=CARTESIAN_POINT('',(6.5,7.,0.));
#11756=CARTESIAN_POINT('Origin',(6.5,-7.,0.));
#11757=CARTESIAN_POINT('',(6.5,-7.,0.));
#11758=CARTESIAN_POINT('',(6.5,-7.,0.));
#11759=CARTESIAN_POINT('',(6.5,-7.,1.2));
#11760=CARTESIAN_POINT('',(6.5,-7.,1.2));
#11761=CARTESIAN_POINT('',(6.5,-7.,0.));
#11762=CARTESIAN_POINT('Origin',(-13.5,-7.,0.));
#11763=CARTESIAN_POINT('',(-13.5,-7.,0.));
#11764=CARTESIAN_POINT('',(-13.5,-7.,0.));
#11765=CARTESIAN_POINT('',(-13.5,-7.,1.2));
#11766=CARTESIAN_POINT('',(-13.5,-7.,1.2));
#11767=CARTESIAN_POINT('',(-13.5,-7.,0.));
#11768=CARTESIAN_POINT('Origin',(-13.5,7.,0.));
#11769=CARTESIAN_POINT('',(-13.5,7.,0.));
#11770=CARTESIAN_POINT('',(-13.5,7.,1.2));
#11771=CARTESIAN_POINT('Origin',(-3.5,0.,1.2));
#11772=CARTESIAN_POINT('Origin',(-3.5,0.,0.));
#11773=CARTESIAN_POINT('',(0.,0.,0.));
#11774=CARTESIAN_POINT('Origin',(-8.5,0.,1.8));
#11775=CARTESIAN_POINT('',(-9.68946857590504,0.000315360110501401,1.89626312369518));
#11776=CARTESIAN_POINT('',(-9.68870505254289,0.000360304848219705,1.85373687630491));
#11777=CARTESIAN_POINT('',(-9.688225,-1.45515594291686E-16,1.8));
#11778=CARTESIAN_POINT('',(-7.98816118883252,1.07233375495116,1.8));
#11779=CARTESIAN_POINT('Ctrl Pts',(-9.688225,1.66533453693773E-15,1.89626312369518));
#11780=CARTESIAN_POINT('Ctrl Pts',(-9.688225,0.298712821306094,1.88425993690586));
#11781=CARTESIAN_POINT('Ctrl Pts',(-9.57054245632586,0.595858078271529,
1.87225675011654));
#11782=CARTESIAN_POINT('Ctrl Pts',(-9.36601586214935,0.813569405232719,
1.86025356332722));
#11783=CARTESIAN_POINT('Ctrl Pts',(-9.16148926797284,1.03128073219391,1.8482503765379));
#11784=CARTESIAN_POINT('Ctrl Pts',(-8.87226522412846,1.16727314847136,1.83624718974859));
#11785=CARTESIAN_POINT('Ctrl Pts',(-8.57413435701451,1.1859100926019,1.82424400295927));
#11786=CARTESIAN_POINT('Ctrl Pts',(-8.37341306103911,1.1984577084027,1.81616266863951));
#11787=CARTESIAN_POINT('Ctrl Pts',(-8.16965911380568,1.15896506886691,1.80808133431976));
#11788=CARTESIAN_POINT('Ctrl Pts',(-7.98816118883253,1.07233375495117,1.8));
#11789=CARTESIAN_POINT('',(-9.0118388111672,1.0723337549513,1.8));
#11790=CARTESIAN_POINT('Origin',(-8.5,0.,1.8));
#11791=CARTESIAN_POINT('Ctrl Pts',(-9.0118388111672,1.0723337549513,1.79999999999999));
#11792=CARTESIAN_POINT('Ctrl Pts',(-9.19046954816081,0.987070987050382,
1.8079536705758));
#11793=CARTESIAN_POINT('Ctrl Pts',(-9.34601190633409,0.856319638879147,
1.81590734115161));
#11794=CARTESIAN_POINT('Ctrl Pts',(-9.46235005017619,0.695941065062742,
1.82386101172742));
#11795=CARTESIAN_POINT('Ctrl Pts',(-9.57868819401829,0.535562491246337,
1.83181468230323));
#11796=CARTESIAN_POINT('Ctrl Pts',(-9.6558221235292,0.345556691784764,1.83976835287904));
#11797=CARTESIAN_POINT('Ctrl Pts',(-9.68019148863806,0.149449620287358,
1.84772202345485));
#11798=CARTESIAN_POINT('Ctrl Pts',(-9.68633448654835,0.10001520437127,1.84972697440487));
#11799=CARTESIAN_POINT('Ctrl Pts',(-9.68912463030123,0.0501930912280235,
1.85173192535489));
#11800=CARTESIAN_POINT('Ctrl Pts',(-9.68870505254289,0.000360304848219705,
1.85373687630491));
#11801=CARTESIAN_POINT('Origin',(-8.5,0.,1.8));
#11802=CARTESIAN_POINT('',(-9.68793925643297,0.00019677074638643,2.19626312369517));
#11803=CARTESIAN_POINT('',(-9.68748917149883,0.000243143348928272,2.15373687630491));
#11804=CARTESIAN_POINT('',(-9.688225,-1.45515594291686E-16,1.8));
#11805=CARTESIAN_POINT('Ctrl Pts',(-9.6874734085738,0.00051756617809895,
2.19626312369517));
#11806=CARTESIAN_POINT('Ctrl Pts',(-9.68805588513481,0.151871918451282,
2.19019552440188));
#11807=CARTESIAN_POINT('Ctrl Pts',(-9.66063518694746,0.302992792078646,
2.18412792510859));
#11808=CARTESIAN_POINT('Ctrl Pts',(-9.60441870150575,0.442514540719334,
2.1780603258153));
#11809=CARTESIAN_POINT('Ctrl Pts',(-9.45703671910369,0.808296779528733,
2.16215298466368));
#11810=CARTESIAN_POINT('Ctrl Pts',(-9.1117344267537,1.09435546738227,2.14624564351206));
#11811=CARTESIAN_POINT('Ctrl Pts',(-8.7250756969201,1.1688514604035,2.13033830236044));
#11812=CARTESIAN_POINT('Ctrl Pts',(-8.33841696708651,1.24334745342473,2.11443096120882));
#11813=CARTESIAN_POINT('Ctrl Pts',(-7.91040179976933,1.10628075161366,2.0985236200572));
#11814=CARTESIAN_POINT('Ctrl Pts',(-7.6383599938754,0.821043330033441,2.08261627890558));
#11815=CARTESIAN_POINT('Ctrl Pts',(-7.36631818798147,0.535805908453222,
2.06670893775396));
#11816=CARTESIAN_POINT('Ctrl Pts',(-7.25024974351079,0.102397767103854,
2.05080159660234));
#11817=CARTESIAN_POINT('Ctrl Pts',(-7.34335808136087,-0.28060568798053,
2.03489425545072));
#11818=CARTESIAN_POINT('Ctrl Pts',(-7.43646641921094,-0.663609143064914,
2.0189869142991));
#11819=CARTESIAN_POINT('Ctrl Pts',(-7.73875153938177,-0.996207911884313,
2.00307957314748));
#11820=CARTESIAN_POINT('Ctrl Pts',(-8.11087993218691,-1.12491486892692,
1.98717223199585));
#11821=CARTESIAN_POINT('Ctrl Pts',(-8.48300832499204,-1.25362182596952,
1.97126489084423));
#11822=CARTESIAN_POINT('Ctrl Pts',(-8.92497999043149,-1.17843697123532,
1.95535754969261));
#11823=CARTESIAN_POINT('Ctrl Pts',(-9.23549131184823,-0.935203778959572,
1.93945020854099));
#11824=CARTESIAN_POINT('Ctrl Pts',(-9.3907469725566,-0.813587182821698,
1.93149653796518));
#11825=CARTESIAN_POINT('Ctrl Pts',(-9.5131375472593,-0.649958502298435,
1.92354286738937));
#11826=CARTESIAN_POINT('Ctrl Pts',(-9.59128485561407,-0.46747485804336,
1.91558919681356));
#11827=CARTESIAN_POINT('Ctrl Pts',(-9.65457976584342,-0.319673403014159,
1.90914717244076));
#11828=CARTESIAN_POINT('Ctrl Pts',(-9.68885071316148,-0.159502929754193,
1.90270514806797));
#11829=CARTESIAN_POINT('Ctrl Pts',(-9.68946857590504,0.000315360110501401,
1.89626312369518));
#11830=CARTESIAN_POINT('Ctrl Pts',(-9.68870505254289,0.000360304848219705,
1.85373687630491));
#11831=CARTESIAN_POINT('Ctrl Pts',(-9.68579568774457,-0.345181735009932,
1.86763926650651));
#11832=CARTESIAN_POINT('Ctrl Pts',(-9.52856043097317,-0.691236952334183,
1.88154165670811));
#11833=CARTESIAN_POINT('Ctrl Pts',(-9.26471878006929,-0.912107988881616,
1.89544404690971));
#11834=CARTESIAN_POINT('Ctrl Pts',(-8.96282686867327,-1.16483222391764,
1.91135138806133));
#11835=CARTESIAN_POINT('Ctrl Pts',(-8.5213625732717,-1.25366146285155,1.92725872921295));
#11836=CARTESIAN_POINT('Ctrl Pts',(-8.1453201794112,-1.13646221921786,1.94316607036457));
#11837=CARTESIAN_POINT('Ctrl Pts',(-7.7692777855507,-1.01926297558418,1.95907341151619));
#11838=CARTESIAN_POINT('Ctrl Pts',(-7.45865729323126,-0.69603524938291,
1.97498075266782));
#11839=CARTESIAN_POINT('Ctrl Pts',(-7.35313075502305,-0.316068910845257,
1.99088809381944));
#11840=CARTESIAN_POINT('Ctrl Pts',(-7.30036748591894,-0.126085741576431,
1.99884176439525));
#11841=CARTESIAN_POINT('Ctrl Pts',(-7.29887770534264,0.0780820807764889,
2.00679543497106));
#11842=CARTESIAN_POINT('Ctrl Pts',(-7.34422871925985,0.271345030563532,
2.01474910554687));
#11843=CARTESIAN_POINT('Ctrl Pts',(-7.38957973317705,0.464607980350577,
2.02270277612268));
#11844=CARTESIAN_POINT('Ctrl Pts',(-7.48177154158776,0.646966057571745,
2.03065644669849));
#11845=CARTESIAN_POINT('Ctrl Pts',(-7.6136099013672,0.793641084515056,2.0386101172743));
#11846=CARTESIAN_POINT('Ctrl Pts',(-7.87728662092608,1.08699113840168,2.05451745842592));
#11847=CARTESIAN_POINT('Ctrl Pts',(-8.29954954595991,1.23760899117687,2.07042479957754));
#11848=CARTESIAN_POINT('Ctrl Pts',(-8.68834880695705,1.1753180915929,2.08633214072916));
#11849=CARTESIAN_POINT('Ctrl Pts',(-9.07714806795419,1.11302719200893,2.10223948188078));
#11850=CARTESIAN_POINT('Ctrl Pts',(-9.43248366491464,0.837827540065792,
2.1181468230324));
#11851=CARTESIAN_POINT('Ctrl Pts',(-9.59053795470158,0.476746315597217,
2.13405416418402));
#11852=CARTESIAN_POINT('Ctrl Pts',(-9.65572666339682,0.327820153650373,
2.14061506822432));
#11853=CARTESIAN_POINT('Ctrl Pts',(-9.6873556683552,0.164284598792956,2.14717597226461));
#11854=CARTESIAN_POINT('Ctrl Pts',(-9.68668762773837,0.000508001308789992,
2.1537368763049));
#11855=CARTESIAN_POINT('Origin',(-8.5,0.,1.8));
#11856=CARTESIAN_POINT('',(-9.688225,-8.88178419700125E-16,2.49626312369518));
#11857=CARTESIAN_POINT('',(-9.68781667187452,-0.000480474173583903,2.45373687630491));
#11858=CARTESIAN_POINT('',(-9.688225,-1.45515594291686E-16,1.8));
#11859=CARTESIAN_POINT('Ctrl Pts',(-9.688225,-8.88178419700125E-16,2.49626312369518));
#11860=CARTESIAN_POINT('Ctrl Pts',(-9.688225,0.298712821306089,2.48425993690586));
#11861=CARTESIAN_POINT('Ctrl Pts',(-9.57054245632587,0.595858078271521,
2.47225675011654));
#11862=CARTESIAN_POINT('Ctrl Pts',(-9.36601586214936,0.813569405232711,
2.46025356332722));
#11863=CARTESIAN_POINT('Ctrl Pts',(-9.16148926797285,1.0312807321939,2.4482503765379));
#11864=CARTESIAN_POINT('Ctrl Pts',(-8.87226522412848,1.16727314847135,2.43624718974859));
#11865=CARTESIAN_POINT('Ctrl Pts',(-8.57413435701453,1.1859100926019,2.42424400295927));
#11866=CARTESIAN_POINT('Ctrl Pts',(-8.27600348990057,1.20454703673245,2.41224081616995));
#11867=CARTESIAN_POINT('Ctrl Pts',(-7.97209482032098,1.10563290540111,2.40023762938063));
#11868=CARTESIAN_POINT('Ctrl Pts',(-7.74204705372066,0.915087963996611,
2.38823444259132));
#11869=CARTESIAN_POINT('Ctrl Pts',(-7.51199928712033,0.724543022592107,
2.376231255802));
#11870=CARTESIAN_POINT('Ctrl Pts',(-7.35822688079637,0.444367128061535,
2.36422806901268));
#11871=CARTESIAN_POINT('Ctrl Pts',(-7.32102560975818,0.147979855990369,
2.35222488222336));
#11872=CARTESIAN_POINT('Ctrl Pts',(-7.28382433871999,-0.148407416080797,
2.34022169543405));
#11873=CARTESIAN_POINT('Ctrl Pts',(-7.36358464744633,-0.457895344721877,
2.32821850864473));
#11874=CARTESIAN_POINT('Ctrl Pts',(-7.53940549437877,-0.699383189957625,
2.31621532185541));
#11875=CARTESIAN_POINT('Ctrl Pts',(-7.71522634131121,-0.940871035193373,
2.30421213506609));
#11876=CARTESIAN_POINT('Ctrl Pts',(-7.98526240565775,-1.11182427083078,
2.29220894827677));
#11877=CARTESIAN_POINT('Ctrl Pts',(-8.27875123560107,-1.16744491727745,
2.28020576148746));
#11878=CARTESIAN_POINT('Ctrl Pts',(-8.57224006554438,-1.22306556372412,
2.26820257469814));
#11879=CARTESIAN_POINT('Ctrl Pts',(-8.8861013605993,-1.16276985667028,2.25619938790882));
#11880=CARTESIAN_POINT('Ctrl Pts',(-9.13808834820084,-1.00235817476355,
2.2441962011195));
#11881=CARTESIAN_POINT('Ctrl Pts',(-9.39007533580238,-0.841946492856832,
2.23219301433019));
#11882=CARTESIAN_POINT('Ctrl Pts',(-9.5775432964213,-0.583102430603028,
2.22018982754087));
#11883=CARTESIAN_POINT('Ctrl Pts',(-9.65136659729188,-0.293655596346343,
2.20818664075155));
#11884=CARTESIAN_POINT('Ctrl Pts',(-9.67581103310541,-0.197813707972594,
2.20421213506609));
#11885=CARTESIAN_POINT('Ctrl Pts',(-9.688225,-0.0989100500924339,2.20023762938063));
#11886=CARTESIAN_POINT('Ctrl Pts',(-9.688225,2.99760216648792E-15,2.19626312369518));
#11887=CARTESIAN_POINT('Ctrl Pts',(-9.688225,-1.74171788103195E-12,2.15373687630491));
#11888=CARTESIAN_POINT('Ctrl Pts',(-9.68822499999956,-0.298712821307831,
2.16574006309422));
#11889=CARTESIAN_POINT('Ctrl Pts',(-9.57054245632499,-0.595858078273089,
2.17774324988354));
#11890=CARTESIAN_POINT('Ctrl Pts',(-9.36601586214817,-0.813569405233979,
2.18974643667286));
#11891=CARTESIAN_POINT('Ctrl Pts',(-9.16148926797134,-1.03128073219487,
2.20174962346218));
#11892=CARTESIAN_POINT('Ctrl Pts',(-8.87226522412677,-1.16727314847189,
2.2137528102515));
#11893=CARTESIAN_POINT('Ctrl Pts',(-8.57413435701279,-1.18591009260201,
2.22575599704081));
#11894=CARTESIAN_POINT('Ctrl Pts',(-8.27600348989881,-1.20454703673212,
2.23775918383013));
#11895=CARTESIAN_POINT('Ctrl Pts',(-7.97209482031937,-1.10563290540034,
2.24976237061945));
#11896=CARTESIAN_POINT('Ctrl Pts',(-7.74204705371932,-0.915087963995503,
2.26176555740877));
#11897=CARTESIAN_POINT('Ctrl Pts',(-7.51199928711927,-0.724543022590664,
2.27376874419808));
#11898=CARTESIAN_POINT('Ctrl Pts',(-7.35822688079572,-0.444367128059868,
2.2857719309874));
#11899=CARTESIAN_POINT('Ctrl Pts',(-7.32102560975796,-0.147979855988648,
2.29777511777672));
#11900=CARTESIAN_POINT('Ctrl Pts',(-7.28382433872021,0.148407416082571,
2.30977830456604));
#11901=CARTESIAN_POINT('Ctrl Pts',(-7.363584647447,0.457895344723534,2.32178149135536));
#11902=CARTESIAN_POINT('Ctrl Pts',(-7.53940549437979,0.699383189959025,
2.33378467814467));
#11903=CARTESIAN_POINT('Ctrl Pts',(-7.71522634131258,0.940871035194516,
2.34578786493399));
#11904=CARTESIAN_POINT('Ctrl Pts',(-7.98526240565937,1.11182427083153,2.35779105172331));
#11905=CARTESIAN_POINT('Ctrl Pts',(-8.27875123560277,1.16744491727777,2.36979423851263));
#11906=CARTESIAN_POINT('Ctrl Pts',(-8.57224006554616,1.22306556372401,2.38179742530194));
#11907=CARTESIAN_POINT('Ctrl Pts',(-8.88610136060099,1.16276985666972,2.39380061209126));
#11908=CARTESIAN_POINT('Ctrl Pts',(-9.1380883482023,1.00235817476263,2.40580379888058));
#11909=CARTESIAN_POINT('Ctrl Pts',(-9.39007533580361,0.841946492855538,
2.4178069856699));
#11910=CARTESIAN_POINT('Ctrl Pts',(-9.57754329642215,0.583102430601462,
2.42981017245921));
#11911=CARTESIAN_POINT('Ctrl Pts',(-9.6513665972923,0.293655596344671,2.44181335924853));
#11912=CARTESIAN_POINT('Ctrl Pts',(-9.6758110331057,0.197813707970885,2.44578786493399));
#11913=CARTESIAN_POINT('Ctrl Pts',(-9.68822500000014,0.0989100500907039,
2.44976237061945));
#11914=CARTESIAN_POINT('Ctrl Pts',(-9.688225,-1.73505654288419E-12,2.45373687630491));
#11915=CARTESIAN_POINT('Origin',(-8.5,0.,1.8));
#11916=CARTESIAN_POINT('',(-9.688225,-5.55111512312578E-16,2.79626312369518));
#11917=CARTESIAN_POINT('',(-9.68934581032131,-0.000146828966271381,2.75373687630491));
#11918=CARTESIAN_POINT('',(-9.688225,-1.45515594291686E-16,1.8));
#11919=CARTESIAN_POINT('Ctrl Pts',(-9.688225,3.66373598126302E-15,2.79626312369518));
#11920=CARTESIAN_POINT('Ctrl Pts',(-9.688225,0.298712821306094,2.78425993690586));
#11921=CARTESIAN_POINT('Ctrl Pts',(-9.57054245632586,0.595858078271526,
2.77225675011654));
#11922=CARTESIAN_POINT('Ctrl Pts',(-9.36601586214935,0.813569405232716,
2.76025356332722));
#11923=CARTESIAN_POINT('Ctrl Pts',(-9.16148926797284,1.03128073219391,2.7482503765379));
#11924=CARTESIAN_POINT('Ctrl Pts',(-8.87226522412847,1.16727314847135,2.73624718974859));
#11925=CARTESIAN_POINT('Ctrl Pts',(-8.57413435701452,1.1859100926019,2.72424400295927));
#11926=CARTESIAN_POINT('Ctrl Pts',(-8.27600348990056,1.20454703673245,2.71224081616995));
#11927=CARTESIAN_POINT('Ctrl Pts',(-7.97209482032097,1.10563290540111,2.70023762938063));
#11928=CARTESIAN_POINT('Ctrl Pts',(-7.74204705372065,0.915087963996604,
2.68823444259132));
#11929=CARTESIAN_POINT('Ctrl Pts',(-7.51199928712032,0.724543022592098,
2.676231255802));
#11930=CARTESIAN_POINT('Ctrl Pts',(-7.35822688079636,0.444367128061523,
2.66422806901268));
#11931=CARTESIAN_POINT('Ctrl Pts',(-7.32102560975818,0.147979855990356,
2.65222488222336));
#11932=CARTESIAN_POINT('Ctrl Pts',(-7.28382433871999,-0.148407416080811,
2.64022169543404));
#11933=CARTESIAN_POINT('Ctrl Pts',(-7.36358464744634,-0.457895344721891,
2.62821850864473));
#11934=CARTESIAN_POINT('Ctrl Pts',(-7.53940549437878,-0.699383189957637,
2.61621532185541));
#11935=CARTESIAN_POINT('Ctrl Pts',(-7.71522634131122,-0.940871035193383,
2.60421213506609));
#11936=CARTESIAN_POINT('Ctrl Pts',(-7.98526240565776,-1.11182427083079,
2.59220894827677));
#11937=CARTESIAN_POINT('Ctrl Pts',(-8.27875123560108,-1.16744491727745,
2.58020576148746));
#11938=CARTESIAN_POINT('Ctrl Pts',(-8.5722400655444,-1.22306556372411,2.56820257469814));
#11939=CARTESIAN_POINT('Ctrl Pts',(-8.88610136059931,-1.16276985667027,
2.55619938790882));
#11940=CARTESIAN_POINT('Ctrl Pts',(-9.13808834820086,-1.00235817476354,
2.5441962011195));
#11941=CARTESIAN_POINT('Ctrl Pts',(-9.3900753358024,-0.841946492856817,
2.53219301433018));
#11942=CARTESIAN_POINT('Ctrl Pts',(-9.57754329642131,-0.583102430603009,
2.52018982754087));
#11943=CARTESIAN_POINT('Ctrl Pts',(-9.65136659729188,-0.293655596346323,
2.50818664075155));
#11944=CARTESIAN_POINT('Ctrl Pts',(-9.67581103310541,-0.197813707972581,
2.50421213506609));
#11945=CARTESIAN_POINT('Ctrl Pts',(-9.688225,-0.0989100500924293,2.50023762938063));
#11946=CARTESIAN_POINT('Ctrl Pts',(-9.688225,-8.88178419700125E-16,2.49626312369518));
#11947=CARTESIAN_POINT('Ctrl Pts',(-9.68737088905248,-0.00100502077275876,
2.45373687630491));
#11948=CARTESIAN_POINT('Ctrl Pts',(-9.68829445628317,-0.120370390803603,
2.45852736032596));
#11949=CARTESIAN_POINT('Ctrl Pts',(-9.67170875826749,-0.239475692471852,
2.46331784434701));
#11950=CARTESIAN_POINT('Ctrl Pts',(-9.63652762380349,-0.352808501661884,
2.46810832836806));
#11951=CARTESIAN_POINT('Ctrl Pts',(-9.51970470871583,-0.729142845234637,
2.48401566951968));
#11952=CARTESIAN_POINT('Ctrl Pts',(-9.19783981952358,-1.04182698858073,
2.4999230106713));
#11953=CARTESIAN_POINT('Ctrl Pts',(-8.8180025015363,-1.14702407757865,2.51583035182292));
#11954=CARTESIAN_POINT('Ctrl Pts',(-8.43816518354902,-1.25222116657657,
2.53173769297454));
#11955=CARTESIAN_POINT('Ctrl Pts',(-8.00035543676671,-1.14993120122632,
2.54764503412616));
#11956=CARTESIAN_POINT('Ctrl Pts',(-7.70675772214978,-0.887471152741141,
2.56355237527778));
#11957=CARTESIAN_POINT('Ctrl Pts',(-7.41316000753286,-0.625011104255964,
2.5794597164294));
#11958=CARTESIAN_POINT('Ctrl Pts',(-7.26377432508131,-0.202380972635861,
2.59536705758103));
#11959=CARTESIAN_POINT('Ctrl Pts',(-7.32507248791809,0.187188402540279,
2.61127439873265));
#11960=CARTESIAN_POINT('Ctrl Pts',(-7.35572156933647,0.381973090128349,
2.61922806930846));
#11961=CARTESIAN_POINT('Ctrl Pts',(-7.43904161207694,0.568492588605429,
2.62718173988427));
#11962=CARTESIAN_POINT('Ctrl Pts',(-7.56040023003843,0.725635480344461,
2.63513541046008));
#11963=CARTESIAN_POINT('Ctrl Pts',(-7.68175884799992,0.882778372083494,
2.64308908103589));
#11964=CARTESIAN_POINT('Ctrl Pts',(-7.84115604118242,1.01054465708448,2.6510427516117));
#11965=CARTESIAN_POINT('Ctrl Pts',(-8.02186533941589,1.08944057941184,2.65899642218751));
#11966=CARTESIAN_POINT('Ctrl Pts',(-8.38328393588282,1.24723242406657,2.67490376333913));
#11967=CARTESIAN_POINT('Ctrl Pts',(-8.8299509525536,1.2095428180268,2.69081110449075));
#11968=CARTESIAN_POINT('Ctrl Pts',(-9.15810856599484,0.991832674325304,
2.70671844564237));
#11969=CARTESIAN_POINT('Ctrl Pts',(-9.48142796607357,0.777332354450122,
2.72239125586322));
#11970=CARTESIAN_POINT('Ctrl Pts',(-9.68970670457596,0.38808065463741,2.73806406608406));
#11971=CARTESIAN_POINT('Ctrl Pts',(-9.69027298352254,-0.000268290982180393,
2.7537368763049));
#11972=CARTESIAN_POINT('Origin',(-8.5,0.,1.8));
#11973=CARTESIAN_POINT('',(-9.688225,-3.33066907387547E-16,3.09626312369518));
#11974=CARTESIAN_POINT('',(-9.688225,-1.73872027886546E-12,3.05373687630491));
#11975=CARTESIAN_POINT('',(-9.688225,-1.45515594291686E-16,1.8));
#11976=CARTESIAN_POINT('Ctrl Pts',(-9.688225,-4.55191440096314E-15,3.09626312369518));
#11977=CARTESIAN_POINT('Ctrl Pts',(-9.688225,0.298712821306082,3.08425993690586));
#11978=CARTESIAN_POINT('Ctrl Pts',(-9.57054245632587,0.595858078271511,
3.07225675011654));
#11979=CARTESIAN_POINT('Ctrl Pts',(-9.36601586214937,0.813569405232701,
3.06025356332722));
#11980=CARTESIAN_POINT('Ctrl Pts',(-9.16148926797286,1.03128073219389,3.04825037653791));
#11981=CARTESIAN_POINT('Ctrl Pts',(-8.8722652241285,1.16727314847134,3.03624718974859));
#11982=CARTESIAN_POINT('Ctrl Pts',(-8.57413435701455,1.1859100926019,3.02424400295927));
#11983=CARTESIAN_POINT('Ctrl Pts',(-8.2760034899006,1.20454703673245,3.01224081616995));
#11984=CARTESIAN_POINT('Ctrl Pts',(-7.97209482032101,1.10563290540113,3.00023762938064));
#11985=CARTESIAN_POINT('Ctrl Pts',(-7.74204705372068,0.915087963996633,
2.98823444259132));
#11986=CARTESIAN_POINT('Ctrl Pts',(-7.51199928712035,0.724543022592139,
2.976231255802));
#11987=CARTESIAN_POINT('Ctrl Pts',(-7.35822688079639,0.444367128061575,
2.96422806901268));
#11988=CARTESIAN_POINT('Ctrl Pts',(-7.32102560975819,0.147979855990414,
2.95222488222336));
#11989=CARTESIAN_POINT('Ctrl Pts',(-7.28382433871999,-0.148407416080746,
2.94022169543405));
#11990=CARTESIAN_POINT('Ctrl Pts',(-7.36358464744631,-0.457895344721826,
2.92821850864473));
#11991=CARTESIAN_POINT('Ctrl Pts',(-7.53940549437874,-0.69938318995758,
2.91621532185541));
#11992=CARTESIAN_POINT('Ctrl Pts',(-7.71522634131116,-0.940871035193333,
2.90421213506609));
#11993=CARTESIAN_POINT('Ctrl Pts',(-7.98526240565769,-1.11182427083075,
2.89220894827678));
#11994=CARTESIAN_POINT('Ctrl Pts',(-8.278751235601,-1.16744491727744,2.88020576148746));
#11995=CARTESIAN_POINT('Ctrl Pts',(-8.57224006554431,-1.22306556372412,
2.86820257469814));
#11996=CARTESIAN_POINT('Ctrl Pts',(-8.88610136059922,-1.1627698566703,2.85619938790882));
#11997=CARTESIAN_POINT('Ctrl Pts',(-9.13808834820077,-1.0023581747636,2.84419620111951));
#11998=CARTESIAN_POINT('Ctrl Pts',(-9.39007533580233,-0.841946492856892,
2.83219301433019));
#11999=CARTESIAN_POINT('Ctrl Pts',(-9.57754329642126,-0.583102430603105,
2.82018982754087));
#12000=CARTESIAN_POINT('Ctrl Pts',(-9.65136659729185,-0.293655596346429,
2.80818664075155));
#12001=CARTESIAN_POINT('Ctrl Pts',(-9.67581103310541,-0.197813707972653,
2.80421213506609));
#12002=CARTESIAN_POINT('Ctrl Pts',(-9.688225,-0.0989100500924628,2.80023762938063));
#12003=CARTESIAN_POINT('Ctrl Pts',(-9.688225,3.66373598126302E-15,2.79626312369518));
#12004=CARTESIAN_POINT('Ctrl Pts',(-9.688225,-1.73899783462161E-12,2.75373687630491));
#12005=CARTESIAN_POINT('Ctrl Pts',(-9.68822499999956,-0.298712821307831,
2.76574006309423));
#12006=CARTESIAN_POINT('Ctrl Pts',(-9.57054245632499,-0.595858078273093,
2.77774324988354));
#12007=CARTESIAN_POINT('Ctrl Pts',(-9.36601586214816,-0.813569405233984,
2.78974643667286));
#12008=CARTESIAN_POINT('Ctrl Pts',(-9.16148926797133,-1.03128073219487,
2.80174962346218));
#12009=CARTESIAN_POINT('Ctrl Pts',(-8.87226522412676,-1.1672731484719,2.8137528102515));
#12010=CARTESIAN_POINT('Ctrl Pts',(-8.57413435701278,-1.18591009260201,
2.82575599704081));
#12011=CARTESIAN_POINT('Ctrl Pts',(-8.27600348989879,-1.20454703673212,
2.83775918383013));
#12012=CARTESIAN_POINT('Ctrl Pts',(-7.97209482031935,-1.10563290540033,
2.84976237061945));
#12013=CARTESIAN_POINT('Ctrl Pts',(-7.7420470537193,-0.915087963995489,
2.86176555740877));
#12014=CARTESIAN_POINT('Ctrl Pts',(-7.51199928711925,-0.724543022590643,
2.87376874419809));
#12015=CARTESIAN_POINT('Ctrl Pts',(-7.35822688079571,-0.444367128059841,
2.8857719309874));
#12016=CARTESIAN_POINT('Ctrl Pts',(-7.32102560975796,-0.147979855988618,
2.89777511777672));
#12017=CARTESIAN_POINT('Ctrl Pts',(-7.28382433872021,0.148407416082605,
2.90977830456604));
#12018=CARTESIAN_POINT('Ctrl Pts',(-7.36358464744701,0.45789534472357,2.92178149135536));
#12019=CARTESIAN_POINT('Ctrl Pts',(-7.53940549437981,0.699383189959057,
2.93378467814467));
#12020=CARTESIAN_POINT('Ctrl Pts',(-7.71522634131261,0.940871035194545,
2.94578786493399));
#12021=CARTESIAN_POINT('Ctrl Pts',(-7.98526240565941,1.11182427083155,2.95779105172331));
#12022=CARTESIAN_POINT('Ctrl Pts',(-8.27875123560281,1.16744491727778,2.96979423851263));
#12023=CARTESIAN_POINT('Ctrl Pts',(-8.57224006554622,1.22306556372401,2.98179742530195));
#12024=CARTESIAN_POINT('Ctrl Pts',(-8.88610136060104,1.1627698566697,2.99380061209126));
#12025=CARTESIAN_POINT('Ctrl Pts',(-9.13808834820234,1.0023581747626,3.00580379888058));
#12026=CARTESIAN_POINT('Ctrl Pts',(-9.39007533580365,0.841946492855494,
3.0178069856699));
#12027=CARTESIAN_POINT('Ctrl Pts',(-9.57754329642218,0.583102430601406,
3.02981017245922));
#12028=CARTESIAN_POINT('Ctrl Pts',(-9.65136659729232,0.293655596344608,
3.04181335924854));
#12029=CARTESIAN_POINT('Ctrl Pts',(-9.67581103310571,0.197813707970839,
3.04578786493399));
#12030=CARTESIAN_POINT('Ctrl Pts',(-9.68822500000014,0.098910050090677,
3.04976237061945));
#12031=CARTESIAN_POINT('Ctrl Pts',(-9.688225,-1.74293912635903E-12,3.05373687630491));
#12032=CARTESIAN_POINT('Origin',(-8.5,0.,1.8));
#12033=CARTESIAN_POINT('',(-9.68741751198286,-6.04159293495165E-5,3.39626312369518));
#12034=CARTESIAN_POINT('',(-9.688225,-1.7384427231093E-12,3.35373687630491));
#12035=CARTESIAN_POINT('',(-9.688225,-1.45515594291686E-16,1.8));
#12036=CARTESIAN_POINT('Ctrl Pts',(-9.688225,-4.32986979603811E-15,3.39626312369518));
#12037=CARTESIAN_POINT('Ctrl Pts',(-9.688225,0.298712821306089,3.38425993690586));
#12038=CARTESIAN_POINT('Ctrl Pts',(-9.57054245632586,0.595858078271525,
3.37225675011654));
#12039=CARTESIAN_POINT('Ctrl Pts',(-9.36601586214935,0.813569405232716,
3.36025356332722));
#12040=CARTESIAN_POINT('Ctrl Pts',(-9.16148926797284,1.03128073219391,3.3482503765379));
#12041=CARTESIAN_POINT('Ctrl Pts',(-8.87226522412847,1.16727314847135,3.33624718974859));
#12042=CARTESIAN_POINT('Ctrl Pts',(-8.57413435701451,1.1859100926019,3.32424400295927));
#12043=CARTESIAN_POINT('Ctrl Pts',(-8.27600348990055,1.20454703673244,3.31224081616995));
#12044=CARTESIAN_POINT('Ctrl Pts',(-7.97209482032096,1.1056329054011,3.30023762938063));
#12045=CARTESIAN_POINT('Ctrl Pts',(-7.74204705372063,0.915087963996593,
3.28823444259131));
#12046=CARTESIAN_POINT('Ctrl Pts',(-7.51199928712031,0.724543022592082,
3.276231255802));
#12047=CARTESIAN_POINT('Ctrl Pts',(-7.35822688079636,0.444367128061501,
3.26422806901268));
#12048=CARTESIAN_POINT('Ctrl Pts',(-7.32102560975818,0.14797985599033,3.25222488222336));
#12049=CARTESIAN_POINT('Ctrl Pts',(-7.28382433872,-0.14840741608084,3.24022169543404));
#12050=CARTESIAN_POINT('Ctrl Pts',(-7.36358464744635,-0.457895344721922,
3.22821850864473));
#12051=CARTESIAN_POINT('Ctrl Pts',(-7.5394054943788,-0.699383189957665,
3.21621532185541));
#12052=CARTESIAN_POINT('Ctrl Pts',(-7.71522634131125,-0.940871035193408,
3.20421213506609));
#12053=CARTESIAN_POINT('Ctrl Pts',(-7.9852624056578,-1.1118242708308,3.19220894827677));
#12054=CARTESIAN_POINT('Ctrl Pts',(-8.27875123560113,-1.16744491727746,
3.18020576148745));
#12055=CARTESIAN_POINT('Ctrl Pts',(-8.57224006554445,-1.22306556372411,
3.16820257469814));
#12056=CARTESIAN_POINT('Ctrl Pts',(-8.88610136059936,-1.16276985667026,
3.15619938790882));
#12057=CARTESIAN_POINT('Ctrl Pts',(-9.1380883482009,-1.00235817476352,3.1441962011195));
#12058=CARTESIAN_POINT('Ctrl Pts',(-9.39007533580244,-0.841946492856777,
3.13219301433018));
#12059=CARTESIAN_POINT('Ctrl Pts',(-9.57754329642134,-0.583102430602958,
3.12018982754086));
#12060=CARTESIAN_POINT('Ctrl Pts',(-9.6513665972919,-0.293655596346265,
3.10818664075155));
#12061=CARTESIAN_POINT('Ctrl Pts',(-9.67581103310542,-0.197813707972543,
3.10421213506609));
#12062=CARTESIAN_POINT('Ctrl Pts',(-9.688225,-0.0989100500924119,3.10023762938063));
#12063=CARTESIAN_POINT('Ctrl Pts',(-9.688225,-4.55191440096314E-15,3.09626312369518));
#12064=CARTESIAN_POINT('Ctrl Pts',(-9.688225,-1.74293912635903E-12,3.05373687630491));
#12065=CARTESIAN_POINT('Ctrl Pts',(-9.68822499999956,-0.298712821307838,
3.06574006309423));
#12066=CARTESIAN_POINT('Ctrl Pts',(-9.57054245632499,-0.595858078273102,
3.07774324988354));
#12067=CARTESIAN_POINT('Ctrl Pts',(-9.36601586214815,-0.813569405233993,
3.08974643667286));
#12068=CARTESIAN_POINT('Ctrl Pts',(-9.16148926797132,-1.03128073219488,
3.10174962346218));
#12069=CARTESIAN_POINT('Ctrl Pts',(-8.87226522412674,-1.1672731484719,3.1137528102515));
#12070=CARTESIAN_POINT('Ctrl Pts',(-8.57413435701276,-1.18591009260201,
3.12575599704082));
#12071=CARTESIAN_POINT('Ctrl Pts',(-8.27600348989877,-1.20454703673211,
3.13775918383013));
#12072=CARTESIAN_POINT('Ctrl Pts',(-7.97209482031932,-1.10563290540032,
3.14976237061945));
#12073=CARTESIAN_POINT('Ctrl Pts',(-7.74204705371928,-0.91508796399547,
3.16176555740877));
#12074=CARTESIAN_POINT('Ctrl Pts',(-7.51199928711924,-0.724543022590617,
3.17376874419809));
#12075=CARTESIAN_POINT('Ctrl Pts',(-7.3582268807957,-0.444367128059807,
3.1857719309874));
#12076=CARTESIAN_POINT('Ctrl Pts',(-7.32102560975796,-0.14797985598858,
3.19777511777672));
#12077=CARTESIAN_POINT('Ctrl Pts',(-7.28382433872022,0.148407416082647,
3.20977830456604));
#12078=CARTESIAN_POINT('Ctrl Pts',(-7.36358464744703,0.457895344723612,
3.22178149135536));
#12079=CARTESIAN_POINT('Ctrl Pts',(-7.53940549437984,0.699383189959094,
3.23378467814468));
#12080=CARTESIAN_POINT('Ctrl Pts',(-7.71522634131265,0.940871035194577,
3.24578786493399));
#12081=CARTESIAN_POINT('Ctrl Pts',(-7.98526240565946,1.11182427083157,3.25779105172331));
#12082=CARTESIAN_POINT('Ctrl Pts',(-8.27875123560287,1.16744491727779,3.26979423851263));
#12083=CARTESIAN_POINT('Ctrl Pts',(-8.57224006554628,1.223065563724,3.28179742530195));
#12084=CARTESIAN_POINT('Ctrl Pts',(-8.8861013606011,1.16276985666968,3.29380061209127));
#12085=CARTESIAN_POINT('Ctrl Pts',(-9.1380883482024,1.00235817476256,3.30580379888058));
#12086=CARTESIAN_POINT('Ctrl Pts',(-9.3900753358037,0.841946492855445,3.3178069856699));
#12087=CARTESIAN_POINT('Ctrl Pts',(-9.57754329642222,0.583102430601342,
3.32981017245922));
#12088=CARTESIAN_POINT('Ctrl Pts',(-9.65136659729234,0.293655596344535,
3.34181335924854));
#12089=CARTESIAN_POINT('Ctrl Pts',(-9.67581103310571,0.19781370797079,3.34578786493399));
#12090=CARTESIAN_POINT('Ctrl Pts',(-9.68822500000014,0.0989100500906548,
3.34976237061945));
#12091=CARTESIAN_POINT('Ctrl Pts',(-9.688225,-1.7384427231093E-12,3.35373687630491));
#12092=CARTESIAN_POINT('Origin',(-8.5,0.,1.8));
#12093=CARTESIAN_POINT('',(-9.68847469849902,-0.000576838186012704,3.69626312369518));
#12094=CARTESIAN_POINT('',(-9.688225,-1.74654735118907E-12,3.65373687630491));
#12095=CARTESIAN_POINT('',(-9.688225,-1.45515594291686E-16,1.8));
#12096=CARTESIAN_POINT('Ctrl Pts',(-9.68866306042472,-0.00101198037532446,
3.69626312369518));
#12097=CARTESIAN_POINT('Ctrl Pts',(-9.68582589943624,0.320508041344992,
3.68332310010213));
#12098=CARTESIAN_POINT('Ctrl Pts',(-9.55110894064229,0.644172586075907,
3.67038307650908));
#12099=CARTESIAN_POINT('Ctrl Pts',(-9.31819110540849,0.864496431520476,
3.65744305291603));
#12100=CARTESIAN_POINT('Ctrl Pts',(-9.03186214791326,1.13534343176913,3.64153571176441));
#12101=CARTESIAN_POINT('Ctrl Pts',(-8.59713096356923,1.2500208492789,3.62562837061279));
#12102=CARTESIAN_POINT('Ctrl Pts',(-8.21479992629871,1.1556382784724,3.60972102946117));
#12103=CARTESIAN_POINT('Ctrl Pts',(-7.8324688890282,1.06125570766591,3.59381368830955));
#12104=CARTESIAN_POINT('Ctrl Pts',(-7.50253799883119,0.757813148543147,
3.57790634715793));
#12105=CARTESIAN_POINT('Ctrl Pts',(-7.37423722665768,0.384904745016853,
3.56199900600631));
#12106=CARTESIAN_POINT('Ctrl Pts',(-7.31008684057093,0.198450543253708,
3.5540453354305));
#12107=CARTESIAN_POINT('Ctrl Pts',(-7.29634398399005,-0.0053701196103213,
3.54609166485469));
#12108=CARTESIAN_POINT('Ctrl Pts',(-7.32996872509888,-0.201051408397636,
3.53813799427888));
#12109=CARTESIAN_POINT('Ctrl Pts',(-7.36359346620772,-0.396732697184954,
3.53018432370307));
#12110=CARTESIAN_POINT('Ctrl Pts',(-7.44458580500627,-0.584274611895558,
3.52223065312726));
#12111=CARTESIAN_POINT('Ctrl Pts',(-7.56729714878503,-0.738619574554616,
3.51427698255145));
#12112=CARTESIAN_POINT('Ctrl Pts',(-7.81271983634256,-1.04730949987273,
3.49836964139982));
#12113=CARTESIAN_POINT('Ctrl Pts',(-8.22501854382095,-1.22321161698467,
3.48246230024821));
#12114=CARTESIAN_POINT('Ctrl Pts',(-8.61692498285394,-1.18455369700755,
3.46655495909659));
#12115=CARTESIAN_POINT('Ctrl Pts',(-9.00883142188693,-1.14589577703044,
3.45064761794497));
#12116=CARTESIAN_POINT('Ctrl Pts',(-9.38034559247452,-0.892677819964278,
3.43474027679334));
#12117=CARTESIAN_POINT('Ctrl Pts',(-9.55983865925423,-0.541786656749807,
3.41883293564172));
#12118=CARTESIAN_POINT('Ctrl Pts',(-9.64472870518362,-0.375835026996589,
3.41130966499287));
#12119=CARTESIAN_POINT('Ctrl Pts',(-9.6866683579978,-0.188036305867981,
3.40378639434402));
#12120=CARTESIAN_POINT('Ctrl Pts',(-9.68633860011409,-0.000141139682333869,
3.39626312369518));
#12121=CARTESIAN_POINT('Ctrl Pts',(-9.688225,-1.7384427231093E-12,3.35373687630491));
#12122=CARTESIAN_POINT('Ctrl Pts',(-9.68822499999956,-0.298712821307826,
3.36574006309423));
#12123=CARTESIAN_POINT('Ctrl Pts',(-9.57054245632499,-0.595858078273084,
3.37774324988354));
#12124=CARTESIAN_POINT('Ctrl Pts',(-9.36601586214817,-0.813569405233974,
3.38974643667286));
#12125=CARTESIAN_POINT('Ctrl Pts',(-9.16148926797135,-1.03128073219486,
3.40174962346218));
#12126=CARTESIAN_POINT('Ctrl Pts',(-8.87226522412678,-1.16727314847189,
3.4137528102515));
#12127=CARTESIAN_POINT('Ctrl Pts',(-8.5741343570128,-1.18591009260201,3.42575599704081));
#12128=CARTESIAN_POINT('Ctrl Pts',(-8.27600348989882,-1.20454703673212,
3.43775918383013));
#12129=CARTESIAN_POINT('Ctrl Pts',(-7.97209482031938,-1.10563290540035,
3.44976237061945));
#12130=CARTESIAN_POINT('Ctrl Pts',(-7.74204705371933,-0.915087963995513,
3.46176555740877));
#12131=CARTESIAN_POINT('Ctrl Pts',(-7.51199928711928,-0.724543022590678,
3.47376874419808));
#12132=CARTESIAN_POINT('Ctrl Pts',(-7.35822688079573,-0.444367128059886,
3.4857719309874));
#12133=CARTESIAN_POINT('Ctrl Pts',(-7.32102560975797,-0.147979855988668,
3.49777511777672));
#12134=CARTESIAN_POINT('Ctrl Pts',(-7.28382433872021,0.148407416082549,
3.50977830456604));
#12135=CARTESIAN_POINT('Ctrl Pts',(-7.36358464744699,0.457895344723512,
3.52178149135535));
#12136=CARTESIAN_POINT('Ctrl Pts',(-7.53940549437977,0.699383189959006,
3.53378467814467));
#12137=CARTESIAN_POINT('Ctrl Pts',(-7.71522634131256,0.940871035194499,
3.54578786493399));
#12138=CARTESIAN_POINT('Ctrl Pts',(-7.98526240565934,1.11182427083152,3.55779105172331));
#12139=CARTESIAN_POINT('Ctrl Pts',(-8.27875123560274,1.16744491727776,3.56979423851263));
#12140=CARTESIAN_POINT('Ctrl Pts',(-8.57224006554613,1.22306556372401,3.58179742530194));
#12141=CARTESIAN_POINT('Ctrl Pts',(-8.88610136060096,1.16276985666972,3.59380061209126));
#12142=CARTESIAN_POINT('Ctrl Pts',(-9.13808834820227,1.00235817476264,3.60580379888058));
#12143=CARTESIAN_POINT('Ctrl Pts',(-9.39007533580358,0.841946492855563,
3.6178069856699));
#12144=CARTESIAN_POINT('Ctrl Pts',(-9.57754329642213,0.583102430601495,
3.62981017245921));
#12145=CARTESIAN_POINT('Ctrl Pts',(-9.65136659729229,0.293655596344707,
3.64181335924853));
#12146=CARTESIAN_POINT('Ctrl Pts',(-9.6758110331057,0.197813707970906,3.64578786493399));
#12147=CARTESIAN_POINT('Ctrl Pts',(-9.68822500000014,0.0989100500907086,
3.64976237061945));
#12148=CARTESIAN_POINT('Ctrl Pts',(-9.688225,-1.74654735118907E-12,3.65373687630491));
#12149=CARTESIAN_POINT('Origin',(-8.5,0.,1.8));
#12150=CARTESIAN_POINT('',(-9.688225,-2.04281036531029E-14,3.99626312369518));
#12151=CARTESIAN_POINT('',(-9.688225,-1.75470749042006E-12,3.95373687630491));
#12152=CARTESIAN_POINT('',(-9.688225,-1.45515594291686E-16,1.8));
#12153=CARTESIAN_POINT('Ctrl Pts',(-9.688225,-3.66373598126302E-15,3.99626312369518));
#12154=CARTESIAN_POINT('Ctrl Pts',(-9.688225,0.29871282130609,3.98425993690586));
#12155=CARTESIAN_POINT('Ctrl Pts',(-9.57054245632586,0.595858078271525,
3.97225675011654));
#12156=CARTESIAN_POINT('Ctrl Pts',(-9.36601586214935,0.813569405232717,
3.96025356332722));
#12157=CARTESIAN_POINT('Ctrl Pts',(-9.16148926797284,1.03128073219391,3.94825037653791));
#12158=CARTESIAN_POINT('Ctrl Pts',(-8.87226522412847,1.16727314847135,3.93624718974859));
#12159=CARTESIAN_POINT('Ctrl Pts',(-8.57413435701451,1.1859100926019,3.92424400295927));
#12160=CARTESIAN_POINT('Ctrl Pts',(-8.27600348990055,1.20454703673244,3.91224081616995));
#12161=CARTESIAN_POINT('Ctrl Pts',(-7.97209482032096,1.1056329054011,3.90023762938063));
#12162=CARTESIAN_POINT('Ctrl Pts',(-7.74204705372063,0.915087963996592,
3.88823444259132));
#12163=CARTESIAN_POINT('Ctrl Pts',(-7.51199928712031,0.724543022592081,
3.876231255802));
#12164=CARTESIAN_POINT('Ctrl Pts',(-7.35822688079636,0.4443671280615,3.86422806901268));
#12165=CARTESIAN_POINT('Ctrl Pts',(-7.32102560975818,0.14797985599033,3.85222488222336));
#12166=CARTESIAN_POINT('Ctrl Pts',(-7.28382433872,-0.148407416080841,3.84022169543404));
#12167=CARTESIAN_POINT('Ctrl Pts',(-7.36358464744635,-0.457895344721922,
3.82821850864473));
#12168=CARTESIAN_POINT('Ctrl Pts',(-7.5394054943788,-0.699383189957666,
3.81621532185541));
#12169=CARTESIAN_POINT('Ctrl Pts',(-7.71522634131125,-0.940871035193409,
3.80421213506609));
#12170=CARTESIAN_POINT('Ctrl Pts',(-7.9852624056578,-1.11182427083081,3.79220894827677));
#12171=CARTESIAN_POINT('Ctrl Pts',(-8.27875123560113,-1.16744491727746,
3.78020576148745));
#12172=CARTESIAN_POINT('Ctrl Pts',(-8.57224006554445,-1.22306556372411,
3.76820257469814));
#12173=CARTESIAN_POINT('Ctrl Pts',(-8.88610136059936,-1.16276985667026,
3.75619938790882));
#12174=CARTESIAN_POINT('Ctrl Pts',(-9.1380883482009,-1.00235817476352,3.7441962011195));
#12175=CARTESIAN_POINT('Ctrl Pts',(-9.39007533580244,-0.841946492856777,
3.73219301433018));
#12176=CARTESIAN_POINT('Ctrl Pts',(-9.57754329642134,-0.583102430602957,
3.72018982754087));
#12177=CARTESIAN_POINT('Ctrl Pts',(-9.6513665972919,-0.293655596346264,
3.70818664075155));
#12178=CARTESIAN_POINT('Ctrl Pts',(-9.67581103310542,-0.197813707972545,
3.70421213506609));
#12179=CARTESIAN_POINT('Ctrl Pts',(-9.688225,-0.0989100500924169,3.70023762938063));
#12180=CARTESIAN_POINT('Ctrl Pts',(-9.688225,-1.24344978758018E-14,3.69626312369518));
#12181=CARTESIAN_POINT('Ctrl Pts',(-9.688225,-1.74654735118907E-12,3.65373687630491));
#12182=CARTESIAN_POINT('Ctrl Pts',(-9.68822499999956,-0.298712821307834,
3.66574006309423));
#12183=CARTESIAN_POINT('Ctrl Pts',(-9.57054245632499,-0.595858078273091,
3.67774324988354));
#12184=CARTESIAN_POINT('Ctrl Pts',(-9.36601586214816,-0.81356940523398,
3.68974643667286));
#12185=CARTESIAN_POINT('Ctrl Pts',(-9.16148926797134,-1.03128073219487,
3.70174962346218));
#12186=CARTESIAN_POINT('Ctrl Pts',(-8.87226522412678,-1.16727314847189,
3.7137528102515));
#12187=CARTESIAN_POINT('Ctrl Pts',(-8.5741343570128,-1.18591009260201,3.72575599704081));
#12188=CARTESIAN_POINT('Ctrl Pts',(-8.27600348989881,-1.20454703673212,
3.73775918383013));
#12189=CARTESIAN_POINT('Ctrl Pts',(-7.97209482031937,-1.10563290540034,
3.74976237061945));
#12190=CARTESIAN_POINT('Ctrl Pts',(-7.74204705371933,-0.915087963995508,
3.76176555740877));
#12191=CARTESIAN_POINT('Ctrl Pts',(-7.51199928711928,-0.724543022590671,
3.77376874419808));
#12192=CARTESIAN_POINT('Ctrl Pts',(-7.35822688079573,-0.444367128059878,
3.7857719309874));
#12193=CARTESIAN_POINT('Ctrl Pts',(-7.32102560975797,-0.14797985598866,
3.79777511777672));
#12194=CARTESIAN_POINT('Ctrl Pts',(-7.28382433872021,0.148407416082557,
3.80977830456604));
#12195=CARTESIAN_POINT('Ctrl Pts',(-7.363584647447,0.45789534472352,3.82178149135535));
#12196=CARTESIAN_POINT('Ctrl Pts',(-7.53940549437978,0.699383189959012,
3.83378467814467));
#12197=CARTESIAN_POINT('Ctrl Pts',(-7.71522634131256,0.940871035194504,
3.84578786493399));
#12198=CARTESIAN_POINT('Ctrl Pts',(-7.98526240565935,1.11182427083152,3.85779105172331));
#12199=CARTESIAN_POINT('Ctrl Pts',(-8.27875123560275,1.16744491727777,3.86979423851263));
#12200=CARTESIAN_POINT('Ctrl Pts',(-8.57224006554614,1.22306556372401,3.88179742530194));
#12201=CARTESIAN_POINT('Ctrl Pts',(-8.88610136060096,1.16276985666972,3.89380061209126));
#12202=CARTESIAN_POINT('Ctrl Pts',(-9.13808834820228,1.00235817476264,3.90580379888058));
#12203=CARTESIAN_POINT('Ctrl Pts',(-9.39007533580359,0.841946492855557,
3.9178069856699));
#12204=CARTESIAN_POINT('Ctrl Pts',(-9.57754329642214,0.583102430601487,
3.92981017245921));
#12205=CARTESIAN_POINT('Ctrl Pts',(-9.6513665972923,0.293655596344699,3.94181335924853));
#12206=CARTESIAN_POINT('Ctrl Pts',(-9.6758110331057,0.1978137079709,3.94578786493399));
#12207=CARTESIAN_POINT('Ctrl Pts',(-9.68822500000014,0.0989100500907061,
3.94976237061945));
#12208=CARTESIAN_POINT('Ctrl Pts',(-9.688225,-1.74621428428168E-12,3.95373687630491));
#12209=CARTESIAN_POINT('Origin',(-8.5,0.,1.8));
#12210=CARTESIAN_POINT('',(-9.688225,-2.87547763377916E-14,4.29626312369518));
#12211=CARTESIAN_POINT('',(-9.688225,-1.76286762965105E-12,4.25373687630491));
#12212=CARTESIAN_POINT('',(-9.688225,-1.45515594291686E-16,1.8));
#12213=CARTESIAN_POINT('Ctrl Pts',(-9.688225,-2.03170813506404E-14,4.29626312369518));
#12214=CARTESIAN_POINT('Ctrl Pts',(-9.68822500000001,0.298712821306068,
4.28425993690586));
#12215=CARTESIAN_POINT('Ctrl Pts',(-9.57054245632588,0.595858078271499,
4.27225675011654));
#12216=CARTESIAN_POINT('Ctrl Pts',(-9.36601586214937,0.813569405232692,
4.26025356332722));
#12217=CARTESIAN_POINT('Ctrl Pts',(-9.16148926797287,1.03128073219389,4.24825037653791));
#12218=CARTESIAN_POINT('Ctrl Pts',(-8.87226522412851,1.16727314847134,4.23624718974859));
#12219=CARTESIAN_POINT('Ctrl Pts',(-8.57413435701456,1.1859100926019,4.22424400295927));
#12220=CARTESIAN_POINT('Ctrl Pts',(-8.2760034899006,1.20454703673245,4.21224081616995));
#12221=CARTESIAN_POINT('Ctrl Pts',(-7.97209482032102,1.10563290540113,4.20023762938064));
#12222=CARTESIAN_POINT('Ctrl Pts',(-7.74204705372069,0.915087963996635,
4.18823444259132));
#12223=CARTESIAN_POINT('Ctrl Pts',(-7.51199928712035,0.724543022592141,
4.176231255802));
#12224=CARTESIAN_POINT('Ctrl Pts',(-7.35822688079639,0.444367128061576,
4.16422806901268));
#12225=CARTESIAN_POINT('Ctrl Pts',(-7.32102560975819,0.147979855990413,
4.15222488222336));
#12226=CARTESIAN_POINT('Ctrl Pts',(-7.28382433871999,-0.148407416080749,
4.14022169543405));
#12227=CARTESIAN_POINT('Ctrl Pts',(-7.36358464744631,-0.45789534472183,
4.12821850864473));
#12228=CARTESIAN_POINT('Ctrl Pts',(-7.53940549437874,-0.699383189957584,
4.11621532185541));
#12229=CARTESIAN_POINT('Ctrl Pts',(-7.71522634131116,-0.940871035193337,
4.10421213506609));
#12230=CARTESIAN_POINT('Ctrl Pts',(-7.9852624056577,-1.11182427083076,4.09220894827678));
#12231=CARTESIAN_POINT('Ctrl Pts',(-8.27875123560101,-1.16744491727744,
4.08020576148746));
#12232=CARTESIAN_POINT('Ctrl Pts',(-8.57224006554433,-1.22306556372412,
4.06820257469814));
#12233=CARTESIAN_POINT('Ctrl Pts',(-8.88610136059923,-1.1627698566703,4.05619938790882));
#12234=CARTESIAN_POINT('Ctrl Pts',(-9.13808834820079,-1.00235817476359,
4.04419620111951));
#12235=CARTESIAN_POINT('Ctrl Pts',(-9.39007533580234,-0.841946492856881,
4.03219301433019));
#12236=CARTESIAN_POINT('Ctrl Pts',(-9.57754329642127,-0.58310243060309,
4.02018982754087));
#12237=CARTESIAN_POINT('Ctrl Pts',(-9.65136659729186,-0.293655596346411,
4.00818664075155));
#12238=CARTESIAN_POINT('Ctrl Pts',(-9.67581103310541,-0.197813707972643,
4.00421213506609));
#12239=CARTESIAN_POINT('Ctrl Pts',(-9.688225,-0.0989100500924617,4.00023762938063));
#12240=CARTESIAN_POINT('Ctrl Pts',(-9.688225,-3.66373598126302E-15,3.99626312369518));
#12241=CARTESIAN_POINT('Ctrl Pts',(-9.688225,-1.74621428428168E-12,3.95373687630491));
#12242=CARTESIAN_POINT('Ctrl Pts',(-9.68822499999956,-0.298712821307834,
3.96574006309423));
#12243=CARTESIAN_POINT('Ctrl Pts',(-9.57054245632499,-0.595858078273091,
3.97774324988354));
#12244=CARTESIAN_POINT('Ctrl Pts',(-9.36601586214816,-0.81356940523398,
3.98974643667286));
#12245=CARTESIAN_POINT('Ctrl Pts',(-9.16148926797134,-1.03128073219487,
4.00174962346218));
#12246=CARTESIAN_POINT('Ctrl Pts',(-8.87226522412678,-1.16727314847189,
4.0137528102515));
#12247=CARTESIAN_POINT('Ctrl Pts',(-8.5741343570128,-1.18591009260201,4.02575599704081));
#12248=CARTESIAN_POINT('Ctrl Pts',(-8.27600348989881,-1.20454703673212,
4.03775918383013));
#12249=CARTESIAN_POINT('Ctrl Pts',(-7.97209482031937,-1.10563290540034,
4.04976237061945));
#12250=CARTESIAN_POINT('Ctrl Pts',(-7.74204705371933,-0.915087963995508,
4.06176555740877));
#12251=CARTESIAN_POINT('Ctrl Pts',(-7.51199928711928,-0.724543022590671,
4.07376874419808));
#12252=CARTESIAN_POINT('Ctrl Pts',(-7.35822688079573,-0.444367128059878,
4.0857719309874));
#12253=CARTESIAN_POINT('Ctrl Pts',(-7.32102560975797,-0.14797985598866,
4.09777511777672));
#12254=CARTESIAN_POINT('Ctrl Pts',(-7.28382433872021,0.148407416082557,
4.10977830456604));
#12255=CARTESIAN_POINT('Ctrl Pts',(-7.363584647447,0.45789534472352,4.12178149135535));
#12256=CARTESIAN_POINT('Ctrl Pts',(-7.53940549437978,0.699383189959012,
4.13378467814467));
#12257=CARTESIAN_POINT('Ctrl Pts',(-7.71522634131256,0.940871035194504,
4.14578786493399));
#12258=CARTESIAN_POINT('Ctrl Pts',(-7.98526240565935,1.11182427083152,4.15779105172331));
#12259=CARTESIAN_POINT('Ctrl Pts',(-8.27875123560275,1.16744491727777,4.16979423851263));
#12260=CARTESIAN_POINT('Ctrl Pts',(-8.57224006554614,1.22306556372401,4.18179742530194));
#12261=CARTESIAN_POINT('Ctrl Pts',(-8.88610136060096,1.16276985666972,4.19380061209126));
#12262=CARTESIAN_POINT('Ctrl Pts',(-9.13808834820228,1.00235817476264,4.20580379888058));
#12263=CARTESIAN_POINT('Ctrl Pts',(-9.39007533580359,0.841946492855557,
4.2178069856699));
#12264=CARTESIAN_POINT('Ctrl Pts',(-9.57754329642213,0.583102430601487,
4.22981017245921));
#12265=CARTESIAN_POINT('Ctrl Pts',(-9.6513665972923,0.293655596344699,4.24181335924853));
#12266=CARTESIAN_POINT('Ctrl Pts',(-9.6758110331057,0.197813707970898,4.24578786493399));
#12267=CARTESIAN_POINT('Ctrl Pts',(-9.68822500000014,0.0989100500907007,
4.24976237061945));
#12268=CARTESIAN_POINT('Ctrl Pts',(-9.688225,-1.7544299346639E-12,4.25373687630491));
#12269=CARTESIAN_POINT('Origin',(-8.5,0.,1.8));
#12270=CARTESIAN_POINT('',(-9.688225,-3.68594044175552E-14,4.59626312369518));
#12271=CARTESIAN_POINT('',(-9.688225,-1.77097225773082E-12,4.55373687630491));
#12272=CARTESIAN_POINT('',(-9.688225,-1.45515594291686E-16,1.8));
#12273=CARTESIAN_POINT('Ctrl Pts',(-9.688225,-1.15463194561016E-14,4.59626312369518));
#12274=CARTESIAN_POINT('Ctrl Pts',(-9.688225,0.298712821306079,4.58425993690586));
#12275=CARTESIAN_POINT('Ctrl Pts',(-9.57054245632587,0.595858078271513,
4.57225675011654));
#12276=CARTESIAN_POINT('Ctrl Pts',(-9.36601586214936,0.813569405232705,
4.56025356332722));
#12277=CARTESIAN_POINT('Ctrl Pts',(-9.16148926797286,1.0312807321939,4.54825037653791));
#12278=CARTESIAN_POINT('Ctrl Pts',(-8.87226522412849,1.16727314847135,4.53624718974859));
#12279=CARTESIAN_POINT('Ctrl Pts',(-8.57413435701453,1.1859100926019,4.52424400295927));
#12280=CARTESIAN_POINT('Ctrl Pts',(-8.27600348990058,1.20454703673245,4.51224081616995));
#12281=CARTESIAN_POINT('Ctrl Pts',(-7.97209482032099,1.10563290540112,4.50023762938063));
#12282=CARTESIAN_POINT('Ctrl Pts',(-7.74204705372066,0.915087963996614,
4.48823444259132));
#12283=CARTESIAN_POINT('Ctrl Pts',(-7.51199928712033,0.724543022592111,
4.476231255802));
#12284=CARTESIAN_POINT('Ctrl Pts',(-7.35822688079637,0.444367128061538,
4.46422806901268));
#12285=CARTESIAN_POINT('Ctrl Pts',(-7.32102560975818,0.147979855990371,
4.45222488222336));
#12286=CARTESIAN_POINT('Ctrl Pts',(-7.28382433871999,-0.148407416080795,
4.44022169543405));
#12287=CARTESIAN_POINT('Ctrl Pts',(-7.36358464744633,-0.457895344721877,
4.42821850864473));
#12288=CARTESIAN_POINT('Ctrl Pts',(-7.53940549437877,-0.699383189957625,
4.41621532185541));
#12289=CARTESIAN_POINT('Ctrl Pts',(-7.71522634131121,-0.940871035193374,
4.40421213506609));
#12290=CARTESIAN_POINT('Ctrl Pts',(-7.98526240565775,-1.11182427083078,
4.39220894827677));
#12291=CARTESIAN_POINT('Ctrl Pts',(-8.27875123560107,-1.16744491727745,
4.38020576148746));
#12292=CARTESIAN_POINT('Ctrl Pts',(-8.57224006554439,-1.22306556372412,
4.36820257469814));
#12293=CARTESIAN_POINT('Ctrl Pts',(-8.8861013605993,-1.16276985667028,4.35619938790882));
#12294=CARTESIAN_POINT('Ctrl Pts',(-9.13808834820084,-1.00235817476355,
4.3441962011195));
#12295=CARTESIAN_POINT('Ctrl Pts',(-9.39007533580239,-0.841946492856829,
4.33219301433019));
#12296=CARTESIAN_POINT('Ctrl Pts',(-9.5775432964213,-0.583102430603023,
4.32018982754087));
#12297=CARTESIAN_POINT('Ctrl Pts',(-9.65136659729188,-0.293655596346337,
4.30818664075155));
#12298=CARTESIAN_POINT('Ctrl Pts',(-9.67581103310541,-0.197813707972598,
4.30421213506609));
#12299=CARTESIAN_POINT('Ctrl Pts',(-9.688225,-0.0989100500924473,4.30023762938063));
#12300=CARTESIAN_POINT('Ctrl Pts',(-9.688225,-2.03170813506404E-14,4.29626312369518));
#12301=CARTESIAN_POINT('Ctrl Pts',(-9.688225,-1.7544299346639E-12,4.25373687630491));
#12302=CARTESIAN_POINT('Ctrl Pts',(-9.68822499999956,-0.298712821307842,
4.26574006309423));
#12303=CARTESIAN_POINT('Ctrl Pts',(-9.57054245632498,-0.595858078273098,
4.27774324988354));
#12304=CARTESIAN_POINT('Ctrl Pts',(-9.36601586214816,-0.813569405233986,
4.28974643667286));
#12305=CARTESIAN_POINT('Ctrl Pts',(-9.16148926797133,-1.03128073219487,
4.30174962346218));
#12306=CARTESIAN_POINT('Ctrl Pts',(-8.87226522412677,-1.1672731484719,4.3137528102515));
#12307=CARTESIAN_POINT('Ctrl Pts',(-8.57413435701279,-1.18591009260201,
4.32575599704081));
#12308=CARTESIAN_POINT('Ctrl Pts',(-8.27600348989881,-1.20454703673212,
4.33775918383013));
#12309=CARTESIAN_POINT('Ctrl Pts',(-7.97209482031937,-1.10563290540034,
4.34976237061945));
#12310=CARTESIAN_POINT('Ctrl Pts',(-7.74204705371932,-0.915087963995503,
4.36176555740877));
#12311=CARTESIAN_POINT('Ctrl Pts',(-7.51199928711927,-0.724543022590665,
4.37376874419808));
#12312=CARTESIAN_POINT('Ctrl Pts',(-7.35822688079572,-0.44436712805987,
4.3857719309874));
#12313=CARTESIAN_POINT('Ctrl Pts',(-7.32102560975797,-0.147979855988652,
4.39777511777672));
#12314=CARTESIAN_POINT('Ctrl Pts',(-7.28382433872021,0.148407416082565,
4.40977830456604));
#12315=CARTESIAN_POINT('Ctrl Pts',(-7.363584647447,0.457895344723527,4.42178149135536));
#12316=CARTESIAN_POINT('Ctrl Pts',(-7.53940549437978,0.699383189959018,
4.43378467814467));
#12317=CARTESIAN_POINT('Ctrl Pts',(-7.71522634131257,0.94087103519451,4.44578786493399));
#12318=CARTESIAN_POINT('Ctrl Pts',(-7.98526240565936,1.11182427083152,4.45779105172331));
#12319=CARTESIAN_POINT('Ctrl Pts',(-8.27875123560275,1.16744491727777,4.46979423851263));
#12320=CARTESIAN_POINT('Ctrl Pts',(-8.57224006554615,1.22306556372401,4.48179742530194));
#12321=CARTESIAN_POINT('Ctrl Pts',(-8.88610136060097,1.16276985666972,4.49380061209126));
#12322=CARTESIAN_POINT('Ctrl Pts',(-9.13808834820228,1.00235817476264,4.50580379888058));
#12323=CARTESIAN_POINT('Ctrl Pts',(-9.39007533580359,0.841946492855551,
4.5178069856699));
#12324=CARTESIAN_POINT('Ctrl Pts',(-9.57754329642214,0.58310243060148,4.52981017245921));
#12325=CARTESIAN_POINT('Ctrl Pts',(-9.6513665972923,0.293655596344692,4.54181335924853));
#12326=CARTESIAN_POINT('Ctrl Pts',(-9.6758110331057,0.197813707970884,4.54578786493399));
#12327=CARTESIAN_POINT('Ctrl Pts',(-9.68822500000015,0.0989100500906813,
4.54976237061945));
#12328=CARTESIAN_POINT('Ctrl Pts',(-9.688225,-1.7794654638692E-12,4.55373687630491));
#12329=CARTESIAN_POINT('Origin',(-8.5,0.,1.8));
#12330=CARTESIAN_POINT('',(-9.688225,-4.50750547997814E-14,4.89626312369518));
#12331=CARTESIAN_POINT('',(-9.68890234474114,2.93777303478513E-5,4.85373687630491));
#12332=CARTESIAN_POINT('',(-9.688225,-1.45515594291686E-16,1.8));
#12333=CARTESIAN_POINT('Ctrl Pts',(-9.688225,-2.80886425230165E-14,4.89626312369518));
#12334=CARTESIAN_POINT('Ctrl Pts',(-9.68822500000001,0.29871282130606,4.88425993690586));
#12335=CARTESIAN_POINT('Ctrl Pts',(-9.57054245632588,0.595858078271492,
4.87225675011654));
#12336=CARTESIAN_POINT('Ctrl Pts',(-9.36601586214938,0.813569405232687,
4.86025356332722));
#12337=CARTESIAN_POINT('Ctrl Pts',(-9.16148926797288,1.03128073219388,4.84825037653791));
#12338=CARTESIAN_POINT('Ctrl Pts',(-8.87226522412852,1.16727314847134,4.83624718974859));
#12339=CARTESIAN_POINT('Ctrl Pts',(-8.57413435701457,1.1859100926019,4.82424400295927));
#12340=CARTESIAN_POINT('Ctrl Pts',(-8.27600348990061,1.20454703673246,4.81224081616995));
#12341=CARTESIAN_POINT('Ctrl Pts',(-7.97209482032102,1.10563290540113,4.80023762938064));
#12342=CARTESIAN_POINT('Ctrl Pts',(-7.74204705372069,0.91508796399664,4.78823444259132));
#12343=CARTESIAN_POINT('Ctrl Pts',(-7.51199928712036,0.724543022592147,
4.776231255802));
#12344=CARTESIAN_POINT('Ctrl Pts',(-7.35822688079639,0.444367128061583,
4.76422806901268));
#12345=CARTESIAN_POINT('Ctrl Pts',(-7.32102560975819,0.147979855990421,
4.75222488222337));
#12346=CARTESIAN_POINT('Ctrl Pts',(-7.28382433871998,-0.148407416080741,
4.74022169543405));
#12347=CARTESIAN_POINT('Ctrl Pts',(-7.36358464744631,-0.457895344721823,
4.72821850864473));
#12348=CARTESIAN_POINT('Ctrl Pts',(-7.53940549437873,-0.699383189957578,
4.71621532185541));
#12349=CARTESIAN_POINT('Ctrl Pts',(-7.71522634131116,-0.940871035193332,
4.7042121350661));
#12350=CARTESIAN_POINT('Ctrl Pts',(-7.98526240565769,-1.11182427083075,
4.69220894827678));
#12351=CARTESIAN_POINT('Ctrl Pts',(-8.278751235601,-1.16744491727744,4.68020576148746));
#12352=CARTESIAN_POINT('Ctrl Pts',(-8.57224006554432,-1.22306556372412,
4.66820257469814));
#12353=CARTESIAN_POINT('Ctrl Pts',(-8.88610136059923,-1.1627698566703,4.65619938790882));
#12354=CARTESIAN_POINT('Ctrl Pts',(-9.13808834820078,-1.00235817476359,
4.64419620111951));
#12355=CARTESIAN_POINT('Ctrl Pts',(-9.39007533580233,-0.841946492856887,
4.63219301433019));
#12356=CARTESIAN_POINT('Ctrl Pts',(-9.57754329642126,-0.583102430603097,
4.62018982754087));
#12357=CARTESIAN_POINT('Ctrl Pts',(-9.65136659729186,-0.293655596346419,
4.60818664075155));
#12358=CARTESIAN_POINT('Ctrl Pts',(-9.67581103310541,-0.197813707972651,
4.60421213506609));
#12359=CARTESIAN_POINT('Ctrl Pts',(-9.688225,-0.0989100500924695,4.60023762938064));
#12360=CARTESIAN_POINT('Ctrl Pts',(-9.688225,-1.15463194561016E-14,4.59626312369518));
#12361=CARTESIAN_POINT('Ctrl Pts',(-9.688225,-1.7794654638692E-12,4.55373687630491));
#12362=CARTESIAN_POINT('Ctrl Pts',(-9.68822499999955,-0.298712821307867,
4.56574006309423));
#12363=CARTESIAN_POINT('Ctrl Pts',(-9.57054245632497,-0.595858078273121,
4.57774324988354));
#12364=CARTESIAN_POINT('Ctrl Pts',(-9.36601586214814,-0.813569405234004,
4.58974643667286));
#12365=CARTESIAN_POINT('Ctrl Pts',(-9.16148926797131,-1.03128073219489,
4.60174962346218));
#12366=CARTESIAN_POINT('Ctrl Pts',(-8.87226522412674,-1.1672731484719,4.6137528102515));
#12367=CARTESIAN_POINT('Ctrl Pts',(-8.57413435701276,-1.18591009260201,
4.62575599704082));
#12368=CARTESIAN_POINT('Ctrl Pts',(-8.27600348989878,-1.20454703673211,
4.63775918383013));
#12369=CARTESIAN_POINT('Ctrl Pts',(-7.97209482031934,-1.10563290540033,
4.64976237061945));
#12370=CARTESIAN_POINT('Ctrl Pts',(-7.7420470537193,-0.915087963995487,
4.66176555740877));
#12371=CARTESIAN_POINT('Ctrl Pts',(-7.51199928711926,-0.724543022590644,
4.67376874419809));
#12372=CARTESIAN_POINT('Ctrl Pts',(-7.35822688079571,-0.444367128059846,
4.6857719309874));
#12373=CARTESIAN_POINT('Ctrl Pts',(-7.32102560975796,-0.147979855988628,
4.69777511777672));
#12374=CARTESIAN_POINT('Ctrl Pts',(-7.28382433872021,0.148407416082591,
4.70977830456604));
#12375=CARTESIAN_POINT('Ctrl Pts',(-7.36358464744701,0.457895344723551,
4.72178149135536));
#12376=CARTESIAN_POINT('Ctrl Pts',(-7.5394054943798,0.699383189959039,4.73378467814467));
#12377=CARTESIAN_POINT('Ctrl Pts',(-7.71522634131259,0.940871035194526,
4.74578786493399));
#12378=CARTESIAN_POINT('Ctrl Pts',(-7.98526240565938,1.11182427083153,4.75779105172331));
#12379=CARTESIAN_POINT('Ctrl Pts',(-8.27875123560278,1.16744491727777,4.76979423851263));
#12380=CARTESIAN_POINT('Ctrl Pts',(-8.57224006554618,1.22306556372401,4.78179742530194));
#12381=CARTESIAN_POINT('Ctrl Pts',(-8.886101360601,1.16276985666971,4.79380061209126));
#12382=CARTESIAN_POINT('Ctrl Pts',(-9.1380883482023,1.00235817476262,4.80580379888058));
#12383=CARTESIAN_POINT('Ctrl Pts',(-9.39007533580361,0.841946492855533,
4.8178069856699));
#12384=CARTESIAN_POINT('Ctrl Pts',(-9.57754329642215,0.583102430601457,
4.82981017245922));
#12385=CARTESIAN_POINT('Ctrl Pts',(-9.6513665972923,0.293655596344667,4.84181335924853));
#12386=CARTESIAN_POINT('Ctrl Pts',(-9.67581103310571,0.19781370797087,4.84578786493399));
#12387=CARTESIAN_POINT('Ctrl Pts',(-9.68822500000015,0.0989100500906788,
4.84976237061945));
#12388=CARTESIAN_POINT('Ctrl Pts',(-9.688225,-1.77075021312589E-12,4.85373687630491));
#12389=CARTESIAN_POINT('Origin',(-8.5,0.,1.8));
#12390=CARTESIAN_POINT('',(-9.688225,-5.3179682879545E-14,5.19626312369518));
#12391=CARTESIAN_POINT('',(-9.68763172722904,0.00105126113166729,5.15373687630492));
#12392=CARTESIAN_POINT('',(-9.688225,-1.45515594291686E-16,1.8));
#12393=CARTESIAN_POINT('Ctrl Pts',(-9.688225,-3.61932706027801E-14,5.19626312369518));
#12394=CARTESIAN_POINT('Ctrl Pts',(-9.68822500000001,0.298712821306057,
5.18425993690586));
#12395=CARTESIAN_POINT('Ctrl Pts',(-9.57054245632588,0.595858078271496,
5.17225675011654));
#12396=CARTESIAN_POINT('Ctrl Pts',(-9.36601586214937,0.813569405232693,
5.16025356332722));
#12397=CARTESIAN_POINT('Ctrl Pts',(-9.16148926797287,1.03128073219389,5.14825037653791));
#12398=CARTESIAN_POINT('Ctrl Pts',(-8.8722652241285,1.16727314847134,5.13624718974859));
#12399=CARTESIAN_POINT('Ctrl Pts',(-8.57413435701454,1.1859100926019,5.12424400295927));
#12400=CARTESIAN_POINT('Ctrl Pts',(-8.27600348990058,1.20454703673245,5.11224081616995));
#12401=CARTESIAN_POINT('Ctrl Pts',(-7.97209482032099,1.10563290540112,5.10023762938063));
#12402=CARTESIAN_POINT('Ctrl Pts',(-7.74204705372066,0.915087963996613,
5.08823444259132));
#12403=CARTESIAN_POINT('Ctrl Pts',(-7.51199928712033,0.724543022592108,
5.076231255802));
#12404=CARTESIAN_POINT('Ctrl Pts',(-7.35822688079637,0.444367128061532,
5.06422806901268));
#12405=CARTESIAN_POINT('Ctrl Pts',(-7.32102560975818,0.147979855990362,
5.05222488222336));
#12406=CARTESIAN_POINT('Ctrl Pts',(-7.28382433871999,-0.148407416080807,
5.04022169543405));
#12407=CARTESIAN_POINT('Ctrl Pts',(-7.36358464744634,-0.457895344721891,
5.02821850864473));
#12408=CARTESIAN_POINT('Ctrl Pts',(-7.53940549437878,-0.699383189957639,
5.01621532185541));
#12409=CARTESIAN_POINT('Ctrl Pts',(-7.71522634131122,-0.940871035193387,
5.00421213506609));
#12410=CARTESIAN_POINT('Ctrl Pts',(-7.98526240565777,-1.11182427083079,
4.99220894827677));
#12411=CARTESIAN_POINT('Ctrl Pts',(-8.27875123560109,-1.16744491727745,
4.98020576148746));
#12412=CARTESIAN_POINT('Ctrl Pts',(-8.57224006554442,-1.22306556372411,
4.96820257469814));
#12413=CARTESIAN_POINT('Ctrl Pts',(-8.88610136059933,-1.16276985667027,
4.95619938790882));
#12414=CARTESIAN_POINT('Ctrl Pts',(-9.13808834820087,-1.00235817476353,
4.9441962011195));
#12415=CARTESIAN_POINT('Ctrl Pts',(-9.39007533580241,-0.841946492856801,
4.93219301433018));
#12416=CARTESIAN_POINT('Ctrl Pts',(-9.57754329642133,-0.583102430602987,
4.92018982754087));
#12417=CARTESIAN_POINT('Ctrl Pts',(-9.65136659729189,-0.293655596346296,
4.90818664075155));
#12418=CARTESIAN_POINT('Ctrl Pts',(-9.67581103310542,-0.197813707972572,
4.90421213506609));
#12419=CARTESIAN_POINT('Ctrl Pts',(-9.688225,-0.0989100500924382,4.90023762938063));
#12420=CARTESIAN_POINT('Ctrl Pts',(-9.688225,-2.80886425230165E-14,4.89626312369518));
#12421=CARTESIAN_POINT('Ctrl Pts',(-9.69028763874726,8.94605781823637E-5,
4.8537368763049));
#12422=CARTESIAN_POINT('Ctrl Pts',(-9.69029065164093,-0.00381389069076675,
4.85389441790699));
#12423=CARTESIAN_POINT('Ctrl Pts',(-9.69027262936407,-0.00771725416388489,
4.85405195950908));
#12424=CARTESIAN_POINT('Ctrl Pts',(-9.69023347715143,-0.0116204539158122,
4.85420950111117));
#12425=CARTESIAN_POINT('Ctrl Pts',(-9.68628018738611,-0.405735590575178,
4.87011684226279));
#12426=CARTESIAN_POINT('Ctrl Pts',(-9.46689854929461,-0.798181522642429,
4.88602418341442));
#12427=CARTESIAN_POINT('Ctrl Pts',(-9.13347788059196,-1.00774237159632,
4.90193152456604));
#12428=CARTESIAN_POINT('Ctrl Pts',(-8.80005721188931,-1.21730322055022,
4.91783886571766));
#12429=CARTESIAN_POINT('Ctrl Pts',(-8.35259751257551,-1.24397898639076,
4.93374620686927));
#12430=CARTESIAN_POINT('Ctrl Pts',(-7.99517517866866,-1.07733253192674,
4.9496535480209));
#12431=CARTESIAN_POINT('Ctrl Pts',(-7.81646401171523,-0.994009304694722,
4.95760721859671));
#12432=CARTESIAN_POINT('Ctrl Pts',(-7.66026218611355,-0.86235552238656,
4.96556088917252));
#12433=CARTESIAN_POINT('Ctrl Pts',(-7.54281123274328,-0.702270971137819,
4.97351455974833));
#12434=CARTESIAN_POINT('Ctrl Pts',(-7.42536027937301,-0.542186419889074,
4.98146823032414));
#12435=CARTESIAN_POINT('Ctrl Pts',(-7.34666019823415,-0.353671099699739,
4.98942190089995));
#12436=CARTESIAN_POINT('Ctrl Pts',(-7.32081840553957,-0.158190555551361,
4.99737557147576));
#12437=CARTESIAN_POINT('Ctrl Pts',(-7.26913482015041,0.232770532745374,
5.01328291262738));
#12438=CARTESIAN_POINT('Ctrl Pts',(-7.42888438853832,0.651592516878301,
5.029190253779));
#12439=CARTESIAN_POINT('Ctrl Pts',(-7.72885825501123,0.906741044535612,
5.04509759493063));
#12440=CARTESIAN_POINT('Ctrl Pts',(-8.02883212148414,1.16188957219293,5.06100493608225));
#12441=CARTESIAN_POINT('Ctrl Pts',(-8.46903028604204,1.25336464337461,5.07691227723386));
#12442=CARTESIAN_POINT('Ctrl Pts',(-8.84616049271118,1.13884313158887,5.09281961838548));
#12443=CARTESIAN_POINT('Ctrl Pts',(-9.22329069938031,1.02432161980314,5.1087269595371));
#12444=CARTESIAN_POINT('Ctrl Pts',(-9.53735294816069,0.703803525049966,
5.12463430068873));
#12445=CARTESIAN_POINT('Ctrl Pts',(-9.64487175298678,0.324706029258399,
5.14054164184035));
#12446=CARTESIAN_POINT('Ctrl Pts',(-9.67460091651171,0.219884817168954,
5.14494005332854));
#12447=CARTESIAN_POINT('Ctrl Pts',(-9.68853914169805,0.110585013592906,
5.14933846481673));
#12448=CARTESIAN_POINT('Ctrl Pts',(-9.68763172722904,0.00105126113166729,
5.15373687630492));
#12449=CARTESIAN_POINT('Origin',(-8.5,0.,1.8));
#12450=CARTESIAN_POINT('',(-9.688225,-6.12843109593086E-14,5.49626312369518));
#12451=CARTESIAN_POINT('',(-9.68743616841376,-0.000177656540254041,5.45373687630491));
#12452=CARTESIAN_POINT('',(-9.688225,-1.45515594291686E-16,1.8));
#12453=CARTESIAN_POINT('Ctrl Pts',(-9.688225,-4.45199432874688E-14,5.49626312369518));
#12454=CARTESIAN_POINT('Ctrl Pts',(-9.68822500000001,0.298712821306043,
5.48425993690586));
#12455=CARTESIAN_POINT('Ctrl Pts',(-9.57054245632589,0.595858078271478,
5.47225675011654));
#12456=CARTESIAN_POINT('Ctrl Pts',(-9.36601586214939,0.813569405232675,
5.46025356332723));
#12457=CARTESIAN_POINT('Ctrl Pts',(-9.16148926797289,1.03128073219387,5.44825037653791));
#12458=CARTESIAN_POINT('Ctrl Pts',(-8.87226522412853,1.16727314847133,5.43624718974859));
#12459=CARTESIAN_POINT('Ctrl Pts',(-8.57413435701458,1.1859100926019,5.42424400295927));
#12460=CARTESIAN_POINT('Ctrl Pts',(-8.27600348990063,1.20454703673246,5.41224081616995));
#12461=CARTESIAN_POINT('Ctrl Pts',(-7.97209482032104,1.10563290540114,5.40023762938064));
#12462=CARTESIAN_POINT('Ctrl Pts',(-7.7420470537207,0.915087963996651,5.38823444259132));
#12463=CARTESIAN_POINT('Ctrl Pts',(-7.51199928712037,0.724543022592161,
5.376231255802));
#12464=CARTESIAN_POINT('Ctrl Pts',(-7.3582268807964,0.444367128061599,5.36422806901268));
#12465=CARTESIAN_POINT('Ctrl Pts',(-7.32102560975819,0.147979855990437,
5.35222488222337));
#12466=CARTESIAN_POINT('Ctrl Pts',(-7.28382433871998,-0.148407416080724,
5.34022169543405));
#12467=CARTESIAN_POINT('Ctrl Pts',(-7.3635846474463,-0.457895344721807,
5.32821850864473));
#12468=CARTESIAN_POINT('Ctrl Pts',(-7.53940549437872,-0.699383189957564,
5.31621532185541));
#12469=CARTESIAN_POINT('Ctrl Pts',(-7.71522634131115,-0.940871035193321,
5.3042121350661));
#12470=CARTESIAN_POINT('Ctrl Pts',(-7.98526240565767,-1.11182427083074,
5.29220894827678));
#12471=CARTESIAN_POINT('Ctrl Pts',(-8.27875123560099,-1.16744491727743,
5.28020576148746));
#12472=CARTESIAN_POINT('Ctrl Pts',(-8.5722400655443,-1.22306556372412,5.26820257469814));
#12473=CARTESIAN_POINT('Ctrl Pts',(-8.88610136059921,-1.1627698566703,5.25619938790882));
#12474=CARTESIAN_POINT('Ctrl Pts',(-9.13808834820077,-1.0023581747636,5.24419620111951));
#12475=CARTESIAN_POINT('Ctrl Pts',(-9.39007533580232,-0.841946492856899,
5.23219301433019));
#12476=CARTESIAN_POINT('Ctrl Pts',(-9.57754329642126,-0.583102430603111,
5.22018982754087));
#12477=CARTESIAN_POINT('Ctrl Pts',(-9.65136659729185,-0.293655596346435,
5.20818664075155));
#12478=CARTESIAN_POINT('Ctrl Pts',(-9.6758110331054,-0.19781370797267,5.2042121350661));
#12479=CARTESIAN_POINT('Ctrl Pts',(-9.688225,-0.0989100500924914,5.20023762938064));
#12480=CARTESIAN_POINT('Ctrl Pts',(-9.688225,-3.61932706027801E-14,5.19626312369518));
#12481=CARTESIAN_POINT('Ctrl Pts',(-9.68763172722904,0.00105126113166729,
5.15373687630492));
#12482=CARTESIAN_POINT('Ctrl Pts',(-9.68525737700568,-0.285555905167675,
5.16524580596835));
#12483=CARTESIAN_POINT('Ctrl Pts',(-9.58124012083503,-0.573764837715244,
5.17675473563178));
#12484=CARTESIAN_POINT('Ctrl Pts',(-9.39251500118686,-0.787532689948571,
5.18826366529521));
#12485=CARTESIAN_POINT('Ctrl Pts',(-9.13166408368907,-1.08299701653396,
5.20417100644683));
#12486=CARTESIAN_POINT('Ctrl Pts',(-8.7089868878217,-1.23624877287478,5.22007834759846));
#12487=CARTESIAN_POINT('Ctrl Pts',(-8.3197251524468,-1.17657974317491,5.23598568875008));
#12488=CARTESIAN_POINT('Ctrl Pts',(-7.9304634170719,-1.11691071347503,5.25189302990169));
#12489=CARTESIAN_POINT('Ctrl Pts',(-7.57461714218948,-0.844320897734477,
5.26780037105331));
#12490=CARTESIAN_POINT('Ctrl Pts',(-7.4133485788613,-0.484440061841653,
5.28370771220493));
#12491=CARTESIAN_POINT('Ctrl Pts',(-7.33271429719722,-0.304499643895246,
5.29166138278075));
#12492=CARTESIAN_POINT('Ctrl Pts',(-7.30072444342169,-0.102736470910765,
5.29961505335656));
#12493=CARTESIAN_POINT('Ctrl Pts',(-7.31664171845983,0.0951736863613,5.30756872393237));
#12494=CARTESIAN_POINT('Ctrl Pts',(-7.33255899349796,0.29308384363337,5.31552239450818));
#12495=CARTESIAN_POINT('Ctrl Pts',(-7.39638339734975,0.487140985193029,
5.32347606508399));
#12496=CARTESIAN_POINT('Ctrl Pts',(-7.50473925661838,0.651881536219088,
5.33142973565979));
#12497=CARTESIAN_POINT('Ctrl Pts',(-7.72145097515565,0.981362638271211,
5.34733707681141));
#12498=CARTESIAN_POINT('Ctrl Pts',(-8.11628851536029,1.19357737818891,5.36324441796304));
#12499=CARTESIAN_POINT('Ctrl Pts',(-8.51008305302381,1.19026771978055,5.37915175911466));
#12500=CARTESIAN_POINT('Ctrl Pts',(-8.90387759068732,1.18695806137218,5.39505910026629));
#12501=CARTESIAN_POINT('Ctrl Pts',(-9.29662912580972,0.968124004637758,
5.4109664414179));
#12502=CARTESIAN_POINT('Ctrl Pts',(-9.50690608495474,0.6347683838711,5.42687378256952));
#12503=CARTESIAN_POINT('Ctrl Pts',(-9.62527260118696,0.447119943181184,
5.43582814714798));
#12504=CARTESIAN_POINT('Ctrl Pts',(-9.68581929966714,0.2231836200531,5.44478251172644));
#12505=CARTESIAN_POINT('Ctrl Pts',(-9.68639654153517,-0.000411795887354318,
5.45373687630491));
#12506=CARTESIAN_POINT('Origin',(-8.5,0.,1.8));
#12507=CARTESIAN_POINT('',(-9.688225,-6.94999613415348E-14,5.79626312369518));
#12508=CARTESIAN_POINT('',(-9.688225,-1.8036128146548E-12,5.75373687630491));
#12509=CARTESIAN_POINT('',(-9.688225,-1.45515594291686E-16,1.8));
#12510=CARTESIAN_POINT('Ctrl Pts',(-9.688225,-5.26245713672324E-14,5.79626312369518));
#12511=CARTESIAN_POINT('Ctrl Pts',(-9.68822500000001,0.29871282130603,5.78425993690586));
#12512=CARTESIAN_POINT('Ctrl Pts',(-9.5705424563259,0.595858078271459,5.77225675011654));
#12513=CARTESIAN_POINT('Ctrl Pts',(-9.36601586214941,0.813569405232657,
5.76025356332723));
#12514=CARTESIAN_POINT('Ctrl Pts',(-9.16148926797292,1.03128073219385,5.74825037653791));
#12515=CARTESIAN_POINT('Ctrl Pts',(-8.87226522412857,1.16727314847132,5.73624718974859));
#12516=CARTESIAN_POINT('Ctrl Pts',(-8.57413435701462,1.18591009260189,5.72424400295927));
#12517=CARTESIAN_POINT('Ctrl Pts',(-8.27600348990068,1.20454703673247,5.71224081616996));
#12518=CARTESIAN_POINT('Ctrl Pts',(-7.97209482032109,1.10563290540116,5.70023762938064));
#12519=CARTESIAN_POINT('Ctrl Pts',(-7.74204705372075,0.915087963996688,
5.68823444259132));
#12520=CARTESIAN_POINT('Ctrl Pts',(-7.51199928712041,0.724543022592213,
5.676231255802));
#12521=CARTESIAN_POINT('Ctrl Pts',(-7.35822688079642,0.444367128061666,
5.66422806901269));
#12522=CARTESIAN_POINT('Ctrl Pts',(-7.3210256097582,0.147979855990512,5.65222488222337));
#12523=CARTESIAN_POINT('Ctrl Pts',(-7.28382433871997,-0.148407416080641,
5.64022169543405));
#12524=CARTESIAN_POINT('Ctrl Pts',(-7.36358464744627,-0.457895344721723,
5.62821850864473));
#12525=CARTESIAN_POINT('Ctrl Pts',(-7.53940549437867,-0.699383189957489,
5.61621532185542));
#12526=CARTESIAN_POINT('Ctrl Pts',(-7.71522634131107,-0.940871035193256,
5.6042121350661));
#12527=CARTESIAN_POINT('Ctrl Pts',(-7.98526240565758,-1.1118242708307,5.59220894827678));
#12528=CARTESIAN_POINT('Ctrl Pts',(-8.27875123560088,-1.16744491727741,
5.58020576148746));
#12529=CARTESIAN_POINT('Ctrl Pts',(-8.57224006554418,-1.22306556372413,
5.56820257469815));
#12530=CARTESIAN_POINT('Ctrl Pts',(-8.88610136059909,-1.16276985667034,
5.55619938790883));
#12531=CARTESIAN_POINT('Ctrl Pts',(-9.13808834820066,-1.00235817476367,
5.54419620111951));
#12532=CARTESIAN_POINT('Ctrl Pts',(-9.39007533580222,-0.841946492856997,
5.5321930143302));
#12533=CARTESIAN_POINT('Ctrl Pts',(-9.57754329642119,-0.583102430603236,
5.52018982754088));
#12534=CARTESIAN_POINT('Ctrl Pts',(-9.65136659729182,-0.293655596346573,
5.50818664075156));
#12535=CARTESIAN_POINT('Ctrl Pts',(-9.67581103310539,-0.197813707972768,
5.5042121350661));
#12536=CARTESIAN_POINT('Ctrl Pts',(-9.688225,-0.0989100500925447,5.50023762938064));
#12537=CARTESIAN_POINT('Ctrl Pts',(-9.688225,-4.45199432874688E-14,5.49626312369518));
#12538=CARTESIAN_POINT('Ctrl Pts',(-9.688225,-1.76175740662643E-12,5.45373687630491));
#12539=CARTESIAN_POINT('Ctrl Pts',(-9.68822499999956,-0.298712821307844,
5.46574006309423));
#12540=CARTESIAN_POINT('Ctrl Pts',(-9.57054245632499,-0.595858078273094,
5.47774324988354));
#12541=CARTESIAN_POINT('Ctrl Pts',(-9.36601586214817,-0.813569405233979,
5.48974643667286));
#12542=CARTESIAN_POINT('Ctrl Pts',(-9.16148926797134,-1.03128073219486,
5.50174962346218));
#12543=CARTESIAN_POINT('Ctrl Pts',(-8.87226522412679,-1.16727314847189,
5.5137528102515));
#12544=CARTESIAN_POINT('Ctrl Pts',(-8.57413435701281,-1.18591009260201,
5.52575599704081));
#12545=CARTESIAN_POINT('Ctrl Pts',(-8.27600348989884,-1.20454703673212,
5.53775918383013));
#12546=CARTESIAN_POINT('Ctrl Pts',(-7.9720948203194,-1.10563290540036,5.54976237061945));
#12547=CARTESIAN_POINT('Ctrl Pts',(-7.74204705371935,-0.915087963995531,
5.56176555740877));
#12548=CARTESIAN_POINT('Ctrl Pts',(-7.5119992871193,-0.724543022590704,
5.57376874419808));
#12549=CARTESIAN_POINT('Ctrl Pts',(-7.35822688079574,-0.444367128059923,
5.5857719309874));
#12550=CARTESIAN_POINT('Ctrl Pts',(-7.32102560975797,-0.147979855988712,
5.59777511777672));
#12551=CARTESIAN_POINT('Ctrl Pts',(-7.2838243387202,0.148407416082498,5.60977830456603));
#12552=CARTESIAN_POINT('Ctrl Pts',(-7.36358464744697,0.457895344723458,
5.62178149135535));
#12553=CARTESIAN_POINT('Ctrl Pts',(-7.53940549437974,0.699383189958956,
5.63378467814467));
#12554=CARTESIAN_POINT('Ctrl Pts',(-7.71522634131251,0.940871035194454,
5.64578786493399));
#12555=CARTESIAN_POINT('Ctrl Pts',(-7.98526240565927,1.11182427083148,5.65779105172331));
#12556=CARTESIAN_POINT('Ctrl Pts',(-8.27875123560266,1.16744491727775,5.66979423851262));
#12557=CARTESIAN_POINT('Ctrl Pts',(-8.57224006554605,1.22306556372401,5.68179742530194));
#12558=CARTESIAN_POINT('Ctrl Pts',(-8.88610136060087,1.16276985666975,5.69380061209126));
#12559=CARTESIAN_POINT('Ctrl Pts',(-9.13808834820219,1.0023581747627,5.70580379888057));
#12560=CARTESIAN_POINT('Ctrl Pts',(-9.39007533580351,0.841946492855637,
5.71780698566989));
#12561=CARTESIAN_POINT('Ctrl Pts',(-9.57754329642208,0.58310243060159,5.72981017245921));
#12562=CARTESIAN_POINT('Ctrl Pts',(-9.65136659729227,0.293655596344815,
5.74181335924853));
#12563=CARTESIAN_POINT('Ctrl Pts',(-9.67581103310569,0.197813707970967,
5.74578786493399));
#12564=CARTESIAN_POINT('Ctrl Pts',(-9.68822500000015,0.098910050090719,
5.74976237061945));
#12565=CARTESIAN_POINT('Ctrl Pts',(-9.688225,-1.78679293583173E-12,5.75373687630491));
#12566=CARTESIAN_POINT('Origin',(-8.5,0.,1.8));
#12567=CARTESIAN_POINT('',(-9.688225,-7.7715611723761E-14,6.09626312369518));
#12568=CARTESIAN_POINT('',(-9.688225,-1.81177295388579E-12,6.05373687630491));
#12569=CARTESIAN_POINT('',(-9.688225,-1.45515594291686E-16,1.8));
#12570=CARTESIAN_POINT('Ctrl Pts',(-9.688225,-7.7715611723761E-14,6.09626312369518));
#12571=CARTESIAN_POINT('Ctrl Pts',(-9.68822500000002,0.29871282130601,6.08425993690586));
#12572=CARTESIAN_POINT('Ctrl Pts',(-9.5705424563259,0.595858078271448,6.07225675011654));
#12573=CARTESIAN_POINT('Ctrl Pts',(-9.36601586214941,0.813569405232651,
6.06025356332723));
#12574=CARTESIAN_POINT('Ctrl Pts',(-9.16148926797292,1.03128073219385,6.04825037653791));
#12575=CARTESIAN_POINT('Ctrl Pts',(-8.87226522412857,1.16727314847132,6.03624718974859));
#12576=CARTESIAN_POINT('Ctrl Pts',(-8.57413435701461,1.18591009260189,6.02424400295927));
#12577=CARTESIAN_POINT('Ctrl Pts',(-8.27600348990066,1.20454703673246,6.01224081616996));
#12578=CARTESIAN_POINT('Ctrl Pts',(-7.97209482032107,1.10563290540116,6.00023762938064));
#12579=CARTESIAN_POINT('Ctrl Pts',(-7.74204705372073,0.915087963996672,
5.98823444259132));
#12580=CARTESIAN_POINT('Ctrl Pts',(-7.51199928712039,0.724543022592188,
5.976231255802));
#12581=CARTESIAN_POINT('Ctrl Pts',(-7.35822688079641,0.444367128061631,
5.96422806901269));
#12582=CARTESIAN_POINT('Ctrl Pts',(-7.32102560975819,0.14797985599047,5.95222488222337));
#12583=CARTESIAN_POINT('Ctrl Pts',(-7.28382433871998,-0.14840741608069,
5.94022169543405));
#12584=CARTESIAN_POINT('Ctrl Pts',(-7.36358464744629,-0.457895344721775,
5.92821850864473));
#12585=CARTESIAN_POINT('Ctrl Pts',(-7.53940549437871,-0.699383189957538,
5.91621532185541));
#12586=CARTESIAN_POINT('Ctrl Pts',(-7.71522634131112,-0.9408710351933,5.9042121350661));
#12587=CARTESIAN_POINT('Ctrl Pts',(-7.98526240565764,-1.11182427083073,
5.89220894827678));
#12588=CARTESIAN_POINT('Ctrl Pts',(-8.27875123560095,-1.16744491727743,
5.88020576148746));
#12589=CARTESIAN_POINT('Ctrl Pts',(-8.57224006554427,-1.22306556372412,
5.86820257469814));
#12590=CARTESIAN_POINT('Ctrl Pts',(-8.88610136059918,-1.16276985667032,
5.85619938790883));
#12591=CARTESIAN_POINT('Ctrl Pts',(-9.13808834820074,-1.00235817476362,
5.84419620111951));
#12592=CARTESIAN_POINT('Ctrl Pts',(-9.3900753358023,-0.841946492856924,
5.83219301433019));
#12593=CARTESIAN_POINT('Ctrl Pts',(-9.57754329642124,-0.583102430603142,
5.82018982754087));
#12594=CARTESIAN_POINT('Ctrl Pts',(-9.65136659729185,-0.293655596346467,
5.80818664075156));
#12595=CARTESIAN_POINT('Ctrl Pts',(-9.6758110331054,-0.197813707972697,
5.8042121350661));
#12596=CARTESIAN_POINT('Ctrl Pts',(-9.688225,-0.0989100500925134,5.80023762938064));
#12597=CARTESIAN_POINT('Ctrl Pts',(-9.688225,-5.26245713672324E-14,5.79626312369518));
#12598=CARTESIAN_POINT('Ctrl Pts',(-9.688225,-1.78679293583173E-12,5.75373687630491));
#12599=CARTESIAN_POINT('Ctrl Pts',(-9.68822499999955,-0.298712821307875,
5.76574006309423));
#12600=CARTESIAN_POINT('Ctrl Pts',(-9.57054245632497,-0.595858078273127,
5.77774324988355));
#12601=CARTESIAN_POINT('Ctrl Pts',(-9.36601586214814,-0.813569405234009,
5.78974643667286));
#12602=CARTESIAN_POINT('Ctrl Pts',(-9.16148926797131,-1.03128073219489,
5.80174962346218));
#12603=CARTESIAN_POINT('Ctrl Pts',(-8.87226522412674,-1.16727314847191,
5.8137528102515));
#12604=CARTESIAN_POINT('Ctrl Pts',(-8.57413435701275,-1.18591009260201,
5.82575599704082));
#12605=CARTESIAN_POINT('Ctrl Pts',(-8.27600348989877,-1.20454703673211,
5.83775918383013));
#12606=CARTESIAN_POINT('Ctrl Pts',(-7.97209482031934,-1.10563290540033,
5.84976237061945));
#12607=CARTESIAN_POINT('Ctrl Pts',(-7.74204705371929,-0.915087963995482,
5.86176555740877));
#12608=CARTESIAN_POINT('Ctrl Pts',(-7.51199928711925,-0.724543022590638,
5.87376874419809));
#12609=CARTESIAN_POINT('Ctrl Pts',(-7.35822688079571,-0.444367128059839,
5.8857719309874));
#12610=CARTESIAN_POINT('Ctrl Pts',(-7.32102560975796,-0.14797985598862,
5.89777511777672));
#12611=CARTESIAN_POINT('Ctrl Pts',(-7.28382433872021,0.148407416082598,
5.90977830456604));
#12612=CARTESIAN_POINT('Ctrl Pts',(-7.36358464744701,0.457895344723558,
5.92178149135536));
#12613=CARTESIAN_POINT('Ctrl Pts',(-7.5394054943798,0.699383189959045,5.93378467814467));
#12614=CARTESIAN_POINT('Ctrl Pts',(-7.7152263413126,0.940871035194531,5.94578786493399));
#12615=CARTESIAN_POINT('Ctrl Pts',(-7.98526240565939,1.11182427083154,5.95779105172331));
#12616=CARTESIAN_POINT('Ctrl Pts',(-8.27875123560279,1.16744491727777,5.96979423851263));
#12617=CARTESIAN_POINT('Ctrl Pts',(-8.57224006554618,1.22306556372401,5.98179742530195));
#12618=CARTESIAN_POINT('Ctrl Pts',(-8.886101360601,1.16276985666971,5.99380061209126));
#12619=CARTESIAN_POINT('Ctrl Pts',(-9.13808834820231,1.00235817476262,6.00580379888058));
#12620=CARTESIAN_POINT('Ctrl Pts',(-9.39007533580362,0.841946492855527,
6.0178069856699));
#12621=CARTESIAN_POINT('Ctrl Pts',(-9.57754329642215,0.583102430601451,
6.02981017245922));
#12622=CARTESIAN_POINT('Ctrl Pts',(-9.65136659729231,0.29365559634466,6.04181335924853));
#12623=CARTESIAN_POINT('Ctrl Pts',(-9.67581103310571,0.197813707970852,
6.04578786493399));
#12624=CARTESIAN_POINT('Ctrl Pts',(-9.68822500000015,0.098910050090649,
6.04976237061945));
#12625=CARTESIAN_POINT('Ctrl Pts',(-9.688225,-1.81177295388579E-12,6.05373687630491));
#12626=CARTESIAN_POINT('Origin',(-8.5,0.,1.8));
#12627=CARTESIAN_POINT('',(-9.688225,-8.57092175010621E-14,6.39626312369518));
#12628=CARTESIAN_POINT('',(-9.688225,-1.81987758196556E-12,6.35373687630491));
#12629=CARTESIAN_POINT('',(-9.688225,-1.45515594291686E-16,1.8));
#12630=CARTESIAN_POINT('Ctrl Pts',(-9.688225,-8.57092175010621E-14,6.39626312369518));
#12631=CARTESIAN_POINT('Ctrl Pts',(-9.68822500000002,0.298712821306008,
6.38425993690586));
#12632=CARTESIAN_POINT('Ctrl Pts',(-9.5705424563259,0.595858078271451,6.37225675011655));
#12633=CARTESIAN_POINT('Ctrl Pts',(-9.36601586214941,0.813569405232657,
6.36025356332723));
#12634=CARTESIAN_POINT('Ctrl Pts',(-9.16148926797291,1.03128073219386,6.34825037653791));
#12635=CARTESIAN_POINT('Ctrl Pts',(-8.87226522412855,1.16727314847133,6.33624718974859));
#12636=CARTESIAN_POINT('Ctrl Pts',(-8.57413435701459,1.18591009260189,6.32424400295927));
#12637=CARTESIAN_POINT('Ctrl Pts',(-8.27600348990063,1.20454703673246,6.31224081616995));
#12638=CARTESIAN_POINT('Ctrl Pts',(-7.97209482032103,1.10563290540114,6.30023762938064));
#12639=CARTESIAN_POINT('Ctrl Pts',(-7.7420470537207,0.915087963996645,6.28823444259132));
#12640=CARTESIAN_POINT('Ctrl Pts',(-7.51199928712036,0.724543022592149,
6.276231255802));
#12641=CARTESIAN_POINT('Ctrl Pts',(-7.35822688079639,0.444367128061579,
6.26422806901268));
#12642=CARTESIAN_POINT('Ctrl Pts',(-7.32102560975819,0.147979855990411,
6.25222488222337));
#12643=CARTESIAN_POINT('Ctrl Pts',(-7.28382433871999,-0.148407416080757,
6.24022169543405));
#12644=CARTESIAN_POINT('Ctrl Pts',(-7.36358464744632,-0.457895344721844,
6.22821850864473));
#12645=CARTESIAN_POINT('Ctrl Pts',(-7.53940549437875,-0.699383189957599,
6.21621532185541));
#12646=CARTESIAN_POINT('Ctrl Pts',(-7.71522634131118,-0.940871035193355,
6.20421213506609));
#12647=CARTESIAN_POINT('Ctrl Pts',(-7.98526240565772,-1.11182427083077,
6.19220894827678));
#12648=CARTESIAN_POINT('Ctrl Pts',(-8.27875123560104,-1.16744491727744,
6.18020576148746));
#12649=CARTESIAN_POINT('Ctrl Pts',(-8.57224006554437,-1.22306556372412,
6.16820257469814));
#12650=CARTESIAN_POINT('Ctrl Pts',(-8.88610136059928,-1.16276985667028,
6.15619938790882));
#12651=CARTESIAN_POINT('Ctrl Pts',(-9.13808834820083,-1.00235817476356,
6.14419620111951));
#12652=CARTESIAN_POINT('Ctrl Pts',(-9.39007533580238,-0.841946492856838,
6.13219301433019));
#12653=CARTESIAN_POINT('Ctrl Pts',(-9.5775432964213,-0.583102430603032,
6.12018982754087));
#12654=CARTESIAN_POINT('Ctrl Pts',(-9.65136659729188,-0.293655596346344,
6.10818664075155));
#12655=CARTESIAN_POINT('Ctrl Pts',(-9.67581103310541,-0.197813707972621,
6.10421213506609));
#12656=CARTESIAN_POINT('Ctrl Pts',(-9.68822499999999,-0.0989100500924879,
6.10023762938064));
#12657=CARTESIAN_POINT('Ctrl Pts',(-9.688225,-7.7715611723761E-14,6.09626312369518));
#12658=CARTESIAN_POINT('Ctrl Pts',(-9.688225,-1.81177295388579E-12,6.05373687630491));
#12659=CARTESIAN_POINT('Ctrl Pts',(-9.68822499999954,-0.2987128213079,6.06574006309423));
#12660=CARTESIAN_POINT('Ctrl Pts',(-9.57054245632496,-0.59585807827315,
6.07774324988355));
#12661=CARTESIAN_POINT('Ctrl Pts',(-9.36601586214812,-0.813569405234027,
6.08974643667286));
#12662=CARTESIAN_POINT('Ctrl Pts',(-9.16148926797128,-1.03128073219491,
6.10174962346218));
#12663=CARTESIAN_POINT('Ctrl Pts',(-8.87226522412671,-1.16727314847191,
6.1137528102515));
#12664=CARTESIAN_POINT('Ctrl Pts',(-8.57413435701273,-1.18591009260201,
6.12575599704082));
#12665=CARTESIAN_POINT('Ctrl Pts',(-8.27600348989875,-1.20454703673211,
6.13775918383013));
#12666=CARTESIAN_POINT('Ctrl Pts',(-7.97209482031931,-1.10563290540032,
6.14976237061945));
#12667=CARTESIAN_POINT('Ctrl Pts',(-7.74204705371927,-0.915087963995467,
6.16176555740877));
#12668=CARTESIAN_POINT('Ctrl Pts',(-7.51199928711924,-0.724543022590617,
6.17376874419809));
#12669=CARTESIAN_POINT('Ctrl Pts',(-7.3582268807957,-0.444367128059815,
6.18577193098741));
#12670=CARTESIAN_POINT('Ctrl Pts',(-7.32102560975796,-0.147979855988595,
6.19777511777672));
#12671=CARTESIAN_POINT('Ctrl Pts',(-7.28382433872022,0.148407416082624,
6.20977830456604));
#12672=CARTESIAN_POINT('Ctrl Pts',(-7.36358464744702,0.457895344723582,
6.22178149135536));
#12673=CARTESIAN_POINT('Ctrl Pts',(-7.53940549437982,0.699383189959065,
6.23378467814468));
#12674=CARTESIAN_POINT('Ctrl Pts',(-7.71522634131261,0.940871035194547,
6.24578786493399));
#12675=CARTESIAN_POINT('Ctrl Pts',(-7.98526240565941,1.11182427083155,6.25779105172331));
#12676=CARTESIAN_POINT('Ctrl Pts',(-8.27875123560281,1.16744491727778,6.26979423851263));
#12677=CARTESIAN_POINT('Ctrl Pts',(-8.57224006554621,1.22306556372401,6.28179742530195));
#12678=CARTESIAN_POINT('Ctrl Pts',(-8.88610136060103,1.1627698566697,6.29380061209126));
#12679=CARTESIAN_POINT('Ctrl Pts',(-9.13808834820233,1.0023581747626,6.30580379888058));
#12680=CARTESIAN_POINT('Ctrl Pts',(-9.39007533580363,0.841946492855508,
6.3178069856699));
#12681=CARTESIAN_POINT('Ctrl Pts',(-9.57754329642217,0.583102430601428,
6.32981017245922));
#12682=CARTESIAN_POINT('Ctrl Pts',(-9.65136659729231,0.293655596344636,
6.34181335924854));
#12683=CARTESIAN_POINT('Ctrl Pts',(-9.67581103310571,0.197813707970833,
6.34578786493399));
#12684=CARTESIAN_POINT('Ctrl Pts',(-9.68822500000015,0.0989100500906353,
6.34976237061945));
#12685=CARTESIAN_POINT('Ctrl Pts',(-9.688225,-1.81987758196556E-12,6.35373687630491));
#12686=CARTESIAN_POINT('Origin',(-8.5,0.,1.8));
#12687=CARTESIAN_POINT('',(-9.68779459938433,-0.000383426657895316,6.69626312369518));
#12688=CARTESIAN_POINT('',(-9.688225,-1.82809323234778E-12,6.65373687630491));
#12689=CARTESIAN_POINT('',(-9.688225,-1.45515594291686E-16,1.8));
#12690=CARTESIAN_POINT('Ctrl Pts',(-9.688225,-9.39248678832882E-14,6.69626312369518));
#12691=CARTESIAN_POINT('Ctrl Pts',(-9.68822500000002,0.298712821305994,
6.68425993690586));
#12692=CARTESIAN_POINT('Ctrl Pts',(-9.57054245632591,0.595858078271433,
6.67225675011654));
#12693=CARTESIAN_POINT('Ctrl Pts',(-9.36601586214942,0.813569405232639,
6.66025356332723));
#12694=CARTESIAN_POINT('Ctrl Pts',(-9.16148926797294,1.03128073219384,6.64825037653791));
#12695=CARTESIAN_POINT('Ctrl Pts',(-8.87226522412858,1.16727314847132,6.63624718974859));
#12696=CARTESIAN_POINT('Ctrl Pts',(-8.57413435701463,1.18591009260189,6.62424400295927));
#12697=CARTESIAN_POINT('Ctrl Pts',(-8.27600348990068,1.20454703673247,6.61224081616996));
#12698=CARTESIAN_POINT('Ctrl Pts',(-7.97209482032109,1.10563290540116,6.60023762938064));
#12699=CARTESIAN_POINT('Ctrl Pts',(-7.74204705372074,0.915087963996682,
6.58823444259132));
#12700=CARTESIAN_POINT('Ctrl Pts',(-7.5119992871204,0.724543022592202,6.576231255802));
#12701=CARTESIAN_POINT('Ctrl Pts',(-7.35822688079641,0.444367128061646,
6.56422806901269));
#12702=CARTESIAN_POINT('Ctrl Pts',(-7.32102560975819,0.147979855990486,
6.55222488222337));
#12703=CARTESIAN_POINT('Ctrl Pts',(-7.28382433871998,-0.148407416080674,
6.54022169543405));
#12704=CARTESIAN_POINT('Ctrl Pts',(-7.36358464744629,-0.45789534472176,
6.52821850864473));
#12705=CARTESIAN_POINT('Ctrl Pts',(-7.5394054943787,-0.699383189957524,
6.51621532185542));
#12706=CARTESIAN_POINT('Ctrl Pts',(-7.71522634131111,-0.940871035193289,
6.5042121350661));
#12707=CARTESIAN_POINT('Ctrl Pts',(-7.98526240565763,-1.11182427083072,
6.49220894827678));
#12708=CARTESIAN_POINT('Ctrl Pts',(-8.27875123560094,-1.16744491727742,
6.48020576148746));
#12709=CARTESIAN_POINT('Ctrl Pts',(-8.57224006554425,-1.22306556372412,
6.46820257469815));
#12710=CARTESIAN_POINT('Ctrl Pts',(-8.88610136059916,-1.16276985667032,
6.45619938790883));
#12711=CARTESIAN_POINT('Ctrl Pts',(-9.13808834820072,-1.00235817476363,
6.44419620111951));
#12712=CARTESIAN_POINT('Ctrl Pts',(-9.39007533580228,-0.841946492856936,
6.43219301433019));
#12713=CARTESIAN_POINT('Ctrl Pts',(-9.57754329642123,-0.583102430603156,
6.42018982754087));
#12714=CARTESIAN_POINT('Ctrl Pts',(-9.65136659729184,-0.293655596346483,
6.40818664075156));
#12715=CARTESIAN_POINT('Ctrl Pts',(-9.6758110331054,-0.197813707972719,
6.4042121350661));
#12716=CARTESIAN_POINT('Ctrl Pts',(-9.68822499999999,-0.0989100500925409,
6.40023762938064));
#12717=CARTESIAN_POINT('Ctrl Pts',(-9.688225,-8.57092175010621E-14,6.39626312369518));
#12718=CARTESIAN_POINT('Ctrl Pts',(-9.688225,-1.81987758196556E-12,6.35373687630491));
#12719=CARTESIAN_POINT('Ctrl Pts',(-9.68822499999954,-0.298712821307902,
6.36574006309423));
#12720=CARTESIAN_POINT('Ctrl Pts',(-9.57054245632496,-0.595858078273146,
6.37774324988355));
#12721=CARTESIAN_POINT('Ctrl Pts',(-9.36601586214813,-0.813569405234021,
6.38974643667286));
#12722=CARTESIAN_POINT('Ctrl Pts',(-9.16148926797129,-1.0312807321949,6.40174962346218));
#12723=CARTESIAN_POINT('Ctrl Pts',(-8.87226522412673,-1.16727314847191,
6.4137528102515));
#12724=CARTESIAN_POINT('Ctrl Pts',(-8.57413435701275,-1.18591009260201,
6.42575599704082));
#12725=CARTESIAN_POINT('Ctrl Pts',(-8.27600348989878,-1.20454703673211,
6.43775918383013));
#12726=CARTESIAN_POINT('Ctrl Pts',(-7.97209482031935,-1.10563290540033,
6.44976237061945));
#12727=CARTESIAN_POINT('Ctrl Pts',(-7.74204705371931,-0.915087963995493,
6.46176555740877));
#12728=CARTESIAN_POINT('Ctrl Pts',(-7.51199928711927,-0.724543022590656,
6.47376874419809));
#12729=CARTESIAN_POINT('Ctrl Pts',(-7.35822688079572,-0.444367128059867,
6.4857719309874));
#12730=CARTESIAN_POINT('Ctrl Pts',(-7.32102560975797,-0.147979855988654,
6.49777511777672));
#12731=CARTESIAN_POINT('Ctrl Pts',(-7.28382433872021,0.148407416082558,
6.50977830456604));
#12732=CARTESIAN_POINT('Ctrl Pts',(-7.36358464744699,0.457895344723514,
6.52178149135536));
#12733=CARTESIAN_POINT('Ctrl Pts',(-7.53940549437977,0.699383189959003,
6.53378467814467));
#12734=CARTESIAN_POINT('Ctrl Pts',(-7.71522634131255,0.940871035194492,
6.54578786493399));
#12735=CARTESIAN_POINT('Ctrl Pts',(-7.98526240565933,1.11182427083151,6.55779105172331));
#12736=CARTESIAN_POINT('Ctrl Pts',(-8.27875123560272,1.16744491727776,6.56979423851263));
#12737=CARTESIAN_POINT('Ctrl Pts',(-8.57224006554611,1.22306556372401,6.58179742530194));
#12738=CARTESIAN_POINT('Ctrl Pts',(-8.88610136060093,1.16276985666973,6.59380061209126));
#12739=CARTESIAN_POINT('Ctrl Pts',(-9.13808834820224,1.00235817476266,6.60580379888058));
#12740=CARTESIAN_POINT('Ctrl Pts',(-9.39007533580355,0.841946492855594,
6.61780698566989));
#12741=CARTESIAN_POINT('Ctrl Pts',(-9.57754329642211,0.583102430601538,
6.62981017245921));
#12742=CARTESIAN_POINT('Ctrl Pts',(-9.65136659729228,0.293655596344759,
6.64181335924853));
#12743=CARTESIAN_POINT('Ctrl Pts',(-9.6758110331057,0.19781370797092,6.64578786493399));
#12744=CARTESIAN_POINT('Ctrl Pts',(-9.68822500000015,0.0989100500906833,
6.64976237061945));
#12745=CARTESIAN_POINT('Ctrl Pts',(-9.688225,-1.81121784237348E-12,6.65373687630491));
#12746=CARTESIAN_POINT('Origin',(-8.5,0.,1.8));
#12747=CARTESIAN_POINT('',(-9.68888225390868,-0.000138896677983098,6.99626312369518));
#12748=CARTESIAN_POINT('',(-9.688225,-1.83614234927632E-12,6.95373687630491));
#12749=CARTESIAN_POINT('',(-9.688225,-1.45515594291686E-16,1.8));
#12750=CARTESIAN_POINT('Ctrl Pts',(-9.6902066384567,-0.00041877727094708,
6.99626312369518));
#12751=CARTESIAN_POINT('Ctrl Pts',(-9.68899674651061,0.379592025804337,
6.98092963956396));
#12752=CARTESIAN_POINT('Ctrl Pts',(-9.49087722055918,0.761025012956179,
6.96559615543274));
#12753=CARTESIAN_POINT('Ctrl Pts',(-9.1791037192896,0.977577133098408,6.95026267130152));
#12754=CARTESIAN_POINT('Ctrl Pts',(-8.85566206674089,1.20223373578116,6.9343553301499));
#12755=CARTESIAN_POINT('Ctrl Pts',(-8.40990023040919,1.24943717064941,6.91844798899829));
#12756=CARTESIAN_POINT('Ctrl Pts',(-8.0451996812129,1.0993862626989,6.90254064784667));
#12757=CARTESIAN_POINT('Ctrl Pts',(-7.86284940661476,1.02436080872364,6.89458697727086));
#12758=CARTESIAN_POINT('Ctrl Pts',(-7.70076445380047,0.900021769043694,
6.88663330669505));
#12759=CARTESIAN_POINT('Ctrl Pts',(-7.5760833820586,0.745501801578665,6.87867963611924));
#12760=CARTESIAN_POINT('Ctrl Pts',(-7.45140231031673,0.590981834113632,
6.87072596554343));
#12761=CARTESIAN_POINT('Ctrl Pts',(-7.36412511964729,0.406280938863516,
6.86277229496762));
#12762=CARTESIAN_POINT('Ctrl Pts',(-7.32933043709483,0.212193918544567,
6.85481862439181));
#12763=CARTESIAN_POINT('Ctrl Pts',(-7.25974107198991,-0.175980122093319,
6.83891128324018));
#12764=CARTESIAN_POINT('Ctrl Pts',(-7.40008173935293,-0.601698663006534,
6.82300394208856));
#12765=CARTESIAN_POINT('Ctrl Pts',(-7.6880176507503,-0.870358303928216,
6.80709660093694));
#12766=CARTESIAN_POINT('Ctrl Pts',(-7.97595356214767,-1.1390179448499,6.79118925978532));
#12767=CARTESIAN_POINT('Ctrl Pts',(-8.41148471757938,-1.25061868578005,
6.7752819186337));
#12768=CARTESIAN_POINT('Ctrl Pts',(-8.79347776741406,-1.15354304866133,
6.75937457748208));
#12769=CARTESIAN_POINT('Ctrl Pts',(-9.17547081724873,-1.05646741154261,
6.74346723633046));
#12770=CARTESIAN_POINT('Ctrl Pts',(-9.50392576148636,-0.750715396374999,
6.72755989517883));
#12771=CARTESIAN_POINT('Ctrl Pts',(-9.62874639685919,-0.376957434999199,
6.71165255402721));
#12772=CARTESIAN_POINT('Ctrl Pts',(-9.66899863959755,-0.256427715359838,
6.70652274391653));
#12773=CARTESIAN_POINT('Ctrl Pts',(-9.68807417965994,-0.128825799924604,
6.70139293380585));
#12774=CARTESIAN_POINT('Ctrl Pts',(-9.68716172628878,-0.00094722793280222,
6.69626312369518));
#12775=CARTESIAN_POINT('Ctrl Pts',(-9.688225,-1.81121784237348E-12,6.65373687630491));
#12776=CARTESIAN_POINT('Ctrl Pts',(-9.68822499999954,-0.298712821307899,
6.66574006309423));
#12777=CARTESIAN_POINT('Ctrl Pts',(-9.57054245632496,-0.595858078273149,
6.67774324988355));
#12778=CARTESIAN_POINT('Ctrl Pts',(-9.36601586214812,-0.813569405234027,
6.68974643667286));
#12779=CARTESIAN_POINT('Ctrl Pts',(-9.16148926797128,-1.0312807321949,6.70174962346218));
#12780=CARTESIAN_POINT('Ctrl Pts',(-8.87226522412671,-1.16727314847191,
6.7137528102515));
#12781=CARTESIAN_POINT('Ctrl Pts',(-8.57413435701273,-1.18591009260201,
6.72575599704082));
#12782=CARTESIAN_POINT('Ctrl Pts',(-8.27600348989875,-1.20454703673211,
6.73775918383013));
#12783=CARTESIAN_POINT('Ctrl Pts',(-7.97209482031931,-1.10563290540032,
6.74976237061945));
#12784=CARTESIAN_POINT('Ctrl Pts',(-7.74204705371928,-0.915087963995467,
6.76176555740877));
#12785=CARTESIAN_POINT('Ctrl Pts',(-7.51199928711924,-0.724543022590618,
6.77376874419809));
#12786=CARTESIAN_POINT('Ctrl Pts',(-7.3582268807957,-0.444367128059816,
6.78577193098741));
#12787=CARTESIAN_POINT('Ctrl Pts',(-7.32102560975796,-0.147979855988596,
6.79777511777672));
#12788=CARTESIAN_POINT('Ctrl Pts',(-7.28382433872022,0.148407416082623,
6.80977830456604));
#12789=CARTESIAN_POINT('Ctrl Pts',(-7.36358464744702,0.457895344723582,
6.82178149135536));
#12790=CARTESIAN_POINT('Ctrl Pts',(-7.53940549437982,0.699383189959064,
6.83378467814468));
#12791=CARTESIAN_POINT('Ctrl Pts',(-7.71522634131261,0.940871035194547,
6.84578786493399));
#12792=CARTESIAN_POINT('Ctrl Pts',(-7.98526240565941,1.11182427083155,6.85779105172331));
#12793=CARTESIAN_POINT('Ctrl Pts',(-8.27875123560281,1.16744491727778,6.86979423851263));
#12794=CARTESIAN_POINT('Ctrl Pts',(-8.57224006554621,1.22306556372401,6.88179742530195));
#12795=CARTESIAN_POINT('Ctrl Pts',(-8.88610136060103,1.1627698566697,6.89380061209126));
#12796=CARTESIAN_POINT('Ctrl Pts',(-9.13808834820233,1.00235817476261,6.90580379888058));
#12797=CARTESIAN_POINT('Ctrl Pts',(-9.39007533580363,0.841946492855509,
6.9178069856699));
#12798=CARTESIAN_POINT('Ctrl Pts',(-9.57754329642217,0.583102430601429,
6.92981017245922));
#12799=CARTESIAN_POINT('Ctrl Pts',(-9.65136659729231,0.293655596344637,
6.94181335924853));
#12800=CARTESIAN_POINT('Ctrl Pts',(-9.67581103310571,0.197813707970828,
6.94578786493399));
#12801=CARTESIAN_POINT('Ctrl Pts',(-9.68822500000015,0.0989100500906246,
6.94976237061945));
#12802=CARTESIAN_POINT('Ctrl Pts',(-9.688225,-1.83614234927632E-12,6.95373687630491));
#12803=CARTESIAN_POINT('Origin',(-8.5,0.,1.8));
#12804=CARTESIAN_POINT('',(-9.688225,-1.10245146345278E-13,7.29626312369518));
#12805=CARTESIAN_POINT('',(-9.688225,-1.84441351080977E-12,7.25373687630491));
#12806=CARTESIAN_POINT('',(-9.688225,-1.45515594291686E-16,1.8));
#12807=CARTESIAN_POINT('Ctrl Pts',(-9.688225,-1.10245146345278E-13,7.29626312369518));
#12808=CARTESIAN_POINT('Ctrl Pts',(-9.68822500000003,0.298712821305983,
7.28425993690586));
#12809=CARTESIAN_POINT('Ctrl Pts',(-9.57054245632592,0.59585807827143,7.27225675011655));
#12810=CARTESIAN_POINT('Ctrl Pts',(-9.36601586214942,0.813569405232639,
7.26025356332723));
#12811=CARTESIAN_POINT('Ctrl Pts',(-9.16148926797293,1.03128073219385,7.24825037653791));
#12812=CARTESIAN_POINT('Ctrl Pts',(-8.87226522412857,1.16727314847132,7.23624718974859));
#12813=CARTESIAN_POINT('Ctrl Pts',(-8.57413435701461,1.18591009260189,7.22424400295927));
#12814=CARTESIAN_POINT('Ctrl Pts',(-8.27600348990066,1.20454703673246,7.21224081616996));
#12815=CARTESIAN_POINT('Ctrl Pts',(-7.97209482032106,1.10563290540115,7.20023762938064));
#12816=CARTESIAN_POINT('Ctrl Pts',(-7.74204705372072,0.91508796399666,7.18823444259132));
#12817=CARTESIAN_POINT('Ctrl Pts',(-7.51199928712037,0.72454302259217,7.176231255802));
#12818=CARTESIAN_POINT('Ctrl Pts',(-7.35822688079639,0.444367128061603,
7.16422806901268));
#12819=CARTESIAN_POINT('Ctrl Pts',(-7.32102560975819,0.147979855990436,
7.15222488222337));
#12820=CARTESIAN_POINT('Ctrl Pts',(-7.28382433871998,-0.148407416080732,
7.14022169543405));
#12821=CARTESIAN_POINT('Ctrl Pts',(-7.36358464744631,-0.45789534472182,
7.12821850864473));
#12822=CARTESIAN_POINT('Ctrl Pts',(-7.53940549437874,-0.699383189957579,
7.11621532185541));
#12823=CARTESIAN_POINT('Ctrl Pts',(-7.71522634131116,-0.940871035193338,
7.10421213506609));
#12824=CARTESIAN_POINT('Ctrl Pts',(-7.9852624056577,-1.11182427083076,7.09220894827678));
#12825=CARTESIAN_POINT('Ctrl Pts',(-8.27875123560102,-1.16744491727744,
7.08020576148746));
#12826=CARTESIAN_POINT('Ctrl Pts',(-8.57224006554434,-1.22306556372412,
7.06820257469814));
#12827=CARTESIAN_POINT('Ctrl Pts',(-8.88610136059926,-1.16276985667029,
7.05619938790882));
#12828=CARTESIAN_POINT('Ctrl Pts',(-9.13808834820081,-1.00235817476357,
7.04419620111951));
#12829=CARTESIAN_POINT('Ctrl Pts',(-9.39007533580236,-0.841946492856857,
7.03219301433019));
#12830=CARTESIAN_POINT('Ctrl Pts',(-9.57754329642129,-0.583102430603054,
7.02018982754087));
#12831=CARTESIAN_POINT('Ctrl Pts',(-9.65136659729187,-0.293655596346368,
7.00818664075155));
#12832=CARTESIAN_POINT('Ctrl Pts',(-9.6758110331054,-0.197813707972645,
7.0042121350661));
#12833=CARTESIAN_POINT('Ctrl Pts',(-9.68822499999999,-0.0989100500925123,
7.00023762938064));
#12834=CARTESIAN_POINT('Ctrl Pts',(-9.688225,-1.02140518265514E-13,6.99626312369518));
#12835=CARTESIAN_POINT('Ctrl Pts',(-9.688225,-1.83614234927632E-12,6.95373687630491));
#12836=CARTESIAN_POINT('Ctrl Pts',(-9.68822499999954,-0.298712821307918,
6.96574006309423));
#12837=CARTESIAN_POINT('Ctrl Pts',(-9.57054245632495,-0.595858078273161,
6.97774324988355));
#12838=CARTESIAN_POINT('Ctrl Pts',(-9.36601586214811,-0.813569405234033,
6.98974643667286));
#12839=CARTESIAN_POINT('Ctrl Pts',(-9.16148926797128,-1.03128073219491,
7.00174962346218));
#12840=CARTESIAN_POINT('Ctrl Pts',(-8.87226522412671,-1.16727314847191,
7.0137528102515));
#12841=CARTESIAN_POINT('Ctrl Pts',(-8.57413435701274,-1.18591009260201,
7.02575599704082));
#12842=CARTESIAN_POINT('Ctrl Pts',(-8.27600348989876,-1.20454703673211,
7.03775918383013));
#12843=CARTESIAN_POINT('Ctrl Pts',(-7.97209482031933,-1.10563290540032,
7.04976237061945));
#12844=CARTESIAN_POINT('Ctrl Pts',(-7.7420470537193,-0.915087963995483,
7.06176555740877));
#12845=CARTESIAN_POINT('Ctrl Pts',(-7.51199928711926,-0.724543022590642,
7.07376874419809));
#12846=CARTESIAN_POINT('Ctrl Pts',(-7.35822688079572,-0.444367128059851,
7.0857719309874));
#12847=CARTESIAN_POINT('Ctrl Pts',(-7.32102560975796,-0.147979855988638,
7.09777511777672));
#12848=CARTESIAN_POINT('Ctrl Pts',(-7.28382433872021,0.148407416082574,
7.10977830456604));
#12849=CARTESIAN_POINT('Ctrl Pts',(-7.363584647447,0.457895344723529,7.12178149135536));
#12850=CARTESIAN_POINT('Ctrl Pts',(-7.53940549437978,0.699383189959016,
7.13378467814467));
#12851=CARTESIAN_POINT('Ctrl Pts',(-7.71522634131256,0.940871035194503,
7.14578786493399));
#12852=CARTESIAN_POINT('Ctrl Pts',(-7.98526240565934,1.11182427083152,7.15779105172331));
#12853=CARTESIAN_POINT('Ctrl Pts',(-8.27875123560274,1.16744491727776,7.16979423851263));
#12854=CARTESIAN_POINT('Ctrl Pts',(-8.57224006554613,1.22306556372401,7.18179742530194));
#12855=CARTESIAN_POINT('Ctrl Pts',(-8.88610136060094,1.16276985666973,7.19380061209126));
#12856=CARTESIAN_POINT('Ctrl Pts',(-9.13808834820225,1.00235817476266,7.20580379888058));
#12857=CARTESIAN_POINT('Ctrl Pts',(-9.39007533580356,0.841946492855582,
7.2178069856699));
#12858=CARTESIAN_POINT('Ctrl Pts',(-9.57754329642211,0.583102430601523,
7.22981017245921));
#12859=CARTESIAN_POINT('Ctrl Pts',(-9.65136659729228,0.293655596344743,
7.24181335924853));
#12860=CARTESIAN_POINT('Ctrl Pts',(-9.6758110331057,0.197813707970899,7.24578786493399));
#12861=CARTESIAN_POINT('Ctrl Pts',(-9.68822500000015,0.0989100500906558,
7.24976237061945));
#12862=CARTESIAN_POINT('Ctrl Pts',(-9.688225,-1.84441351080977E-12,7.25373687630491));
#12863=CARTESIAN_POINT('Origin',(-8.5,0.,1.8));
#12864=CARTESIAN_POINT('',(-9.688225,-1.18460796727504E-13,7.59626312369518));
#12865=CARTESIAN_POINT('',(-9.688225,-1.85257365004077E-12,7.55373687630491));
#12866=CARTESIAN_POINT('',(-9.688225,-1.45515594291686E-16,1.8));
#12867=CARTESIAN_POINT('Ctrl Pts',(-9.688225,-8.47100167788994E-14,7.59626312369518));
#12868=CARTESIAN_POINT('Ctrl Pts',(-9.68822500000002,0.298712821306009,
7.58425993690586));
#12869=CARTESIAN_POINT('Ctrl Pts',(-9.5705424563259,0.595858078271453,7.57225675011655));
#12870=CARTESIAN_POINT('Ctrl Pts',(-9.36601586214941,0.813569405232658,
7.56025356332723));
#12871=CARTESIAN_POINT('Ctrl Pts',(-9.16148926797291,1.03128073219386,7.54825037653791));
#12872=CARTESIAN_POINT('Ctrl Pts',(-8.87226522412855,1.16727314847133,7.53624718974859));
#12873=CARTESIAN_POINT('Ctrl Pts',(-8.57413435701459,1.18591009260189,7.52424400295927));
#12874=CARTESIAN_POINT('Ctrl Pts',(-8.27600348990063,1.20454703673246,7.51224081616995));
#12875=CARTESIAN_POINT('Ctrl Pts',(-7.97209482032103,1.10563290540114,7.50023762938064));
#12876=CARTESIAN_POINT('Ctrl Pts',(-7.7420470537207,0.915087963996644,7.48823444259132));
#12877=CARTESIAN_POINT('Ctrl Pts',(-7.51199928712036,0.724543022592149,
7.476231255802));
#12878=CARTESIAN_POINT('Ctrl Pts',(-7.35822688079639,0.444367128061578,
7.46422806901268));
#12879=CARTESIAN_POINT('Ctrl Pts',(-7.32102560975819,0.14797985599041,7.45222488222337));
#12880=CARTESIAN_POINT('Ctrl Pts',(-7.28382433871999,-0.148407416080758,
7.44022169543405));
#12881=CARTESIAN_POINT('Ctrl Pts',(-7.36358464744632,-0.457895344721845,
7.42821850864473));
#12882=CARTESIAN_POINT('Ctrl Pts',(-7.53940549437875,-0.6993831899576,7.41621532185541));
#12883=CARTESIAN_POINT('Ctrl Pts',(-7.71522634131118,-0.940871035193355,
7.40421213506609));
#12884=CARTESIAN_POINT('Ctrl Pts',(-7.98526240565772,-1.11182427083077,
7.39220894827678));
#12885=CARTESIAN_POINT('Ctrl Pts',(-8.27875123560105,-1.16744491727744,
7.38020576148746));
#12886=CARTESIAN_POINT('Ctrl Pts',(-8.57224006554437,-1.22306556372412,
7.36820257469814));
#12887=CARTESIAN_POINT('Ctrl Pts',(-8.88610136059928,-1.16276985667028,
7.35619938790882));
#12888=CARTESIAN_POINT('Ctrl Pts',(-9.13808834820083,-1.00235817476356,
7.34419620111951));
#12889=CARTESIAN_POINT('Ctrl Pts',(-9.39007533580238,-0.841946492856837,
7.33219301433019));
#12890=CARTESIAN_POINT('Ctrl Pts',(-9.5775432964213,-0.583102430603031,
7.32018982754087));
#12891=CARTESIAN_POINT('Ctrl Pts',(-9.65136659729188,-0.293655596346343,
7.30818664075155));
#12892=CARTESIAN_POINT('Ctrl Pts',(-9.6758110331054,-0.19781370797263,7.30421213506609));
#12893=CARTESIAN_POINT('Ctrl Pts',(-9.68822499999999,-0.0989100500925091,
7.30023762938064));
#12894=CARTESIAN_POINT('Ctrl Pts',(-9.688225,-1.10245146345278E-13,7.29626312369518));
#12895=CARTESIAN_POINT('Ctrl Pts',(-9.688225,-1.84441351080977E-12,7.25373687630491));
#12896=CARTESIAN_POINT('Ctrl Pts',(-9.68822499999954,-0.298712821307943,
7.26574006309423));
#12897=CARTESIAN_POINT('Ctrl Pts',(-9.57054245632493,-0.595858078273201,
7.27774324988355));
#12898=CARTESIAN_POINT('Ctrl Pts',(-9.36601586214807,-0.813569405234076,
7.28974643667287));
#12899=CARTESIAN_POINT('Ctrl Pts',(-9.16148926797122,-1.03128073219495,
7.30174962346219));
#12900=CARTESIAN_POINT('Ctrl Pts',(-8.87226522412662,-1.16727314847194,
7.3137528102515));
#12901=CARTESIAN_POINT('Ctrl Pts',(-8.57413435701263,-1.18591009260202,
7.32575599704082));
#12902=CARTESIAN_POINT('Ctrl Pts',(-8.27600348989864,-1.20454703673209,
7.33775918383014));
#12903=CARTESIAN_POINT('Ctrl Pts',(-7.9720948203192,-1.10563290540026,7.34976237061946));
#12904=CARTESIAN_POINT('Ctrl Pts',(-7.74204705371917,-0.915087963995381,
7.36176555740878));
#12905=CARTESIAN_POINT('Ctrl Pts',(-7.51199928711915,-0.724543022590499,
7.37376874419809));
#12906=CARTESIAN_POINT('Ctrl Pts',(-7.35822688079564,-0.444367128059665,
7.38577193098741));
#12907=CARTESIAN_POINT('Ctrl Pts',(-7.32102560975794,-0.147979855988429,
7.39777511777673));
#12908=CARTESIAN_POINT('Ctrl Pts',(-7.28382433872024,0.148407416082807,
7.40977830456605));
#12909=CARTESIAN_POINT('Ctrl Pts',(-7.36358464744709,0.457895344723766,
7.42178149135537));
#12910=CARTESIAN_POINT('Ctrl Pts',(-7.53940549437994,0.699383189959228,
7.43378467814468));
#12911=CARTESIAN_POINT('Ctrl Pts',(-7.71522634131278,0.94087103519469,7.445787864934));
#12912=CARTESIAN_POINT('Ctrl Pts',(-7.98526240565962,1.11182427083165,7.45779105172332));
#12913=CARTESIAN_POINT('Ctrl Pts',(-8.27875123560304,1.16744491727782,7.46979423851264));
#12914=CARTESIAN_POINT('Ctrl Pts',(-8.57224006554646,1.22306556372399,7.48179742530196));
#12915=CARTESIAN_POINT('Ctrl Pts',(-8.88610136060128,1.16276985666962,7.49380061209127));
#12916=CARTESIAN_POINT('Ctrl Pts',(-9.13808834820256,1.00235817476246,7.50580379888059));
#12917=CARTESIAN_POINT('Ctrl Pts',(-9.39007533580383,0.841946492855301,
7.51780698566991));
#12918=CARTESIAN_POINT('Ctrl Pts',(-9.57754329642231,0.583102430601164,
7.52981017245923));
#12919=CARTESIAN_POINT('Ctrl Pts',(-9.65136659729239,0.293655596344343,
7.54181335924855));
#12920=CARTESIAN_POINT('Ctrl Pts',(-9.67581103310574,0.197813707970626,
7.545787864934));
#12921=CARTESIAN_POINT('Ctrl Pts',(-9.68822500000015,0.0989100500905238,
7.54976237061946));
#12922=CARTESIAN_POINT('Ctrl Pts',(-9.688225,-1.83564274891523E-12,7.55373687630491));
#12923=CARTESIAN_POINT('Origin',(-8.5,0.,1.8));
#12924=CARTESIAN_POINT('',(-9.688225,-1.26565424807268E-13,7.89626312369518));
#12925=CARTESIAN_POINT('',(-9.688225,-1.86067827812053E-12,7.85373687630491));
#12926=CARTESIAN_POINT('',(-9.688225,-1.45515594291686E-16,1.8));
#12927=CARTESIAN_POINT('Ctrl Pts',(-9.688225,-1.26565424807268E-13,7.89626312369518));
#12928=CARTESIAN_POINT('Ctrl Pts',(-9.68822500000003,0.298712821305967,
7.88425993690586));
#12929=CARTESIAN_POINT('Ctrl Pts',(-9.57054245632592,0.595858078271415,
7.87225675011655));
#12930=CARTESIAN_POINT('Ctrl Pts',(-9.36601586214944,0.813569405232627,
7.86025356332723));
#12931=CARTESIAN_POINT('Ctrl Pts',(-9.16148926797295,1.03128073219384,7.84825037653791));
#12932=CARTESIAN_POINT('Ctrl Pts',(-8.87226522412859,1.16727314847132,7.83624718974859));
#12933=CARTESIAN_POINT('Ctrl Pts',(-8.57413435701463,1.18591009260189,7.82424400295927));
#12934=CARTESIAN_POINT('Ctrl Pts',(-8.27600348990067,1.20454703673247,7.81224081616996));
#12935=CARTESIAN_POINT('Ctrl Pts',(-7.97209482032107,1.10563290540116,7.80023762938064));
#12936=CARTESIAN_POINT('Ctrl Pts',(-7.74204705372073,0.915087963996671,
7.78823444259132));
#12937=CARTESIAN_POINT('Ctrl Pts',(-7.51199928712038,0.724543022592183,
7.776231255802));
#12938=CARTESIAN_POINT('Ctrl Pts',(-7.3582268807964,0.444367128061618,7.76422806901269));
#12939=CARTESIAN_POINT('Ctrl Pts',(-7.32102560975819,0.147979855990452,
7.75222488222337));
#12940=CARTESIAN_POINT('Ctrl Pts',(-7.28382433871998,-0.148407416080715,
7.74022169543405));
#12941=CARTESIAN_POINT('Ctrl Pts',(-7.3635846474463,-0.457895344721805,
7.72821850864473));
#12942=CARTESIAN_POINT('Ctrl Pts',(-7.53940549437873,-0.699383189957566,
7.71621532185541));
#12943=CARTESIAN_POINT('Ctrl Pts',(-7.71522634131115,-0.940871035193328,
7.7042121350661));
#12944=CARTESIAN_POINT('Ctrl Pts',(-7.98526240565768,-1.11182427083075,
7.69220894827678));
#12945=CARTESIAN_POINT('Ctrl Pts',(-8.27875123560101,-1.16744491727744,
7.68020576148746));
#12946=CARTESIAN_POINT('Ctrl Pts',(-8.57224006554432,-1.22306556372412,
7.66820257469814));
#12947=CARTESIAN_POINT('Ctrl Pts',(-8.88610136059924,-1.1627698566703,7.65619938790883));
#12948=CARTESIAN_POINT('Ctrl Pts',(-9.1380883482008,-1.00235817476358,7.64419620111951));
#12949=CARTESIAN_POINT('Ctrl Pts',(-9.39007533580235,-0.841946492856869,
7.63219301433019));
#12950=CARTESIAN_POINT('Ctrl Pts',(-9.57754329642128,-0.583102430603069,
7.62018982754087));
#12951=CARTESIAN_POINT('Ctrl Pts',(-9.65136659729187,-0.293655596346383,
7.60818664075155));
#12952=CARTESIAN_POINT('Ctrl Pts',(-9.6758110331054,-0.19781370797265,7.6042121350661));
#12953=CARTESIAN_POINT('Ctrl Pts',(-9.68822499999999,-0.0989100500925061,
7.60023762938064));
#12954=CARTESIAN_POINT('Ctrl Pts',(-9.688225,-8.47100167788994E-14,7.59626312369518));
#12955=CARTESIAN_POINT('Ctrl Pts',(-9.688225,-1.83564274891523E-12,7.55373687630491));
#12956=CARTESIAN_POINT('Ctrl Pts',(-9.68822499999954,-0.298712821307918,
7.56574006309423));
#12957=CARTESIAN_POINT('Ctrl Pts',(-9.57054245632495,-0.59585807827316,
7.57774324988355));
#12958=CARTESIAN_POINT('Ctrl Pts',(-9.36601586214812,-0.813569405234033,
7.58974643667286));
#12959=CARTESIAN_POINT('Ctrl Pts',(-9.16148926797128,-1.0312807321949,7.60174962346218));
#12960=CARTESIAN_POINT('Ctrl Pts',(-8.87226522412671,-1.16727314847191,
7.6137528102515));
#12961=CARTESIAN_POINT('Ctrl Pts',(-8.57413435701274,-1.18591009260201,
7.62575599704082));
#12962=CARTESIAN_POINT('Ctrl Pts',(-8.27600348989876,-1.20454703673211,
7.63775918383013));
#12963=CARTESIAN_POINT('Ctrl Pts',(-7.97209482031933,-1.10563290540032,
7.64976237061945));
#12964=CARTESIAN_POINT('Ctrl Pts',(-7.7420470537193,-0.915087963995484,
7.66176555740877));
#12965=CARTESIAN_POINT('Ctrl Pts',(-7.51199928711926,-0.724543022590643,
7.67376874419809));
#12966=CARTESIAN_POINT('Ctrl Pts',(-7.35822688079572,-0.444367128059851,
7.6857719309874));
#12967=CARTESIAN_POINT('Ctrl Pts',(-7.32102560975796,-0.147979855988639,
7.69777511777672));
#12968=CARTESIAN_POINT('Ctrl Pts',(-7.28382433872021,0.148407416082574,
7.70977830456604));
#12969=CARTESIAN_POINT('Ctrl Pts',(-7.363584647447,0.457895344723529,7.72178149135536));
#12970=CARTESIAN_POINT('Ctrl Pts',(-7.53940549437978,0.699383189959016,
7.73378467814467));
#12971=CARTESIAN_POINT('Ctrl Pts',(-7.71522634131256,0.940871035194503,
7.74578786493399));
#12972=CARTESIAN_POINT('Ctrl Pts',(-7.98526240565934,1.11182427083152,7.75779105172331));
#12973=CARTESIAN_POINT('Ctrl Pts',(-8.27875123560273,1.16744491727776,7.76979423851263));
#12974=CARTESIAN_POINT('Ctrl Pts',(-8.57224006554613,1.22306556372401,7.78179742530194));
#12975=CARTESIAN_POINT('Ctrl Pts',(-8.88610136060094,1.16276985666973,7.79380061209126));
#12976=CARTESIAN_POINT('Ctrl Pts',(-9.13808834820225,1.00235817476266,7.80580379888058));
#12977=CARTESIAN_POINT('Ctrl Pts',(-9.39007533580356,0.841946492855582,
7.8178069856699));
#12978=CARTESIAN_POINT('Ctrl Pts',(-9.57754329642211,0.583102430601523,
7.82981017245921));
#12979=CARTESIAN_POINT('Ctrl Pts',(-9.65136659729228,0.293655596344744,
7.84181335924853));
#12980=CARTESIAN_POINT('Ctrl Pts',(-9.67581103310571,0.197813707970894,
7.84578786493399));
#12981=CARTESIAN_POINT('Ctrl Pts',(-9.68822500000015,0.0989100500906451,
7.84976237061945));
#12982=CARTESIAN_POINT('Ctrl Pts',(-9.688225,-1.86067827812053E-12,7.85373687630491));
#12983=CARTESIAN_POINT('Origin',(-8.5,0.,1.8));
#12984=CARTESIAN_POINT('',(-9.68879783790665,0.000205673080331772,8.19626312369518));
#12985=CARTESIAN_POINT('',(-9.6886956555678,0.00043025090496092,8.15373687630491));
#12986=CARTESIAN_POINT('',(-9.688225,-1.45515594291686E-16,1.8));
#12987=CARTESIAN_POINT('Ctrl Pts',(-9.688225,-6.7168492989822E-14,8.19626312369518));
#12988=CARTESIAN_POINT('Ctrl Pts',(-9.68822500000002,0.298712821306026,
8.18425993690586));
#12989=CARTESIAN_POINT('Ctrl Pts',(-9.57054245632589,0.595858078271468,
8.17225675011654));
#12990=CARTESIAN_POINT('Ctrl Pts',(-9.36601586214939,0.813569405232671,
8.16025356332723));
#12991=CARTESIAN_POINT('Ctrl Pts',(-9.16148926797289,1.03128073219387,8.14825037653791));
#12992=CARTESIAN_POINT('Ctrl Pts',(-8.87226522412853,1.16727314847133,8.13624718974859));
#12993=CARTESIAN_POINT('Ctrl Pts',(-8.57413435701457,1.1859100926019,8.12424400295927));
#12994=CARTESIAN_POINT('Ctrl Pts',(-8.27600348990061,1.20454703673246,8.11224081616995));
#12995=CARTESIAN_POINT('Ctrl Pts',(-7.97209482032102,1.10563290540113,8.10023762938064));
#12996=CARTESIAN_POINT('Ctrl Pts',(-7.74204705372068,0.915087963996633,
8.08823444259132));
#12997=CARTESIAN_POINT('Ctrl Pts',(-7.51199928712035,0.724543022592134,
8.076231255802));
#12998=CARTESIAN_POINT('Ctrl Pts',(-7.35822688079638,0.444367128061561,
8.06422806901268));
#12999=CARTESIAN_POINT('Ctrl Pts',(-7.32102560975818,0.147979855990393,
8.05222488222337));
#13000=CARTESIAN_POINT('Ctrl Pts',(-7.28382433871999,-0.148407416080776,
8.04022169543405));
#13001=CARTESIAN_POINT('Ctrl Pts',(-7.36358464744632,-0.457895344721862,
8.02821850864473));
#13002=CARTESIAN_POINT('Ctrl Pts',(-7.53940549437876,-0.699383189957614,
8.01621532185541));
#13003=CARTESIAN_POINT('Ctrl Pts',(-7.7152263413112,-0.940871035193367,
8.00421213506609));
#13004=CARTESIAN_POINT('Ctrl Pts',(-7.98526240565774,-1.11182427083078,
7.99220894827678));
#13005=CARTESIAN_POINT('Ctrl Pts',(-8.27875123560106,-1.16744491727745,
7.98020576148746));
#13006=CARTESIAN_POINT('Ctrl Pts',(-8.57224006554439,-1.22306556372412,
7.96820257469814));
#13007=CARTESIAN_POINT('Ctrl Pts',(-8.8861013605993,-1.16276985667028,7.95619938790882));
#13008=CARTESIAN_POINT('Ctrl Pts',(-9.13808834820085,-1.00235817476355,
7.9441962011195));
#13009=CARTESIAN_POINT('Ctrl Pts',(-9.39007533580239,-0.841946492856824,
7.93219301433019));
#13010=CARTESIAN_POINT('Ctrl Pts',(-9.57754329642131,-0.583102430603015,
7.92018982754087));
#13011=CARTESIAN_POINT('Ctrl Pts',(-9.65136659729188,-0.293655596346326,
7.90818664075155));
#13012=CARTESIAN_POINT('Ctrl Pts',(-9.67581103310541,-0.197813707972624,
7.90421213506609));
#13013=CARTESIAN_POINT('Ctrl Pts',(-9.68822499999999,-0.0989100500925142,
7.90023762938064));
#13014=CARTESIAN_POINT('Ctrl Pts',(-9.688225,-1.26565424807268E-13,7.89626312369518));
#13015=CARTESIAN_POINT('Ctrl Pts',(-9.688225,-1.86067827812053E-12,7.85373687630491));
#13016=CARTESIAN_POINT('Ctrl Pts',(-9.68822499999953,-0.298712821307954,
7.86574006309423));
#13017=CARTESIAN_POINT('Ctrl Pts',(-9.57054245632493,-0.595858078273205,
7.87774324988355));
#13018=CARTESIAN_POINT('Ctrl Pts',(-9.36601586214807,-0.813569405234075,
7.88974643667287));
#13019=CARTESIAN_POINT('Ctrl Pts',(-9.16148926797122,-1.03128073219495,
7.90174962346219));
#13020=CARTESIAN_POINT('Ctrl Pts',(-8.87226522412662,-1.16727314847194,
7.9137528102515));
#13021=CARTESIAN_POINT('Ctrl Pts',(-8.57413435701263,-1.18591009260202,
7.92575599704082));
#13022=CARTESIAN_POINT('Ctrl Pts',(-8.27600348989864,-1.20454703673209,
7.93775918383014));
#13023=CARTESIAN_POINT('Ctrl Pts',(-7.97209482031921,-1.10563290540027,
7.94976237061946));
#13024=CARTESIAN_POINT('Ctrl Pts',(-7.74204705371919,-0.915087963995392,
7.96176555740877));
#13025=CARTESIAN_POINT('Ctrl Pts',(-7.51199928711916,-0.724543022590517,
7.97376874419809));
#13026=CARTESIAN_POINT('Ctrl Pts',(-7.35822688079565,-0.444367128059693,
7.98577193098741));
#13027=CARTESIAN_POINT('Ctrl Pts',(-7.32102560975794,-0.147979855988463,
7.99777511777673));
#13028=CARTESIAN_POINT('Ctrl Pts',(-7.28382433872023,0.148407416082766,
8.00977830456605));
#13029=CARTESIAN_POINT('Ctrl Pts',(-7.36358464744707,0.457895344723721,
8.02178149135536));
#13030=CARTESIAN_POINT('Ctrl Pts',(-7.53940549437991,0.699383189959186,
8.03378467814468));
#13031=CARTESIAN_POINT('Ctrl Pts',(-7.71522634131274,0.940871035194651,
8.045787864934));
#13032=CARTESIAN_POINT('Ctrl Pts',(-7.98526240565956,1.11182427083162,8.05779105172332));
#13033=CARTESIAN_POINT('Ctrl Pts',(-8.27875123560298,1.16744491727781,8.06979423851264));
#13034=CARTESIAN_POINT('Ctrl Pts',(-8.57224006554639,1.223065563724,8.08179742530195));
#13035=CARTESIAN_POINT('Ctrl Pts',(-8.8861013606012,1.16276985666964,8.09380061209127));
#13036=CARTESIAN_POINT('Ctrl Pts',(-9.13808834820249,1.00235817476251,8.10580379888059));
#13037=CARTESIAN_POINT('Ctrl Pts',(-9.39007533580377,0.841946492855368,
8.11780698566991));
#13038=CARTESIAN_POINT('Ctrl Pts',(-9.57754329642226,0.583102430601251,
8.12981017245922));
#13039=CARTESIAN_POINT('Ctrl Pts',(-9.65136659729236,0.293655596344441,
8.14181335924854));
#13040=CARTESIAN_POINT('Ctrl Pts',(-9.67581103310573,0.197813707970689,
8.145787864934));
#13041=CARTESIAN_POINT('Ctrl Pts',(-9.68822500000015,0.0989100500905469,
8.14976237061946));
#13042=CARTESIAN_POINT('Ctrl Pts',(-9.688225,-1.85196302737722E-12,8.15373687630491));
#13043=CARTESIAN_POINT('Origin',(-8.5,0.,1.8));
#13044=CARTESIAN_POINT('',(-9.68736610752,0.000385205738155315,8.49626312369518));
#13045=CARTESIAN_POINT('',(-9.68747447047123,0.000180197558070845,8.45373687630491));
#13046=CARTESIAN_POINT('',(-9.688225,-1.45515594291686E-16,1.8));
#13047=CARTESIAN_POINT('Ctrl Pts',(-9.68638374935818,0.000825784751013359,
8.49626312369518));
#13048=CARTESIAN_POINT('Ctrl Pts',(-9.68732027411901,0.157930601934615,
8.48996455641583));
#13049=CARTESIAN_POINT('Ctrl Pts',(-9.65847850514943,0.314731334995638,
8.48366598913647));
#13050=CARTESIAN_POINT('Ctrl Pts',(-9.598408411445,0.458626072499957,8.47736742185712));
#13051=CARTESIAN_POINT('Ctrl Pts',(-9.44669843817874,0.822039302506726,
8.4614600807055));
#13052=CARTESIAN_POINT('Ctrl Pts',(-9.09580176716099,1.10313295059665,8.44555273955388));
#13053=CARTESIAN_POINT('Ctrl Pts',(-8.70773403538356,1.17202275388512,8.42964539840227));
#13054=CARTESIAN_POINT('Ctrl Pts',(-8.31966630360613,1.2409125571736,8.41373805725065));
#13055=CARTESIAN_POINT('Ctrl Pts',(-7.89442751106905,1.09759851566063,8.39783071609902));
#13056=CARTESIAN_POINT('Ctrl Pts',(-7.62673268623578,0.808436475509857,
8.3819233749474));
#13057=CARTESIAN_POINT('Ctrl Pts',(-7.3590378614025,0.519274435359075,8.36601603379578));
#13058=CARTESIAN_POINT('Ctrl Pts',(-7.24888700427306,0.0842643965704531,
8.35010869264415));
#13059=CARTESIAN_POINT('Ctrl Pts',(-7.34744850505387,-0.297347972212119,
8.33420135149253));
#13060=CARTESIAN_POINT('Ctrl Pts',(-7.44601000583468,-0.67896034099468,
8.31829401034092));
#13061=CARTESIAN_POINT('Ctrl Pts',(-7.75328386452571,-1.00717503977121,
8.3023866691893));
#13062=CARTESIAN_POINT('Ctrl Pts',(-8.12729821016773,-1.13045667257339,
8.28647932803768));
#13063=CARTESIAN_POINT('Ctrl Pts',(-8.50131255580976,-1.25373830537556,
8.27057198688606));
#13064=CARTESIAN_POINT('Ctrl Pts',(-8.94206738840278,-1.17208687220337,
8.25466464573443));
#13065=CARTESIAN_POINT('Ctrl Pts',(-9.24895983130622,-0.924420172686451,
8.23875730458281));
#13066=CARTESIAN_POINT('Ctrl Pts',(-9.40240605275795,-0.800586822927992,
8.230803634007));
#13067=CARTESIAN_POINT('Ctrl Pts',(-9.52238667678728,-0.635249656583355,
8.22284996343119));
#13068=CARTESIAN_POINT('Ctrl Pts',(-9.5979190957647,-0.4516287327225,8.21489629285538));
#13069=CARTESIAN_POINT('Ctrl Pts',(-9.65690269444705,-0.308238344471755,
8.20868523646865));
#13070=CARTESIAN_POINT('Ctrl Pts',(-9.68878125811642,-0.153698307161689,
8.20247418008191));
#13071=CARTESIAN_POINT('Ctrl Pts',(-9.6894905109208,0.000454372041894774,
8.19626312369518));
#13072=CARTESIAN_POINT('Ctrl Pts',(-9.68916921325107,0.000863154794381365,
8.15373687630491));
#13073=CARTESIAN_POINT('Ctrl Pts',(-9.68644568297345,-0.338450824757492,
8.16740829852045));
#13074=CARTESIAN_POINT('Ctrl Pts',(-9.53412983057639,-0.679944095139565,
8.181079720736));
#13075=CARTESIAN_POINT('Ctrl Pts',(-9.27761323455168,-0.901170584590548,
8.19475114295154));
#13076=CARTESIAN_POINT('Ctrl Pts',(-8.97914414043077,-1.15857798405419,
8.21065848410316));
#13077=CARTESIAN_POINT('Ctrl Pts',(-8.53960376307625,-1.25316323344806,
8.22656582525477));
#13078=CARTESIAN_POINT('Ctrl Pts',(-8.16201220914371,-1.14131641797617,
8.24247316640639));
#13079=CARTESIAN_POINT('Ctrl Pts',(-7.78442065521116,-1.02946960250427,
8.25838050755802));
#13080=CARTESIAN_POINT('Ctrl Pts',(-7.46877792470057,-0.711190722166612,
8.27428784870964));
#13081=CARTESIAN_POINT('Ctrl Pts',(-7.35774362943076,-0.332782013447075,
8.29019518986126));
#13082=CARTESIAN_POINT('Ctrl Pts',(-7.30222648179586,-0.143577659087295,
8.29814886043707));
#13083=CARTESIAN_POINT('Ctrl Pts',(-7.29786144297115,0.060659152367949,
8.30610253101288));
#13084=CARTESIAN_POINT('Ctrl Pts',(-7.3404400790801,0.254589164854932,8.31405620158869));
#13085=CARTESIAN_POINT('Ctrl Pts',(-7.38301871518904,0.448519177341904,
8.3220098721645));
#13086=CARTESIAN_POINT('Ctrl Pts',(-7.47254102623163,0.632142390860607,
8.32996354274031));
#13087=CARTESIAN_POINT('Ctrl Pts',(-7.60221326400362,0.780687172463381,
8.33791721331612));
#13088=CARTESIAN_POINT('Ctrl Pts',(-7.86155773954761,1.07777673566892,8.35382455446774));
#13089=CARTESIAN_POINT('Ctrl Pts',(-8.28150192200923,1.23455257121074,8.36973189561937));
#13090=CARTESIAN_POINT('Ctrl Pts',(-8.67121870081464,1.17793169122883,8.38563923677099));
#13091=CARTESIAN_POINT('Ctrl Pts',(-9.06093547962008,1.12131081124692,8.40154657792261));
#13092=CARTESIAN_POINT('Ctrl Pts',(-9.42042485476932,0.851293215741264,
8.41745391907422));
#13093=CARTESIAN_POINT('Ctrl Pts',(-9.58360884738056,0.492526781972071,
8.43336126022584));
#13094=CARTESIAN_POINT('Ctrl Pts',(-9.65328264037972,0.339346204382988,
8.4401531322522));
#13095=CARTESIAN_POINT('Ctrl Pts',(-9.68717019866577,0.169986820509775,
8.44694500427855));
#13096=CARTESIAN_POINT('Ctrl Pts',(-9.68650724062112,0.000412423542754418,
8.45373687630491));
#13097=CARTESIAN_POINT('Origin',(-8.5,0.,1.8));
#13098=CARTESIAN_POINT('',(-9.688225,-4.9737991503207E-14,8.79626312369518));
#13099=CARTESIAN_POINT('',(-9.688225,-1.80067072363954E-12,8.75373687630491));
#13100=CARTESIAN_POINT('',(-9.688225,-1.45515594291686E-16,1.8));
#13101=CARTESIAN_POINT('Ctrl Pts',(-9.688225,-1.58761892521397E-14,8.79626312369518));
#13102=CARTESIAN_POINT('Ctrl Pts',(-9.688225,0.298712821306078,8.78425993690586));
#13103=CARTESIAN_POINT('Ctrl Pts',(-9.57054245632587,0.595858078271514,
8.77225675011654));
#13104=CARTESIAN_POINT('Ctrl Pts',(-9.36601586214936,0.813569405232708,
8.76025356332722));
#13105=CARTESIAN_POINT('Ctrl Pts',(-9.16148926797285,1.0312807321939,8.74825037653791));
#13106=CARTESIAN_POINT('Ctrl Pts',(-8.87226522412848,1.16727314847135,8.73624718974859));
#13107=CARTESIAN_POINT('Ctrl Pts',(-8.57413435701452,1.1859100926019,8.72424400295927));
#13108=CARTESIAN_POINT('Ctrl Pts',(-8.27600348990056,1.20454703673245,8.71224081616995));
#13109=CARTESIAN_POINT('Ctrl Pts',(-7.97209482032097,1.10563290540111,8.70023762938063));
#13110=CARTESIAN_POINT('Ctrl Pts',(-7.74204705372064,0.9150879639966,8.68823444259132));
#13111=CARTESIAN_POINT('Ctrl Pts',(-7.51199928712032,0.724543022592091,
8.676231255802));
#13112=CARTESIAN_POINT('Ctrl Pts',(-7.35822688079636,0.444367128061512,
8.66422806901268));
#13113=CARTESIAN_POINT('Ctrl Pts',(-7.32102560975818,0.147979855990342,
8.65222488222336));
#13114=CARTESIAN_POINT('Ctrl Pts',(-7.28382433871999,-0.148407416080828,
8.64022169543404));
#13115=CARTESIAN_POINT('Ctrl Pts',(-7.36358464744634,-0.45789534472191,
8.62821850864473));
#13116=CARTESIAN_POINT('Ctrl Pts',(-7.53940549437879,-0.699383189957656,
8.61621532185541));
#13117=CARTESIAN_POINT('Ctrl Pts',(-7.71522634131124,-0.940871035193401,
8.60421213506609));
#13118=CARTESIAN_POINT('Ctrl Pts',(-7.98526240565779,-1.1118242708308,8.59220894827677));
#13119=CARTESIAN_POINT('Ctrl Pts',(-8.27875123560111,-1.16744491727746,
8.58020576148746));
#13120=CARTESIAN_POINT('Ctrl Pts',(-8.57224006554444,-1.22306556372411,
8.56820257469814));
#13121=CARTESIAN_POINT('Ctrl Pts',(-8.88610136059935,-1.16276985667026,
8.55619938790882));
#13122=CARTESIAN_POINT('Ctrl Pts',(-9.13808834820089,-1.00235817476352,
8.5441962011195));
#13123=CARTESIAN_POINT('Ctrl Pts',(-9.39007533580243,-0.841946492856786,
8.53219301433018));
#13124=CARTESIAN_POINT('Ctrl Pts',(-9.57754329642134,-0.583102430602969,
8.52018982754087));
#13125=CARTESIAN_POINT('Ctrl Pts',(-9.65136659729189,-0.293655596346276,
8.50818664075155));
#13126=CARTESIAN_POINT('Ctrl Pts',(-9.67581103310542,-0.197813707972562,
8.50421213506609));
#13127=CARTESIAN_POINT('Ctrl Pts',(-9.688225,-0.0989100500924404,8.50023762938064));
#13128=CARTESIAN_POINT('Ctrl Pts',(-9.688225,-4.15223411209809E-14,8.49626312369518));
#13129=CARTESIAN_POINT('Ctrl Pts',(-9.688225,-1.82637238665961E-12,8.45373687630491));
#13130=CARTESIAN_POINT('Ctrl Pts',(-9.68822499999954,-0.298712821307931,
8.46574006309423));
#13131=CARTESIAN_POINT('Ctrl Pts',(-9.57054245632493,-0.595858078273196,
8.47774324988355));
#13132=CARTESIAN_POINT('Ctrl Pts',(-9.36601586214807,-0.813569405234075,
8.48974643667287));
#13133=CARTESIAN_POINT('Ctrl Pts',(-9.16148926797121,-1.03128073219495,
8.50174962346219));
#13134=CARTESIAN_POINT('Ctrl Pts',(-8.87226522412661,-1.16727314847195,
8.5137528102515));
#13135=CARTESIAN_POINT('Ctrl Pts',(-8.57413435701261,-1.18591009260202,
8.52575599704082));
#13136=CARTESIAN_POINT('Ctrl Pts',(-8.27600348989861,-1.20454703673209,
8.53775918383014));
#13137=CARTESIAN_POINT('Ctrl Pts',(-7.97209482031917,-1.10563290540025,
8.54976237061946));
#13138=CARTESIAN_POINT('Ctrl Pts',(-7.74204705371915,-0.91508796399536,
8.56176555740878));
#13139=CARTESIAN_POINT('Ctrl Pts',(-7.51199928711912,-0.724543022590468,
8.57376874419809));
#13140=CARTESIAN_POINT('Ctrl Pts',(-7.35822688079562,-0.444367128059623,
8.58577193098741));
#13141=CARTESIAN_POINT('Ctrl Pts',(-7.32102560975793,-0.14797985598838,
8.59777511777673));
#13142=CARTESIAN_POINT('Ctrl Pts',(-7.28382433872024,0.148407416082863,
8.60977830456605));
#13143=CARTESIAN_POINT('Ctrl Pts',(-7.36358464744711,0.457895344723825,
8.62178149135537));
#13144=CARTESIAN_POINT('Ctrl Pts',(-7.53940549437997,0.699383189959281,
8.63378467814469));
#13145=CARTESIAN_POINT('Ctrl Pts',(-7.71522634131284,0.940871035194738,
8.64578786493401));
#13146=CARTESIAN_POINT('Ctrl Pts',(-7.98526240565969,1.11182427083168,8.65779105172332));
#13147=CARTESIAN_POINT('Ctrl Pts',(-8.27875123560312,1.16744491727784,8.66979423851264));
#13148=CARTESIAN_POINT('Ctrl Pts',(-8.57224006554655,1.22306556372399,8.68179742530196));
#13149=CARTESIAN_POINT('Ctrl Pts',(-8.88610136060138,1.16276985666959,8.69380061209128));
#13150=CARTESIAN_POINT('Ctrl Pts',(-9.13808834820264,1.00235817476241,8.7058037988806));
#13151=CARTESIAN_POINT('Ctrl Pts',(-9.39007533580391,0.841946492855223,
8.71780698566991));
#13152=CARTESIAN_POINT('Ctrl Pts',(-9.57754329642237,0.583102430601064,
8.72981017245923));
#13153=CARTESIAN_POINT('Ctrl Pts',(-9.65136659729242,0.293655596344229,
8.74181335924855));
#13154=CARTESIAN_POINT('Ctrl Pts',(-9.67581103310575,0.197813707970559,
8.745787864934));
#13155=CARTESIAN_POINT('Ctrl Pts',(-9.68822500000015,0.0989100500905081,
8.74976237061946));
#13156=CARTESIAN_POINT('Ctrl Pts',(-9.688225,-1.80067072363954E-12,8.75373687630491));
#13157=CARTESIAN_POINT('Origin',(-8.5,0.,1.8));
#13158=CARTESIAN_POINT('',(-9.688225,-2.40918396343659E-14,9.09626312369518));
#13159=CARTESIAN_POINT('',(-9.688225,-1.77513559407316E-12,9.05373687630491));
#13160=CARTESIAN_POINT('',(-9.688225,-1.45515594291686E-16,1.8));
#13161=CARTESIAN_POINT('Ctrl Pts',(-9.688225,9.54791801177635E-15,9.09626312369518));
#13162=CARTESIAN_POINT('Ctrl Pts',(-9.688225,0.298712821306092,9.08425993690586));
#13163=CARTESIAN_POINT('Ctrl Pts',(-9.57054245632587,0.595858078271515,
9.07225675011654));
#13164=CARTESIAN_POINT('Ctrl Pts',(-9.36601586214937,0.813569405232702,
9.06025356332722));
#13165=CARTESIAN_POINT('Ctrl Pts',(-9.16148926797287,1.03128073219389,9.04825037653791));
#13166=CARTESIAN_POINT('Ctrl Pts',(-8.87226522412851,1.16727314847134,9.03624718974859));
#13167=CARTESIAN_POINT('Ctrl Pts',(-8.57413435701456,1.1859100926019,9.02424400295927));
#13168=CARTESIAN_POINT('Ctrl Pts',(-8.27600348990061,1.20454703673245,9.01224081616995));
#13169=CARTESIAN_POINT('Ctrl Pts',(-7.97209482032103,1.10563290540114,9.00023762938064));
#13170=CARTESIAN_POINT('Ctrl Pts',(-7.7420470537207,0.915087963996648,8.98823444259132));
#13171=CARTESIAN_POINT('Ctrl Pts',(-7.51199928712037,0.724543022592161,
8.976231255802));
#13172=CARTESIAN_POINT('Ctrl Pts',(-7.3582268807964,0.444367128061606,8.96422806901269));
#13173=CARTESIAN_POINT('Ctrl Pts',(-7.32102560975819,0.147979855990451,
8.95222488222337));
#13174=CARTESIAN_POINT('Ctrl Pts',(-7.28382433871998,-0.148407416080705,
8.94022169543405));
#13175=CARTESIAN_POINT('Ctrl Pts',(-7.3635846474463,-0.457895344721783,
8.92821850864473));
#13176=CARTESIAN_POINT('Ctrl Pts',(-7.53940549437871,-0.69938318995754,
8.91621532185541));
#13177=CARTESIAN_POINT('Ctrl Pts',(-7.71522634131112,-0.940871035193297,
8.9042121350661));
#13178=CARTESIAN_POINT('Ctrl Pts',(-7.98526240565763,-1.11182427083073,
8.89220894827678));
#13179=CARTESIAN_POINT('Ctrl Pts',(-8.27875123560094,-1.16744491727742,
8.88020576148746));
#13180=CARTESIAN_POINT('Ctrl Pts',(-8.57224006554425,-1.22306556372412,
8.86820257469815));
#13181=CARTESIAN_POINT('Ctrl Pts',(-8.88610136059915,-1.16276985667032,
8.85619938790883));
#13182=CARTESIAN_POINT('Ctrl Pts',(-9.13808834820071,-1.00235817476364,
8.84419620111951));
#13183=CARTESIAN_POINT('Ctrl Pts',(-9.39007533580227,-0.84194649285695,
8.83219301433019));
#13184=CARTESIAN_POINT('Ctrl Pts',(-9.57754329642122,-0.583102430603179,
8.82018982754088));
#13185=CARTESIAN_POINT('Ctrl Pts',(-9.65136659729183,-0.293655596346513,
8.80818664075156));
#13186=CARTESIAN_POINT('Ctrl Pts',(-9.6758110331054,-0.197813707972717,
8.8042121350661));
#13187=CARTESIAN_POINT('Ctrl Pts',(-9.688225,-0.0989100500925048,8.80023762938064));
#13188=CARTESIAN_POINT('Ctrl Pts',(-9.688225,-1.58761892521397E-14,8.79626312369518));
#13189=CARTESIAN_POINT('Ctrl Pts',(-9.688225,-1.80067072363954E-12,8.75373687630491));
#13190=CARTESIAN_POINT('Ctrl Pts',(-9.68822499999955,-0.298712821307894,
8.76574006309423));
#13191=CARTESIAN_POINT('Ctrl Pts',(-9.57054245632496,-0.595858078273151,
8.77774324988355));
#13192=CARTESIAN_POINT('Ctrl Pts',(-9.36601586214812,-0.813569405234032,
8.78974643667286));
#13193=CARTESIAN_POINT('Ctrl Pts',(-9.16148926797127,-1.03128073219491,
8.80174962346218));
#13194=CARTESIAN_POINT('Ctrl Pts',(-8.87226522412669,-1.16727314847192,
8.8137528102515));
#13195=CARTESIAN_POINT('Ctrl Pts',(-8.57413435701271,-1.18591009260201,
8.82575599704082));
#13196=CARTESIAN_POINT('Ctrl Pts',(-8.27600348989872,-1.2045470367321,8.83775918383014));
#13197=CARTESIAN_POINT('Ctrl Pts',(-7.97209482031928,-1.1056329054003,8.84976237061945));
#13198=CARTESIAN_POINT('Ctrl Pts',(-7.74204705371924,-0.915087963995441,
8.86176555740877));
#13199=CARTESIAN_POINT('Ctrl Pts',(-7.51199928711921,-0.724543022590581,
8.87376874419809));
#13200=CARTESIAN_POINT('Ctrl Pts',(-7.35822688079568,-0.444367128059766,
8.88577193098741));
#13201=CARTESIAN_POINT('Ctrl Pts',(-7.32102560975795,-0.147979855988539,
8.89777511777672));
#13202=CARTESIAN_POINT('Ctrl Pts',(-7.28382433872022,0.148407416082687,
8.90977830456604));
#13203=CARTESIAN_POINT('Ctrl Pts',(-7.36358464744704,0.457895344723648,
8.92178149135536));
#13204=CARTESIAN_POINT('Ctrl Pts',(-7.53940549437986,0.699383189959124,
8.93378467814468));
#13205=CARTESIAN_POINT('Ctrl Pts',(-7.71522634131268,0.9408710351946,8.945787864934));
#13206=CARTESIAN_POINT('Ctrl Pts',(-7.98526240565949,1.11182427083159,8.95779105172331));
#13207=CARTESIAN_POINT('Ctrl Pts',(-8.2787512356029,1.16744491727779,8.96979423851263));
#13208=CARTESIAN_POINT('Ctrl Pts',(-8.57224006554631,1.223065563724,8.98179742530195));
#13209=CARTESIAN_POINT('Ctrl Pts',(-8.88610136060113,1.16276985666967,8.99380061209127));
#13210=CARTESIAN_POINT('Ctrl Pts',(-9.13808834820242,1.00235817476255,9.00580379888059));
#13211=CARTESIAN_POINT('Ctrl Pts',(-9.39007533580372,0.841946492855425,
9.01780698566991));
#13212=CARTESIAN_POINT('Ctrl Pts',(-9.57754329642223,0.583102430601321,
9.02981017245922));
#13213=CARTESIAN_POINT('Ctrl Pts',(-9.65136659729234,0.293655596344516,
9.04181335924854));
#13214=CARTESIAN_POINT('Ctrl Pts',(-9.67581103310572,0.197813707970765,
9.045787864934));
#13215=CARTESIAN_POINT('Ctrl Pts',(-9.68822500000015,0.0989100500906238,
9.04976237061945));
#13216=CARTESIAN_POINT('Ctrl Pts',(-9.688225,-1.77513559407316E-12,9.05373687630491));
#13217=CARTESIAN_POINT('Origin',(-8.5,0.,1.8));
#13218=CARTESIAN_POINT('',(-9.68802305040078,0.000608274356598134,9.39626312369518));
#13219=CARTESIAN_POINT('',(-9.688225,-1.74948944220432E-12,9.35373687630491));
#13220=CARTESIAN_POINT('',(-9.688225,-1.45515594291686E-16,1.8));
#13221=CARTESIAN_POINT('Ctrl Pts',(-9.688225,3.530509218308E-14,9.39626312369518));
#13222=CARTESIAN_POINT('Ctrl Pts',(-9.68822499999999,0.298712821306129,
9.38425993690586));
#13223=CARTESIAN_POINT('Ctrl Pts',(-9.57054245632584,0.595858078271561,
9.37225675011654));
#13224=CARTESIAN_POINT('Ctrl Pts',(-9.36601586214933,0.813569405232745,
9.36025356332722));
#13225=CARTESIAN_POINT('Ctrl Pts',(-9.16148926797281,1.03128073219393,9.3482503765379));
#13226=CARTESIAN_POINT('Ctrl Pts',(-8.87226522412843,1.16727314847137,9.33624718974859));
#13227=CARTESIAN_POINT('Ctrl Pts',(-8.57413435701447,1.1859100926019,9.32424400295927));
#13228=CARTESIAN_POINT('Ctrl Pts',(-8.27600348990051,1.20454703673244,9.31224081616995));
#13229=CARTESIAN_POINT('Ctrl Pts',(-7.97209482032092,1.10563290540109,9.30023762938063));
#13230=CARTESIAN_POINT('Ctrl Pts',(-7.7420470537206,0.915087963996567,9.28823444259131));
#13231=CARTESIAN_POINT('Ctrl Pts',(-7.51199928712029,0.724543022592049,
9.276231255802));
#13232=CARTESIAN_POINT('Ctrl Pts',(-7.35822688079634,0.444367128061463,
9.26422806901268));
#13233=CARTESIAN_POINT('Ctrl Pts',(-7.32102560975817,0.147979855990291,
9.25222488222336));
#13234=CARTESIAN_POINT('Ctrl Pts',(-7.28382433872,-0.148407416080881,9.24022169543404));
#13235=CARTESIAN_POINT('Ctrl Pts',(-7.36358464744636,-0.457895344721959,
9.22821850864473));
#13236=CARTESIAN_POINT('Ctrl Pts',(-7.53940549437882,-0.699383189957697,
9.21621532185541));
#13237=CARTESIAN_POINT('Ctrl Pts',(-7.71522634131128,-0.940871035193435,
9.20421213506609));
#13238=CARTESIAN_POINT('Ctrl Pts',(-7.98526240565783,-1.11182427083082,
9.19220894827677));
#13239=CARTESIAN_POINT('Ctrl Pts',(-8.27875123560116,-1.16744491727747,
9.18020576148745));
#13240=CARTESIAN_POINT('Ctrl Pts',(-8.57224006554449,-1.22306556372411,
9.16820257469814));
#13241=CARTESIAN_POINT('Ctrl Pts',(-8.8861013605994,-1.16276985667024,9.15619938790882));
#13242=CARTESIAN_POINT('Ctrl Pts',(-9.13808834820093,-1.0023581747635,9.1441962011195));
#13243=CARTESIAN_POINT('Ctrl Pts',(-9.39007533580246,-0.841946492856748,
9.13219301433018));
#13244=CARTESIAN_POINT('Ctrl Pts',(-9.57754329642136,-0.583102430602922,
9.12018982754086));
#13245=CARTESIAN_POINT('Ctrl Pts',(-9.65136659729191,-0.293655596346227,
9.10818664075155));
#13246=CARTESIAN_POINT('Ctrl Pts',(-9.67581103310543,-0.197813707972512,
9.10421213506609));
#13247=CARTESIAN_POINT('Ctrl Pts',(-9.688225,-0.0989100500923894,9.10023762938063));
#13248=CARTESIAN_POINT('Ctrl Pts',(-9.688225,9.54791801177635E-15,9.09626312369518));
#13249=CARTESIAN_POINT('Ctrl Pts',(-9.688225,-1.77513559407316E-12,9.05373687630491));
#13250=CARTESIAN_POINT('Ctrl Pts',(-9.68822499999955,-0.298712821307869,
9.06574006309423));
#13251=CARTESIAN_POINT('Ctrl Pts',(-9.57054245632497,-0.595858078273128,
9.07774324988354));
#13252=CARTESIAN_POINT('Ctrl Pts',(-9.36601586214813,-0.813569405234013,
9.08974643667286));
#13253=CARTESIAN_POINT('Ctrl Pts',(-9.1614892679713,-1.0312807321949,9.10174962346218));
#13254=CARTESIAN_POINT('Ctrl Pts',(-8.87226522412672,-1.16727314847191,
9.1137528102515));
#13255=CARTESIAN_POINT('Ctrl Pts',(-8.57413435701273,-1.18591009260201,
9.12575599704082));
#13256=CARTESIAN_POINT('Ctrl Pts',(-8.27600348989875,-1.20454703673211,
9.13775918383014));
#13257=CARTESIAN_POINT('Ctrl Pts',(-7.9720948203193,-1.10563290540031,9.14976237061945));
#13258=CARTESIAN_POINT('Ctrl Pts',(-7.74204705371926,-0.915087963995458,
9.16176555740877));
#13259=CARTESIAN_POINT('Ctrl Pts',(-7.51199928711922,-0.724543022590602,
9.17376874419809));
#13260=CARTESIAN_POINT('Ctrl Pts',(-7.35822688079569,-0.444367128059791,
9.18577193098741));
#13261=CARTESIAN_POINT('Ctrl Pts',(-7.32102560975795,-0.147979855988565,
9.19777511777673));
#13262=CARTESIAN_POINT('Ctrl Pts',(-7.28382433872022,0.148407416082661,
9.20977830456604));
#13263=CARTESIAN_POINT('Ctrl Pts',(-7.36358464744704,0.457895344723623,
9.22178149135536));
#13264=CARTESIAN_POINT('Ctrl Pts',(-7.53940549437985,0.699383189959103,
9.23378467814468));
#13265=CARTESIAN_POINT('Ctrl Pts',(-7.71522634131266,0.940871035194583,
9.245787864934));
#13266=CARTESIAN_POINT('Ctrl Pts',(-7.98526240565946,1.11182427083158,9.25779105172331));
#13267=CARTESIAN_POINT('Ctrl Pts',(-8.27875123560287,1.16744491727779,9.26979423851263));
#13268=CARTESIAN_POINT('Ctrl Pts',(-8.57224006554628,1.223065563724,9.28179742530195));
#13269=CARTESIAN_POINT('Ctrl Pts',(-8.8861013606011,1.16276985666968,9.29380061209127));
#13270=CARTESIAN_POINT('Ctrl Pts',(-9.1380883482024,1.00235817476256,9.30580379888059));
#13271=CARTESIAN_POINT('Ctrl Pts',(-9.3900753358037,0.841946492855444,9.3178069856699));
#13272=CARTESIAN_POINT('Ctrl Pts',(-9.57754329642221,0.583102430601344,
9.32981017245922));
#13273=CARTESIAN_POINT('Ctrl Pts',(-9.65136659729234,0.293655596344541,
9.34181335924854));
#13274=CARTESIAN_POINT('Ctrl Pts',(-9.67581103310571,0.197813707970801,
9.34578786493399));
#13275=CARTESIAN_POINT('Ctrl Pts',(-9.68822500000014,0.0989100500906719,
9.34976237061945));
#13276=CARTESIAN_POINT('Ctrl Pts',(-9.688225,-1.71568315110449E-12,9.35373687630491));
#13277=CARTESIAN_POINT('Origin',(-8.5,0.,1.8));
#13278=CARTESIAN_POINT('',(-9.68728951167887,-0.000140790589323958,9.69626312369518));
#13279=CARTESIAN_POINT('',(-9.688225,-1.72389880148671E-12,9.65373687630491));
#13280=CARTESIAN_POINT('',(-9.688225,-1.45515594291686E-16,1.8));
#13281=CARTESIAN_POINT('Ctrl Pts',(-9.68633624213298,-0.000284257245408481,
9.69626312369518));
#13282=CARTESIAN_POINT('Ctrl Pts',(-9.68599772448992,0.214868365865776,
9.68764808520634));
#13283=CARTESIAN_POINT('Ctrl Pts',(-9.63021606168018,0.430233739330785,
9.67903304671751));
#13284=CARTESIAN_POINT('Ctrl Pts',(-9.52020978820705,0.613158016442515,
9.67041800822868));
#13285=CARTESIAN_POINT('Ctrl Pts',(-9.31708738507166,0.950920742018469,
9.65451066707706));
#13286=CARTESIAN_POINT('Ctrl Pts',(-8.92909040695752,1.17807808330892,9.63860332592544));
#13287=CARTESIAN_POINT('Ctrl Pts',(-8.5354559263329,1.18978224478168,9.62269598477382));
#13288=CARTESIAN_POINT('Ctrl Pts',(-8.14182144570827,1.20148640625444,9.6067886436222));
#13289=CARTESIAN_POINT('Ctrl Pts',(-7.74254946257315,0.997737387909526,
9.59088130247057));
#13290=CARTESIAN_POINT('Ctrl Pts',(-7.5188628313805,0.672951217350277,9.57497396131895));
#13291=CARTESIAN_POINT('Ctrl Pts',(-7.40701951578419,0.510558132070666,
9.56702029074314));
#13292=CARTESIAN_POINT('Ctrl Pts',(-7.3390725381735,0.317905758737486,9.55906662016734));
#13293=CARTESIAN_POINT('Ctrl Pts',(-7.31893965943283,0.120379919441194,
9.55111294959153));
#13294=CARTESIAN_POINT('Ctrl Pts',(-7.29880678069217,-0.0771459198551094,
9.54315927901572));
#13295=CARTESIAN_POINT('Ctrl Pts',(-7.32648800082156,-0.279545225114548,
9.5352056084399));
#13296=CARTESIAN_POINT('Ctrl Pts',(-7.40326782979251,-0.461163779379811,
9.52725193786409));
#13297=CARTESIAN_POINT('Ctrl Pts',(-7.55682748773441,-0.824400887910347,
9.51134459671246));
#13298=CARTESIAN_POINT('Ctrl Pts',(-7.90678158104258,-1.10451499246429,
9.49543725556086));
#13299=CARTESIAN_POINT('Ctrl Pts',(-8.29468277135129,-1.1724690820358,9.47952991440923));
#13300=CARTESIAN_POINT('Ctrl Pts',(-8.68258396166,-1.24042317160732,9.46362257325761));
#13301=CARTESIAN_POINT('Ctrl Pts',(-9.10843224896924,-1.09621724619641,
9.44771523210598));
#13302=CARTESIAN_POINT('Ctrl Pts',(-9.37552284820049,-0.806381117933753,
9.43180789095436));
#13303=CARTESIAN_POINT('Ctrl Pts',(-9.57445978547795,-0.590502641361061,
9.4199596352013));
#13304=CARTESIAN_POINT('Ctrl Pts',(-9.68532258180007,-0.293832770251182,
9.40811137944824));
#13305=CARTESIAN_POINT('Ctrl Pts',(-9.68786906204226,0.0010720889423268,
9.39626312369517));
#13306=CARTESIAN_POINT('Ctrl Pts',(-9.688225,-1.71568315110449E-12,9.35373687630491));
#13307=CARTESIAN_POINT('Ctrl Pts',(-9.68822499999957,-0.298712821307787,
9.36574006309422));
#13308=CARTESIAN_POINT('Ctrl Pts',(-9.57054245632502,-0.59585807827303,
9.37774324988354));
#13309=CARTESIAN_POINT('Ctrl Pts',(-9.36601586214822,-0.813569405233921,
9.38974643667286));
#13310=CARTESIAN_POINT('Ctrl Pts',(-9.16148926797142,-1.03128073219481,
9.40174962346217));
#13311=CARTESIAN_POINT('Ctrl Pts',(-8.87226522412689,-1.16727314847185,
9.41375281025149));
#13312=CARTESIAN_POINT('Ctrl Pts',(-8.57413435701293,-1.185910092602,9.42575599704081));
#13313=CARTESIAN_POINT('Ctrl Pts',(-8.27600348989897,-1.20454703673214,
9.43775918383013));
#13314=CARTESIAN_POINT('Ctrl Pts',(-7.97209482031953,-1.10563290540042,
9.44976237061944));
#13315=CARTESIAN_POINT('Ctrl Pts',(-7.74204705371947,-0.915087963995625,
9.46176555740876));
#13316=CARTESIAN_POINT('Ctrl Pts',(-7.5119992871194,-0.724543022590834,
9.47376874419808));
#13317=CARTESIAN_POINT('Ctrl Pts',(-7.35822688079581,-0.444367128060085,
9.4857719309874));
#13318=CARTESIAN_POINT('Ctrl Pts',(-7.321025609758,-0.147979855988892,9.49777511777671));
#13319=CARTESIAN_POINT('Ctrl Pts',(-7.28382433872018,0.148407416082302,
9.50977830456603));
#13320=CARTESIAN_POINT('Ctrl Pts',(-7.3635846474469,0.457895344723262,9.52178149135535));
#13321=CARTESIAN_POINT('Ctrl Pts',(-7.53940549437961,0.699383189958782,
9.53378467814466));
#13322=CARTESIAN_POINT('Ctrl Pts',(-7.71522634131233,0.940871035194303,
9.54578786493398));
#13323=CARTESIAN_POINT('Ctrl Pts',(-7.98526240565905,1.11182427083138,9.5577910517233));
#13324=CARTESIAN_POINT('Ctrl Pts',(-8.27875123560242,1.1674449172777,9.56979423851261));
#13325=CARTESIAN_POINT('Ctrl Pts',(-8.57224006554578,1.22306556372403,9.58179742530193));
#13326=CARTESIAN_POINT('Ctrl Pts',(-8.8861013606006,1.16276985666984,9.59380061209125));
#13327=CARTESIAN_POINT('Ctrl Pts',(-9.13808834820195,1.00235817476285,9.60580379888056));
#13328=CARTESIAN_POINT('Ctrl Pts',(-9.3900753358033,0.841946492855855,9.61780698566988));
#13329=CARTESIAN_POINT('Ctrl Pts',(-9.57754329642193,0.583102430601866,
9.6298101724592));
#13330=CARTESIAN_POINT('Ctrl Pts',(-9.65136659729219,0.293655596345122,
9.64181335924851));
#13331=CARTESIAN_POINT('Ctrl Pts',(-9.67581103310566,0.197813707971209,
9.64578786493398));
#13332=CARTESIAN_POINT('Ctrl Pts',(-9.68822500000014,0.0989100500908889,
9.64976237061944));
#13333=CARTESIAN_POINT('Ctrl Pts',(-9.688225,-1.69009251038688E-12,9.65373687630491));
#13334=CARTESIAN_POINT('Origin',(-8.5,0.,1.8));
#13335=CARTESIAN_POINT('',(-9.688225,5.27355936696949E-14,9.99626312369517));
#13336=CARTESIAN_POINT('',(-9.688225,-1.69825264961787E-12,9.95373687630491));
#13337=CARTESIAN_POINT('',(-9.688225,-1.45515594291686E-16,1.8));
#13338=CARTESIAN_POINT('Ctrl Pts',(-9.688225,8.65973959207622E-14,9.99626312369517));
#13339=CARTESIAN_POINT('Ctrl Pts',(-9.68822499999998,0.29871282130618,9.98425993690586));
#13340=CARTESIAN_POINT('Ctrl Pts',(-9.57054245632582,0.595858078271607,
9.97225675011654));
#13341=CARTESIAN_POINT('Ctrl Pts',(-9.36601586214929,0.813569405232783,
9.96025356332722));
#13342=CARTESIAN_POINT('Ctrl Pts',(-9.16148926797276,1.03128073219396,9.9482503765379));
#13343=CARTESIAN_POINT('Ctrl Pts',(-8.87226522412838,1.16727314847138,9.93624718974858));
#13344=CARTESIAN_POINT('Ctrl Pts',(-8.57413435701442,1.18591009260191,9.92424400295927));
#13345=CARTESIAN_POINT('Ctrl Pts',(-8.27600348990046,1.20454703673243,9.91224081616995));
#13346=CARTESIAN_POINT('Ctrl Pts',(-7.97209482032087,1.10563290540106,9.90023762938063));
#13347=CARTESIAN_POINT('Ctrl Pts',(-7.74204705372056,0.915087963996535,
9.88823444259131));
#13348=CARTESIAN_POINT('Ctrl Pts',(-7.51199928712025,0.724543022592006,
9.87623125580199));
#13349=CARTESIAN_POINT('Ctrl Pts',(-7.35822688079632,0.444367128061413,
9.86422806901268));
#13350=CARTESIAN_POINT('Ctrl Pts',(-7.32102560975816,0.14797985599024,9.85222488222336));
#13351=CARTESIAN_POINT('Ctrl Pts',(-7.28382433872001,-0.148407416080933,
9.84022169543404));
#13352=CARTESIAN_POINT('Ctrl Pts',(-7.36358464744638,-0.457895344722009,
9.82821850864472));
#13353=CARTESIAN_POINT('Ctrl Pts',(-7.53940549437885,-0.699383189957739,
9.8162153218554));
#13354=CARTESIAN_POINT('Ctrl Pts',(-7.71522634131132,-0.940871035193468,
9.80421213506609));
#13355=CARTESIAN_POINT('Ctrl Pts',(-7.98526240565788,-1.11182427083084,
9.79220894827677));
#13356=CARTESIAN_POINT('Ctrl Pts',(-8.27875123560121,-1.16744491727748,
9.78020576148745));
#13357=CARTESIAN_POINT('Ctrl Pts',(-8.57224006554454,-1.22306556372411,
9.76820257469813));
#13358=CARTESIAN_POINT('Ctrl Pts',(-8.88610136059945,-1.16276985667023,
9.75619938790882));
#13359=CARTESIAN_POINT('Ctrl Pts',(-9.13808834820098,-1.00235817476347,
9.7441962011195));
#13360=CARTESIAN_POINT('Ctrl Pts',(-9.3900753358025,-0.841946492856709,
9.73219301433018));
#13361=CARTESIAN_POINT('Ctrl Pts',(-9.57754329642139,-0.583102430602876,
9.72018982754086));
#13362=CARTESIAN_POINT('Ctrl Pts',(-9.65136659729192,-0.293655596346177,
9.70818664075154));
#13363=CARTESIAN_POINT('Ctrl Pts',(-9.67581103310543,-0.197813707972472,
9.70421213506609));
#13364=CARTESIAN_POINT('Ctrl Pts',(-9.688225,-0.0989100500923605,9.70023762938063));
#13365=CARTESIAN_POINT('Ctrl Pts',(-9.688225,2.70894418008538E-14,9.69626312369518));
#13366=CARTESIAN_POINT('Ctrl Pts',(-9.688225,-1.69009251038688E-12,9.65373687630491));
#13367=CARTESIAN_POINT('Ctrl Pts',(-9.68822499999957,-0.298712821307784,
9.66574006309422));
#13368=CARTESIAN_POINT('Ctrl Pts',(-9.57054245632501,-0.595858078273051,
9.67774324988354));
#13369=CARTESIAN_POINT('Ctrl Pts',(-9.36601586214819,-0.813569405233951,
9.68974643667286));
#13370=CARTESIAN_POINT('Ctrl Pts',(-9.16148926797137,-1.03128073219485,
9.70174962346218));
#13371=CARTESIAN_POINT('Ctrl Pts',(-8.8722652241268,-1.16727314847189,9.7137528102515));
#13372=CARTESIAN_POINT('Ctrl Pts',(-8.57413435701282,-1.185910092602,9.72575599704081));
#13373=CARTESIAN_POINT('Ctrl Pts',(-8.27600348989883,-1.20454703673212,
9.73775918383013));
#13374=CARTESIAN_POINT('Ctrl Pts',(-7.97209482031938,-1.10563290540035,
9.74976237061945));
#13375=CARTESIAN_POINT('Ctrl Pts',(-7.74204705371933,-0.915087963995512,
9.76176555740877));
#13376=CARTESIAN_POINT('Ctrl Pts',(-7.51199928711928,-0.724543022590673,
9.77376874419808));
#13377=CARTESIAN_POINT('Ctrl Pts',(-7.35822688079572,-0.444367128059873,
9.7857719309874));
#13378=CARTESIAN_POINT('Ctrl Pts',(-7.32102560975796,-0.147979855988649,
9.79777511777672));
#13379=CARTESIAN_POINT('Ctrl Pts',(-7.28382433872021,0.148407416082574,
9.80977830456604));
#13380=CARTESIAN_POINT('Ctrl Pts',(-7.363584647447,0.457895344723542,9.82178149135536));
#13381=CARTESIAN_POINT('Ctrl Pts',(-7.5394054943798,0.699383189959035,9.83378467814468));
#13382=CARTESIAN_POINT('Ctrl Pts',(-7.71522634131259,0.940871035194527,
9.84578786493399));
#13383=CARTESIAN_POINT('Ctrl Pts',(-7.98526240565938,1.11182427083154,9.85779105172331));
#13384=CARTESIAN_POINT('Ctrl Pts',(-8.27875123560279,1.16744491727777,9.86979423851263));
#13385=CARTESIAN_POINT('Ctrl Pts',(-8.57224006554619,1.22306556372401,9.88179742530195));
#13386=CARTESIAN_POINT('Ctrl Pts',(-8.88610136060102,1.16276985666971,9.89380061209126));
#13387=CARTESIAN_POINT('Ctrl Pts',(-9.13808834820233,1.00235817476261,9.90580379888058));
#13388=CARTESIAN_POINT('Ctrl Pts',(-9.39007533580364,0.841946492855508,
9.9178069856699));
#13389=CARTESIAN_POINT('Ctrl Pts',(-9.57754329642217,0.583102430601421,
9.92981017245922));
#13390=CARTESIAN_POINT('Ctrl Pts',(-9.65136659729231,0.293655596344623,
9.94181335924854));
#13391=CARTESIAN_POINT('Ctrl Pts',(-9.6758110331057,0.197813707970874,9.94578786493399));
#13392=CARTESIAN_POINT('Ctrl Pts',(-9.68822500000014,0.0989100500907344,
9.94976237061945));
#13393=CARTESIAN_POINT('Ctrl Pts',(-9.688225,-1.66444635851803E-12,9.95373687630491));
#13394=CARTESIAN_POINT('Origin',(-8.5,0.,1.8));
#13395=CARTESIAN_POINT('',(-9.688225,7.84927678409986E-14,10.2962631236952));
#13396=CARTESIAN_POINT('',(-9.688225,-1.67266200890026E-12,10.2537368763049));
#13397=CARTESIAN_POINT('',(-9.688225,-1.45515594291686E-16,1.8));
#13398=CARTESIAN_POINT('Ctrl Pts',(-9.688225,1.12132525487141E-13,10.2962631236952));
#13399=CARTESIAN_POINT('Ctrl Pts',(-9.68822499999997,0.298712821306206,
10.2842599369059));
#13400=CARTESIAN_POINT('Ctrl Pts',(-9.57054245632581,0.59585807827163,10.2722567501165));
#13401=CARTESIAN_POINT('Ctrl Pts',(-9.36601586214927,0.813569405232801,
10.2602535633272));
#13402=CARTESIAN_POINT('Ctrl Pts',(-9.16148926797274,1.03128073219397,10.2482503765379));
#13403=CARTESIAN_POINT('Ctrl Pts',(-8.87226522412835,1.16727314847139,10.2362471897486));
#13404=CARTESIAN_POINT('Ctrl Pts',(-8.57413435701439,1.18591009260191,10.2242440029593));
#13405=CARTESIAN_POINT('Ctrl Pts',(-8.27600348990043,1.20454703673242,10.2122408161699));
#13406=CARTESIAN_POINT('Ctrl Pts',(-7.97209482032085,1.10563290540105,10.2002376293806));
#13407=CARTESIAN_POINT('Ctrl Pts',(-7.74204705372054,0.915087963996519,
10.1882344425913));
#13408=CARTESIAN_POINT('Ctrl Pts',(-7.51199928712024,0.724543022591985,
10.176231255802));
#13409=CARTESIAN_POINT('Ctrl Pts',(-7.35822688079631,0.444367128061389,
10.1642280690127));
#13410=CARTESIAN_POINT('Ctrl Pts',(-7.32102560975816,0.147979855990215,
10.1522248822234));
#13411=CARTESIAN_POINT('Ctrl Pts',(-7.28382433872001,-0.148407416080959,
10.140221695434));
#13412=CARTESIAN_POINT('Ctrl Pts',(-7.36358464744639,-0.457895344722033,
10.1282185086447));
#13413=CARTESIAN_POINT('Ctrl Pts',(-7.53940549437887,-0.699383189957759,
10.1162153218554));
#13414=CARTESIAN_POINT('Ctrl Pts',(-7.71522634131134,-0.940871035193485,
10.1042121350661));
#13415=CARTESIAN_POINT('Ctrl Pts',(-7.98526240565791,-1.11182427083086,
10.0922089482768));
#13416=CARTESIAN_POINT('Ctrl Pts',(-8.27875123560124,-1.16744491727748,
10.0802057614875));
#13417=CARTESIAN_POINT('Ctrl Pts',(-8.57224006554457,-1.22306556372411,
10.0682025746981));
#13418=CARTESIAN_POINT('Ctrl Pts',(-8.88610136059948,-1.16276985667022,
10.0561993879088));
#13419=CARTESIAN_POINT('Ctrl Pts',(-9.138088348201,-1.00235817476345,10.0441962011195));
#13420=CARTESIAN_POINT('Ctrl Pts',(-9.39007533580252,-0.84194649285669,
10.0321930143302));
#13421=CARTESIAN_POINT('Ctrl Pts',(-9.5775432964214,-0.583102430602852,
10.0201898275409));
#13422=CARTESIAN_POINT('Ctrl Pts',(-9.65136659729193,-0.293655596346152,
10.0081866407515));
#13423=CARTESIAN_POINT('Ctrl Pts',(-9.67581103310544,-0.197813707972436,
10.0042121350661));
#13424=CARTESIAN_POINT('Ctrl Pts',(-9.68822500000001,-0.0989100500923123,
10.0002376293806));
#13425=CARTESIAN_POINT('Ctrl Pts',(-9.688225,8.65973959207622E-14,9.99626312369517));
#13426=CARTESIAN_POINT('Ctrl Pts',(-9.688225,-1.66444635851803E-12,9.95373687630491));
#13427=CARTESIAN_POINT('Ctrl Pts',(-9.68822499999958,-0.298712821307758,
9.96574006309422));
#13428=CARTESIAN_POINT('Ctrl Pts',(-9.57054245632503,-0.595858078273028,
9.97774324988354));
#13429=CARTESIAN_POINT('Ctrl Pts',(-9.36601586214821,-0.813569405233932,
9.98974643667286));
#13430=CARTESIAN_POINT('Ctrl Pts',(-9.16148926797139,-1.03128073219484,
10.0017496234622));
#13431=CARTESIAN_POINT('Ctrl Pts',(-8.87226522412683,-1.16727314847188,
10.0137528102515));
#13432=CARTESIAN_POINT('Ctrl Pts',(-8.57413435701284,-1.185910092602,10.0257559970408));
#13433=CARTESIAN_POINT('Ctrl Pts',(-8.27600348989886,-1.20454703673213,
10.0377591838301));
#13434=CARTESIAN_POINT('Ctrl Pts',(-7.97209482031941,-1.10563290540036,
10.0497623706194));
#13435=CARTESIAN_POINT('Ctrl Pts',(-7.74204705371935,-0.915087963995528,
10.0617655574088));
#13436=CARTESIAN_POINT('Ctrl Pts',(-7.51199928711929,-0.724543022590694,
10.0737687441981));
#13437=CARTESIAN_POINT('Ctrl Pts',(-7.35822688079573,-0.444367128059897,
10.0857719309874));
#13438=CARTESIAN_POINT('Ctrl Pts',(-7.32102560975797,-0.147979855988675,
10.0977751177767));
#13439=CARTESIAN_POINT('Ctrl Pts',(-7.2838243387202,0.148407416082548,10.109778304566));
#13440=CARTESIAN_POINT('Ctrl Pts',(-7.36358464744699,0.457895344723518,
10.1217814913554));
#13441=CARTESIAN_POINT('Ctrl Pts',(-7.53940549437978,0.699383189959014,
10.1337846781447));
#13442=CARTESIAN_POINT('Ctrl Pts',(-7.71522634131257,0.94087103519451,10.145787864934));
#13443=CARTESIAN_POINT('Ctrl Pts',(-7.98526240565936,1.11182427083153,10.1577910517233));
#13444=CARTESIAN_POINT('Ctrl Pts',(-8.27875123560277,1.16744491727777,10.1697942385126));
#13445=CARTESIAN_POINT('Ctrl Pts',(-8.57224006554617,1.22306556372401,10.1817974253019));
#13446=CARTESIAN_POINT('Ctrl Pts',(-8.88610136060099,1.16276985666971,10.1938006120913));
#13447=CARTESIAN_POINT('Ctrl Pts',(-9.13808834820231,1.00235817476262,10.2058037988806));
#13448=CARTESIAN_POINT('Ctrl Pts',(-9.39007533580362,0.841946492855527,
10.2178069856699));
#13449=CARTESIAN_POINT('Ctrl Pts',(-9.57754329642216,0.583102430601445,
10.2298101724592));
#13450=CARTESIAN_POINT('Ctrl Pts',(-9.65136659729231,0.293655596344648,
10.2418133592485));
#13451=CARTESIAN_POINT('Ctrl Pts',(-9.6758110331057,0.1978137079709,10.245787864934));
#13452=CARTESIAN_POINT('Ctrl Pts',(-9.68822500000014,0.09891005009076,10.2497623706194));
#13453=CARTESIAN_POINT('Ctrl Pts',(-9.688225,-1.63885571780042E-12,10.2537368763049));
#13454=CARTESIAN_POINT('Origin',(-8.5,0.,1.8));
#13455=CARTESIAN_POINT('',(-9.688225,1.0413891970984E-13,10.5962631236952));
#13456=CARTESIAN_POINT('',(-9.688225,-1.64701585703142E-12,10.5537368763049));
#13457=CARTESIAN_POINT('',(-9.688225,-1.45515594291686E-16,1.8));
#13458=CARTESIAN_POINT('Ctrl Pts',(-9.688225,1.37778677355982E-13,10.5962631236952));
#13459=CARTESIAN_POINT('Ctrl Pts',(-9.68822499999997,0.29871282130622,10.5842599369059));
#13460=CARTESIAN_POINT('Ctrl Pts',(-9.5705424563258,0.595858078271631,10.5722567501165));
#13461=CARTESIAN_POINT('Ctrl Pts',(-9.36601586214928,0.813569405232795,
10.5602535633272));
#13462=CARTESIAN_POINT('Ctrl Pts',(-9.16148926797275,1.03128073219396,10.5482503765379));
#13463=CARTESIAN_POINT('Ctrl Pts',(-8.87226522412838,1.16727314847138,10.5362471897486));
#13464=CARTESIAN_POINT('Ctrl Pts',(-8.57413435701443,1.1859100926019,10.5242440029593));
#13465=CARTESIAN_POINT('Ctrl Pts',(-8.27600348990048,1.20454703673243,10.5122408161699));
#13466=CARTESIAN_POINT('Ctrl Pts',(-7.97209482032091,1.10563290540108,10.5002376293806));
#13467=CARTESIAN_POINT('Ctrl Pts',(-7.7420470537206,0.915087963996567,10.4882344425913));
#13468=CARTESIAN_POINT('Ctrl Pts',(-7.51199928712029,0.724543022592055,
10.476231255802));
#13469=CARTESIAN_POINT('Ctrl Pts',(-7.35822688079635,0.444367128061483,
10.4642280690127));
#13470=CARTESIAN_POINT('Ctrl Pts',(-7.32102560975817,0.147979855990323,
10.4522248822234));
#13471=CARTESIAN_POINT('Ctrl Pts',(-7.28382433872,-0.148407416080836,10.440221695434));
#13472=CARTESIAN_POINT('Ctrl Pts',(-7.36358464744634,-0.457895344721905,
10.4282185086447));
#13473=CARTESIAN_POINT('Ctrl Pts',(-7.53940549437878,-0.699383189957643,
10.4162153218554));
#13474=CARTESIAN_POINT('Ctrl Pts',(-7.71522634131122,-0.940871035193382,
10.4042121350661));
#13475=CARTESIAN_POINT('Ctrl Pts',(-7.98526240565775,-1.11182427083078,
10.3922089482768));
#13476=CARTESIAN_POINT('Ctrl Pts',(-8.27875123560107,-1.16744491727745,
10.3802057614875));
#13477=CARTESIAN_POINT('Ctrl Pts',(-8.57224006554438,-1.22306556372411,
10.3682025746981));
#13478=CARTESIAN_POINT('Ctrl Pts',(-8.88610136059928,-1.16276985667028,
10.3561993879088));
#13479=CARTESIAN_POINT('Ctrl Pts',(-9.13808834820082,-1.00235817476357,
10.3441962011195));
#13480=CARTESIAN_POINT('Ctrl Pts',(-9.39007533580236,-0.841946492856854,
10.3321930143302));
#13481=CARTESIAN_POINT('Ctrl Pts',(-9.57754329642128,-0.583102430603063,
10.3201898275409));
#13482=CARTESIAN_POINT('Ctrl Pts',(-9.65136659729187,-0.293655596346389,
10.3081866407516));
#13483=CARTESIAN_POINT('Ctrl Pts',(-9.67581103310542,-0.19781370797259,
10.3042121350661));
#13484=CARTESIAN_POINT('Ctrl Pts',(-9.68822500000001,-0.0989100500923768,
10.3002376293806));
#13485=CARTESIAN_POINT('Ctrl Pts',(-9.688225,1.12132525487141E-13,10.2962631236952));
#13486=CARTESIAN_POINT('Ctrl Pts',(-9.688225,-1.63885571780042E-12,10.2537368763049));
#13487=CARTESIAN_POINT('Ctrl Pts',(-9.68822499999959,-0.298712821307732,
10.2657400630942));
#13488=CARTESIAN_POINT('Ctrl Pts',(-9.57054245632504,-0.595858078273005,
10.2777432498835));
#13489=CARTESIAN_POINT('Ctrl Pts',(-9.36601586214823,-0.813569405233914,
10.2897464366729));
#13490=CARTESIAN_POINT('Ctrl Pts',(-9.16148926797141,-1.03128073219482,
10.3017496234622));
#13491=CARTESIAN_POINT('Ctrl Pts',(-8.87226522412685,-1.16727314847187,
10.3137528102515));
#13492=CARTESIAN_POINT('Ctrl Pts',(-8.57413435701287,-1.185910092602,10.3257559970408));
#13493=CARTESIAN_POINT('Ctrl Pts',(-8.27600348989888,-1.20454703673213,
10.3377591838301));
#13494=CARTESIAN_POINT('Ctrl Pts',(-7.97209482031943,-1.10563290540037,
10.3497623706194));
#13495=CARTESIAN_POINT('Ctrl Pts',(-7.74204705371937,-0.915087963995544,
10.3617655574088));
#13496=CARTESIAN_POINT('Ctrl Pts',(-7.51199928711931,-0.724543022590715,
10.3737687441981));
#13497=CARTESIAN_POINT('Ctrl Pts',(-7.35822688079574,-0.444367128059922,
10.3857719309874));
#13498=CARTESIAN_POINT('Ctrl Pts',(-7.32102560975797,-0.1479798559887,10.3977751177767));
#13499=CARTESIAN_POINT('Ctrl Pts',(-7.2838243387202,0.148407416082522,10.409778304566));
#13500=CARTESIAN_POINT('Ctrl Pts',(-7.36358464744698,0.457895344723493,
10.4217814913554));
#13501=CARTESIAN_POINT('Ctrl Pts',(-7.53940549437977,0.699383189958993,
10.4337846781447));
#13502=CARTESIAN_POINT('Ctrl Pts',(-7.71522634131255,0.940871035194494,
10.445787864934));
#13503=CARTESIAN_POINT('Ctrl Pts',(-7.98526240565934,1.11182427083152,10.4577910517233));
#13504=CARTESIAN_POINT('Ctrl Pts',(-8.27875123560274,1.16744491727776,10.4697942385126));
#13505=CARTESIAN_POINT('Ctrl Pts',(-8.57224006554614,1.22306556372401,10.4817974253019));
#13506=CARTESIAN_POINT('Ctrl Pts',(-8.88610136060097,1.16276985666972,10.4938006120913));
#13507=CARTESIAN_POINT('Ctrl Pts',(-9.13808834820228,1.00235817476263,10.5058037988806));
#13508=CARTESIAN_POINT('Ctrl Pts',(-9.3900753358036,0.841946492855546,10.5178069856699));
#13509=CARTESIAN_POINT('Ctrl Pts',(-9.57754329642215,0.583102430601468,
10.5298101724592));
#13510=CARTESIAN_POINT('Ctrl Pts',(-9.6513665972923,0.293655596344673,10.5418133592485));
#13511=CARTESIAN_POINT('Ctrl Pts',(-9.67581103310569,0.197813707970925,
10.545787864934));
#13512=CARTESIAN_POINT('Ctrl Pts',(-9.68822500000013,0.0989100500907857,
10.5497623706194));
#13513=CARTESIAN_POINT('Ctrl Pts',(-9.688225,-1.61320956593158E-12,10.5537368763049));
#13514=CARTESIAN_POINT('Origin',(-8.5,0.,1.8));
#13515=CARTESIAN_POINT('',(-9.688225,1.29674049276218E-13,10.8962631236952));
#13516=CARTESIAN_POINT('',(-9.688225,-1.62142521631381E-12,10.8537368763049));
#13517=CARTESIAN_POINT('',(-9.688225,-1.45515594291686E-16,1.8));
#13518=CARTESIAN_POINT('Ctrl Pts',(-9.688225,1.29674049276218E-13,10.8962631236952));
#13519=CARTESIAN_POINT('Ctrl Pts',(-9.68822499999997,0.298712821306223,
10.8842599369059));
#13520=CARTESIAN_POINT('Ctrl Pts',(-9.57054245632579,0.595858078271646,
10.8722567501165));
#13521=CARTESIAN_POINT('Ctrl Pts',(-9.36601586214926,0.813569405232814,
10.8602535633272));
#13522=CARTESIAN_POINT('Ctrl Pts',(-9.16148926797272,1.03128073219398,10.8482503765379));
#13523=CARTESIAN_POINT('Ctrl Pts',(-8.87226522412834,1.1672731484714,10.8362471897486));
#13524=CARTESIAN_POINT('Ctrl Pts',(-8.57413435701437,1.18591009260191,10.8242440029593));
#13525=CARTESIAN_POINT('Ctrl Pts',(-8.27600348990041,1.20454703673242,10.8122408161699));
#13526=CARTESIAN_POINT('Ctrl Pts',(-7.97209482032083,1.10563290540104,10.8002376293806));
#13527=CARTESIAN_POINT('Ctrl Pts',(-7.74204705372053,0.915087963996507,
10.7882344425913));
#13528=CARTESIAN_POINT('Ctrl Pts',(-7.51199928712023,0.72454302259197,10.776231255802));
#13529=CARTESIAN_POINT('Ctrl Pts',(-7.35822688079631,0.444367128061372,
10.7642280690127));
#13530=CARTESIAN_POINT('Ctrl Pts',(-7.32102560975816,0.147979855990197,
10.7522248822234));
#13531=CARTESIAN_POINT('Ctrl Pts',(-7.28382433872001,-0.148407416080977,
10.740221695434));
#13532=CARTESIAN_POINT('Ctrl Pts',(-7.3635846474464,-0.45789534472205,10.7282185086447));
#13533=CARTESIAN_POINT('Ctrl Pts',(-7.53940549437888,-0.699383189957773,
10.7162153218554));
#13534=CARTESIAN_POINT('Ctrl Pts',(-7.71522634131135,-0.940871035193497,
10.7042121350661));
#13535=CARTESIAN_POINT('Ctrl Pts',(-7.98526240565793,-1.11182427083086,
10.6922089482768));
#13536=CARTESIAN_POINT('Ctrl Pts',(-8.27875123560126,-1.16744491727748,
10.6802057614874));
#13537=CARTESIAN_POINT('Ctrl Pts',(-8.57224006554459,-1.2230655637241,10.6682025746981));
#13538=CARTESIAN_POINT('Ctrl Pts',(-8.88610136059949,-1.16276985667021,
10.6561993879088));
#13539=CARTESIAN_POINT('Ctrl Pts',(-9.13808834820101,-1.00235817476344,
10.6441962011195));
#13540=CARTESIAN_POINT('Ctrl Pts',(-9.39007533580253,-0.841946492856677,
10.6321930143302));
#13541=CARTESIAN_POINT('Ctrl Pts',(-9.57754329642141,-0.583102430602837,
10.6201898275409));
#13542=CARTESIAN_POINT('Ctrl Pts',(-9.65136659729193,-0.293655596346135,
10.6081866407515));
#13543=CARTESIAN_POINT('Ctrl Pts',(-9.67581103310544,-0.197813707972407,
10.6042121350661));
#13544=CARTESIAN_POINT('Ctrl Pts',(-9.68822500000001,-0.0989100500922724,
10.6002376293806));
#13545=CARTESIAN_POINT('Ctrl Pts',(-9.688225,1.37778677355982E-13,10.5962631236952));
#13546=CARTESIAN_POINT('Ctrl Pts',(-9.688225,-1.61320956593158E-12,10.5537368763049));
#13547=CARTESIAN_POINT('Ctrl Pts',(-9.68822499999959,-0.298712821307707,
10.5657400630942));
#13548=CARTESIAN_POINT('Ctrl Pts',(-9.57054245632505,-0.595858078272982,
10.5777432498835));
#13549=CARTESIAN_POINT('Ctrl Pts',(-9.36601586214824,-0.813569405233895,
10.5897464366729));
#13550=CARTESIAN_POINT('Ctrl Pts',(-9.16148926797144,-1.03128073219481,
10.6017496234622));
#13551=CARTESIAN_POINT('Ctrl Pts',(-8.87226522412688,-1.16727314847186,
10.6137528102515));
#13552=CARTESIAN_POINT('Ctrl Pts',(-8.57413435701289,-1.185910092602,10.6257559970408));
#13553=CARTESIAN_POINT('Ctrl Pts',(-8.27600348989891,-1.20454703673214,
10.6377591838301));
#13554=CARTESIAN_POINT('Ctrl Pts',(-7.97209482031945,-1.10563290540038,
10.6497623706194));
#13555=CARTESIAN_POINT('Ctrl Pts',(-7.74204705371939,-0.915087963995561,
10.6617655574088));
#13556=CARTESIAN_POINT('Ctrl Pts',(-7.51199928711932,-0.724543022590736,
10.6737687441981));
#13557=CARTESIAN_POINT('Ctrl Pts',(-7.35822688079575,-0.444367128059946,
10.6857719309874));
#13558=CARTESIAN_POINT('Ctrl Pts',(-7.32102560975797,-0.147979855988725,
10.6977751177767));
#13559=CARTESIAN_POINT('Ctrl Pts',(-7.2838243387202,0.148407416082496,10.709778304566));
#13560=CARTESIAN_POINT('Ctrl Pts',(-7.36358464744697,0.457895344723468,
10.7217814913554));
#13561=CARTESIAN_POINT('Ctrl Pts',(-7.53940549437975,0.699383189958973,
10.7337846781447));
#13562=CARTESIAN_POINT('Ctrl Pts',(-7.71522634131253,0.940871035194477,
10.745787864934));
#13563=CARTESIAN_POINT('Ctrl Pts',(-7.98526240565931,1.11182427083151,10.7577910517233));
#13564=CARTESIAN_POINT('Ctrl Pts',(-8.27875123560271,1.16744491727776,10.7697942385126));
#13565=CARTESIAN_POINT('Ctrl Pts',(-8.57224006554612,1.22306556372401,10.7817974253019));
#13566=CARTESIAN_POINT('Ctrl Pts',(-8.88610136060094,1.16276985666973,10.7938006120913));
#13567=CARTESIAN_POINT('Ctrl Pts',(-9.13808834820226,1.00235817476265,10.8058037988806));
#13568=CARTESIAN_POINT('Ctrl Pts',(-9.39007533580358,0.841946492855566,
10.8178069856699));
#13569=CARTESIAN_POINT('Ctrl Pts',(-9.57754329642214,0.583102430601491,
10.8298101724592));
#13570=CARTESIAN_POINT('Ctrl Pts',(-9.6513665972923,0.293655596344697,10.8418133592485));
#13571=CARTESIAN_POINT('Ctrl Pts',(-9.67581103310569,0.19781370797095,10.845787864934));
#13572=CARTESIAN_POINT('Ctrl Pts',(-9.68822500000013,0.0989100500908113,
10.8497623706194));
#13573=CARTESIAN_POINT('Ctrl Pts',(-9.688225,-1.58756341406274E-12,10.8537368763049));
#13574=CARTESIAN_POINT('Origin',(-8.5,0.,1.8));
#13575=CARTESIAN_POINT('',(-9.688225,1.55320201145059E-13,11.1962631236952));
#13576=CARTESIAN_POINT('',(-9.688225,-1.59577906444497E-12,11.1537368763049));
#13577=CARTESIAN_POINT('',(-9.688225,-1.45515594291686E-16,1.8));
#13578=CARTESIAN_POINT('Ctrl Pts',(-9.688225,1.55320201145059E-13,11.1962631236952));
#13579=CARTESIAN_POINT('Ctrl Pts',(-9.68822499999996,0.29871282130626,11.1842599369059));
#13580=CARTESIAN_POINT('Ctrl Pts',(-9.57054245632577,0.595858078271691,
11.1722567501165));
#13581=CARTESIAN_POINT('Ctrl Pts',(-9.36601586214922,0.813569405232857,
11.1602535633272));
#13582=CARTESIAN_POINT('Ctrl Pts',(-9.16148926797266,1.03128073219402,11.1482503765379));
#13583=CARTESIAN_POINT('Ctrl Pts',(-8.87226522412826,1.16727314847143,11.1362471897486));
#13584=CARTESIAN_POINT('Ctrl Pts',(-8.57413435701428,1.18591009260191,11.1242440029593));
#13585=CARTESIAN_POINT('Ctrl Pts',(-8.27600348990031,1.2045470367324,11.1122408161699));
#13586=CARTESIAN_POINT('Ctrl Pts',(-7.97209482032072,1.105632905401,11.1002376293806));
#13587=CARTESIAN_POINT('Ctrl Pts',(-7.74204705372043,0.915087963996426,
11.0882344425913));
#13588=CARTESIAN_POINT('Ctrl Pts',(-7.51199928712014,0.724543022591858,
11.076231255802));
#13589=CARTESIAN_POINT('Ctrl Pts',(-7.35822688079625,0.444367128061229,
11.0642280690127));
#13590=CARTESIAN_POINT('Ctrl Pts',(-7.32102560975814,0.147979855990038,
11.0522248822234));
#13591=CARTESIAN_POINT('Ctrl Pts',(-7.28382433872003,-0.148407416081153,
11.040221695434));
#13592=CARTESIAN_POINT('Ctrl Pts',(-7.36358464744647,-0.457895344722227,
11.0282185086447));
#13593=CARTESIAN_POINT('Ctrl Pts',(-7.53940549437899,-0.699383189957931,
11.0162153218554));
#13594=CARTESIAN_POINT('Ctrl Pts',(-7.71522634131151,-0.940871035193635,
11.0042121350661));
#13595=CARTESIAN_POINT('Ctrl Pts',(-7.98526240565813,-1.11182427083096,
10.9922089482768));
#13596=CARTESIAN_POINT('Ctrl Pts',(-8.27875123560148,-1.16744491727753,
10.9802057614874));
#13597=CARTESIAN_POINT('Ctrl Pts',(-8.57224006554484,-1.22306556372409,
10.9682025746981));
#13598=CARTESIAN_POINT('Ctrl Pts',(-8.88610136059974,-1.16276985667013,
10.9561993879088));
#13599=CARTESIAN_POINT('Ctrl Pts',(-9.13808834820123,-1.0023581747633,10.9441962011195));
#13600=CARTESIAN_POINT('Ctrl Pts',(-9.39007533580273,-0.841946492856475,
10.9321930143302));
#13601=CARTESIAN_POINT('Ctrl Pts',(-9.57754329642155,-0.583102430602579,
10.9201898275408));
#13602=CARTESIAN_POINT('Ctrl Pts',(-9.651366597292,-0.293655596345848,10.9081866407515));
#13603=CARTESIAN_POINT('Ctrl Pts',(-9.67581103310547,-0.197813707972213,
10.9042121350661));
#13604=CARTESIAN_POINT('Ctrl Pts',(-9.68822500000001,-0.0989100500921791,
10.9002376293806));
#13605=CARTESIAN_POINT('Ctrl Pts',(-9.688225,1.29674049276218E-13,10.8962631236952));
#13606=CARTESIAN_POINT('Ctrl Pts',(-9.688225,-1.58756341406274E-12,10.8537368763049));
#13607=CARTESIAN_POINT('Ctrl Pts',(-9.6882249999996,-0.298712821307681,
10.8657400630942));
#13608=CARTESIAN_POINT('Ctrl Pts',(-9.57054245632506,-0.595858078272959,
10.8777432498835));
#13609=CARTESIAN_POINT('Ctrl Pts',(-9.36601586214826,-0.813569405233876,
10.8897464366729));
#13610=CARTESIAN_POINT('Ctrl Pts',(-9.16148926797146,-1.03128073219479,
10.9017496234622));
#13611=CARTESIAN_POINT('Ctrl Pts',(-8.8722652241269,-1.16727314847185,10.9137528102515));
#13612=CARTESIAN_POINT('Ctrl Pts',(-8.57413435701292,-1.185910092602,10.9257559970408));
#13613=CARTESIAN_POINT('Ctrl Pts',(-8.27600348989893,-1.20454703673214,
10.9377591838301));
#13614=CARTESIAN_POINT('Ctrl Pts',(-7.97209482031948,-1.1056329054004,10.9497623706194));
#13615=CARTESIAN_POINT('Ctrl Pts',(-7.74204705371941,-0.915087963995577,
10.9617655574088));
#13616=CARTESIAN_POINT('Ctrl Pts',(-7.51199928711934,-0.724543022590758,
10.9737687441981));
#13617=CARTESIAN_POINT('Ctrl Pts',(-7.35822688079576,-0.444367128059971,
10.9857719309874));
#13618=CARTESIAN_POINT('Ctrl Pts',(-7.32102560975798,-0.147979855988751,
10.9977751177767));
#13619=CARTESIAN_POINT('Ctrl Pts',(-7.2838243387202,0.148407416082469,11.009778304566));
#13620=CARTESIAN_POINT('Ctrl Pts',(-7.36358464744696,0.457895344723444,
11.0217814913554));
#13621=CARTESIAN_POINT('Ctrl Pts',(-7.53940549437974,0.699383189958952,
11.0337846781447));
#13622=CARTESIAN_POINT('Ctrl Pts',(-7.71522634131251,0.94087103519446,11.045787864934));
#13623=CARTESIAN_POINT('Ctrl Pts',(-7.98526240565929,1.11182427083149,11.0577910517233));
#13624=CARTESIAN_POINT('Ctrl Pts',(-8.27875123560269,1.16744491727775,11.0697942385126));
#13625=CARTESIAN_POINT('Ctrl Pts',(-8.57224006554609,1.22306556372402,11.0817974253019));
#13626=CARTESIAN_POINT('Ctrl Pts',(-8.88610136060092,1.16276985666974,11.0938006120913));
#13627=CARTESIAN_POINT('Ctrl Pts',(-9.13808834820224,1.00235817476266,11.1058037988806));
#13628=CARTESIAN_POINT('Ctrl Pts',(-9.39007533580356,0.841946492855585,
11.1178069856699));
#13629=CARTESIAN_POINT('Ctrl Pts',(-9.57754329642212,0.583102430601514,
11.1298101724592));
#13630=CARTESIAN_POINT('Ctrl Pts',(-9.65136659729229,0.293655596344722,
11.1418133592485));
#13631=CARTESIAN_POINT('Ctrl Pts',(-9.67581103310568,0.197813707970976,
11.145787864934));
#13632=CARTESIAN_POINT('Ctrl Pts',(-9.68822500000013,0.0989100500908369,
11.1497623706194));
#13633=CARTESIAN_POINT('Ctrl Pts',(-9.688225,-1.56197277334513E-12,11.1537368763049));
#13634=CARTESIAN_POINT('Origin',(-8.5,0.,1.8));
#13635=CARTESIAN_POINT('',(-9.688225,1.80966353013901E-13,11.4962631236952));
#13636=CARTESIAN_POINT('',(-9.688225,-1.57013291257613E-12,11.4537368763049));
#13637=CARTESIAN_POINT('',(-9.688225,-1.45515594291686E-16,1.8));
#13638=CARTESIAN_POINT('Ctrl Pts',(-9.688225,1.80966353013901E-13,11.4962631236952));
#13639=CARTESIAN_POINT('Ctrl Pts',(-9.68822499999995,0.298712821306286,
11.4842599369059));
#13640=CARTESIAN_POINT('Ctrl Pts',(-9.57054245632576,0.595858078271714,
11.4722567501165));
#13641=CARTESIAN_POINT('Ctrl Pts',(-9.3660158621492,0.813569405232876,11.4602535633272));
#13642=CARTESIAN_POINT('Ctrl Pts',(-9.16148926797264,1.03128073219404,11.4482503765379));
#13643=CARTESIAN_POINT('Ctrl Pts',(-8.87226522412823,1.16727314847143,11.4362471897486));
#13644=CARTESIAN_POINT('Ctrl Pts',(-8.57413435701426,1.18591009260192,11.4242440029593));
#13645=CARTESIAN_POINT('Ctrl Pts',(-8.27600348990028,1.2045470367324,11.4122408161699));
#13646=CARTESIAN_POINT('Ctrl Pts',(-7.9720948203207,1.10563290540098,11.4002376293806));
#13647=CARTESIAN_POINT('Ctrl Pts',(-7.74204705372041,0.91508796399641,11.3882344425913));
#13648=CARTESIAN_POINT('Ctrl Pts',(-7.51199928712013,0.724543022591836,
11.376231255802));
#13649=CARTESIAN_POINT('Ctrl Pts',(-7.35822688079624,0.444367128061204,
11.3642280690127));
#13650=CARTESIAN_POINT('Ctrl Pts',(-7.32102560975814,0.147979855990013,
11.3522248822234));
#13651=CARTESIAN_POINT('Ctrl Pts',(-7.28382433872004,-0.148407416081179,
11.340221695434));
#13652=CARTESIAN_POINT('Ctrl Pts',(-7.36358464744648,-0.457895344722251,
11.3282185086447));
#13653=CARTESIAN_POINT('Ctrl Pts',(-7.53940549437901,-0.699383189957951,
11.3162153218554));
#13654=CARTESIAN_POINT('Ctrl Pts',(-7.71522634131153,-0.940871035193652,
11.3042121350661));
#13655=CARTESIAN_POINT('Ctrl Pts',(-7.98526240565815,-1.11182427083097,
11.2922089482768));
#13656=CARTESIAN_POINT('Ctrl Pts',(-8.27875123560151,-1.16744491727753,
11.2802057614874));
#13657=CARTESIAN_POINT('Ctrl Pts',(-8.57224006554486,-1.22306556372409,
11.2682025746981));
#13658=CARTESIAN_POINT('Ctrl Pts',(-8.88610136059977,-1.16276985667013,
11.2561993879088));
#13659=CARTESIAN_POINT('Ctrl Pts',(-9.13808834820125,-1.00235817476329,
11.2441962011195));
#13660=CARTESIAN_POINT('Ctrl Pts',(-9.39007533580274,-0.841946492856455,
11.2321930143302));
#13661=CARTESIAN_POINT('Ctrl Pts',(-9.57754329642156,-0.583102430602556,
11.2201898275408));
#13662=CARTESIAN_POINT('Ctrl Pts',(-9.65136659729201,-0.293655596345824,
11.2081866407515));
#13663=CARTESIAN_POINT('Ctrl Pts',(-9.67581103310547,-0.197813707972188,
11.2042121350661));
#13664=CARTESIAN_POINT('Ctrl Pts',(-9.68822500000001,-0.0989100500921535,
11.2002376293806));
#13665=CARTESIAN_POINT('Ctrl Pts',(-9.688225,1.55320201145059E-13,11.1962631236952));
#13666=CARTESIAN_POINT('Ctrl Pts',(-9.688225,-1.56197277334513E-12,11.1537368763049));
#13667=CARTESIAN_POINT('Ctrl Pts',(-9.68822499999961,-0.298712821307667,
11.1657400630942));
#13668=CARTESIAN_POINT('Ctrl Pts',(-9.57054245632507,-0.595858078272958,
11.1777432498835));
#13669=CARTESIAN_POINT('Ctrl Pts',(-9.36601586214826,-0.813569405233882,
11.1897464366729));
#13670=CARTESIAN_POINT('Ctrl Pts',(-9.16148926797144,-1.03128073219481,
11.2017496234622));
#13671=CARTESIAN_POINT('Ctrl Pts',(-8.87226522412687,-1.16727314847187,
11.2137528102515));
#13672=CARTESIAN_POINT('Ctrl Pts',(-8.57413435701288,-1.185910092602,11.2257559970408));
#13673=CARTESIAN_POINT('Ctrl Pts',(-8.27600348989888,-1.20454703673214,
11.2377591838301));
#13674=CARTESIAN_POINT('Ctrl Pts',(-7.97209482031942,-1.10563290540037,
11.2497623706194));
#13675=CARTESIAN_POINT('Ctrl Pts',(-7.74204705371935,-0.915087963995529,
11.2617655574088));
#13676=CARTESIAN_POINT('Ctrl Pts',(-7.51199928711928,-0.724543022590688,
11.2737687441981));
#13677=CARTESIAN_POINT('Ctrl Pts',(-7.35822688079572,-0.444367128059877,
11.2857719309874));
#13678=CARTESIAN_POINT('Ctrl Pts',(-7.32102560975796,-0.147979855988642,
11.2977751177767));
#13679=CARTESIAN_POINT('Ctrl Pts',(-7.28382433872021,0.148407416082593,
11.309778304566));
#13680=CARTESIAN_POINT('Ctrl Pts',(-7.36358464744701,0.457895344723572,
11.3217814913554));
#13681=CARTESIAN_POINT('Ctrl Pts',(-7.53940549437982,0.699383189959068,
11.3337846781447));
#13682=CARTESIAN_POINT('Ctrl Pts',(-7.71522634131263,0.940871035194563,
11.345787864934));
#13683=CARTESIAN_POINT('Ctrl Pts',(-7.98526240565944,1.11182427083157,11.3577910517233));
#13684=CARTESIAN_POINT('Ctrl Pts',(-8.27875123560286,1.16744491727779,11.3697942385126));
#13685=CARTESIAN_POINT('Ctrl Pts',(-8.57224006554628,1.22306556372401,11.381797425302));
#13686=CARTESIAN_POINT('Ctrl Pts',(-8.88610136060112,1.16276985666968,11.3938006120913));
#13687=CARTESIAN_POINT('Ctrl Pts',(-9.13808834820242,1.00235817476255,11.4058037988806));
#13688=CARTESIAN_POINT('Ctrl Pts',(-9.39007533580372,0.841946492855421,
11.4178069856699));
#13689=CARTESIAN_POINT('Ctrl Pts',(-9.57754329642224,0.583102430601303,
11.4298101724592));
#13690=CARTESIAN_POINT('Ctrl Pts',(-9.65136659729235,0.293655596344485,
11.4418133592485));
#13691=CARTESIAN_POINT('Ctrl Pts',(-9.6758110331057,0.19781370797081,11.445787864934));
#13692=CARTESIAN_POINT('Ctrl Pts',(-9.68822500000013,0.0989100500907499,
11.4497623706194));
#13693=CARTESIAN_POINT('Ctrl Pts',(-9.688225,-1.57013291257613E-12,11.4537368763049));
#13694=CARTESIAN_POINT('Origin',(-8.5,0.,1.8));
#13695=CARTESIAN_POINT('',(-9.688225,2.06501482580279E-13,11.7962631236952));
#13696=CARTESIAN_POINT('',(-9.688225,-1.54454227185852E-12,11.7537368763049));
#13697=CARTESIAN_POINT('',(-9.688225,-1.45515594291686E-16,1.8));
#13698=CARTESIAN_POINT('Ctrl Pts',(-9.688225,2.06501482580279E-13,11.7962631236952));
#13699=CARTESIAN_POINT('Ctrl Pts',(-9.68822499999995,0.298712821306311,
11.7842599369059));
#13700=CARTESIAN_POINT('Ctrl Pts',(-9.57054245632575,0.595858078271737,
11.7722567501165));
#13701=CARTESIAN_POINT('Ctrl Pts',(-9.36601586214918,0.813569405232895,
11.7602535633272));
#13702=CARTESIAN_POINT('Ctrl Pts',(-9.16148926797262,1.03128073219405,11.7482503765379));
#13703=CARTESIAN_POINT('Ctrl Pts',(-8.8722652241282,1.16727314847144,11.7362471897486));
#13704=CARTESIAN_POINT('Ctrl Pts',(-8.57413435701423,1.18591009260192,11.7242440029593));
#13705=CARTESIAN_POINT('Ctrl Pts',(-8.27600348990026,1.20454703673239,11.7122408161699));
#13706=CARTESIAN_POINT('Ctrl Pts',(-7.97209482032068,1.10563290540097,11.7002376293806));
#13707=CARTESIAN_POINT('Ctrl Pts',(-7.74204705372039,0.915087963996394,
11.6882344425913));
#13708=CARTESIAN_POINT('Ctrl Pts',(-7.51199928712011,0.724543022591815,
11.676231255802));
#13709=CARTESIAN_POINT('Ctrl Pts',(-7.35822688079623,0.44436712806118,11.6642280690127));
#13710=CARTESIAN_POINT('Ctrl Pts',(-7.32102560975813,0.147979855989987,
11.6522248822233));
#13711=CARTESIAN_POINT('Ctrl Pts',(-7.28382433872004,-0.148407416081205,
11.640221695434));
#13712=CARTESIAN_POINT('Ctrl Pts',(-7.36358464744649,-0.457895344722276,
11.6282185086447));
#13713=CARTESIAN_POINT('Ctrl Pts',(-7.53940549437902,-0.699383189957972,
11.6162153218554));
#13714=CARTESIAN_POINT('Ctrl Pts',(-7.71522634131155,-0.940871035193668,
11.6042121350661));
#13715=CARTESIAN_POINT('Ctrl Pts',(-7.98526240565817,-1.11182427083098,
11.5922089482768));
#13716=CARTESIAN_POINT('Ctrl Pts',(-8.27875123560153,-1.16744491727754,
11.5802057614874));
#13717=CARTESIAN_POINT('Ctrl Pts',(-8.57224006554489,-1.22306556372409,
11.5682025746981));
#13718=CARTESIAN_POINT('Ctrl Pts',(-8.88610136059979,-1.16276985667012,
11.5561993879088));
#13719=CARTESIAN_POINT('Ctrl Pts',(-9.13808834820128,-1.00235817476328,
11.5441962011195));
#13720=CARTESIAN_POINT('Ctrl Pts',(-9.39007533580276,-0.841946492856436,
11.5321930143302));
#13721=CARTESIAN_POINT('Ctrl Pts',(-9.57754329642158,-0.583102430602533,
11.5201898275408));
#13722=CARTESIAN_POINT('Ctrl Pts',(-9.65136659729202,-0.293655596345799,
11.5081866407515));
#13723=CARTESIAN_POINT('Ctrl Pts',(-9.67581103310548,-0.197813707972162,
11.5042121350661));
#13724=CARTESIAN_POINT('Ctrl Pts',(-9.68822500000002,-0.0989100500921278,
11.5002376293806));
#13725=CARTESIAN_POINT('Ctrl Pts',(-9.688225,1.80966353013901E-13,11.4962631236952));
#13726=CARTESIAN_POINT('Ctrl Pts',(-9.688225,-1.57013291257613E-12,11.4537368763049));
#13727=CARTESIAN_POINT('Ctrl Pts',(-9.6882249999996,-0.298712821307664,
11.4657400630942));
#13728=CARTESIAN_POINT('Ctrl Pts',(-9.57054245632507,-0.595858078272943,
11.4777432498835));
#13729=CARTESIAN_POINT('Ctrl Pts',(-9.36601586214827,-0.813569405233864,
11.4897464366729));
#13730=CARTESIAN_POINT('Ctrl Pts',(-9.16148926797147,-1.03128073219478,
11.5017496234622));
#13731=CARTESIAN_POINT('Ctrl Pts',(-8.87226522412692,-1.16727314847185,
11.5137528102515));
#13732=CARTESIAN_POINT('Ctrl Pts',(-8.57413435701294,-1.185910092602,11.5257559970408));
#13733=CARTESIAN_POINT('Ctrl Pts',(-8.27600348989895,-1.20454703673215,
11.5377591838301));
#13734=CARTESIAN_POINT('Ctrl Pts',(-7.97209482031949,-1.1056329054004,11.5497623706194));
#13735=CARTESIAN_POINT('Ctrl Pts',(-7.74204705371942,-0.915087963995588,
11.5617655574088));
#13736=CARTESIAN_POINT('Ctrl Pts',(-7.51199928711935,-0.724543022590772,
11.5737687441981));
#13737=CARTESIAN_POINT('Ctrl Pts',(-7.35822688079577,-0.444367128059988,
11.5857719309874));
#13738=CARTESIAN_POINT('Ctrl Pts',(-7.32102560975798,-0.147979855988768,
11.5977751177767));
#13739=CARTESIAN_POINT('Ctrl Pts',(-7.28382433872019,0.148407416082451,
11.609778304566));
#13740=CARTESIAN_POINT('Ctrl Pts',(-7.36358464744696,0.457895344723427,
11.6217814913554));
#13741=CARTESIAN_POINT('Ctrl Pts',(-7.53940549437973,0.699383189958938,
11.6337846781447));
#13742=CARTESIAN_POINT('Ctrl Pts',(-7.71522634131249,0.940871035194448,
11.645787864934));
#13743=CARTESIAN_POINT('Ctrl Pts',(-7.98526240565927,1.11182427083149,11.6577910517233));
#13744=CARTESIAN_POINT('Ctrl Pts',(-8.27875123560267,1.16744491727775,11.6697942385126));
#13745=CARTESIAN_POINT('Ctrl Pts',(-8.57224006554607,1.22306556372402,11.6817974253019));
#13746=CARTESIAN_POINT('Ctrl Pts',(-8.8861013606009,1.16276985666974,11.6938006120913));
#13747=CARTESIAN_POINT('Ctrl Pts',(-9.13808834820223,1.00235817476267,11.7058037988806));
#13748=CARTESIAN_POINT('Ctrl Pts',(-9.39007533580355,0.841946492855598,
11.7178069856699));
#13749=CARTESIAN_POINT('Ctrl Pts',(-9.57754329642211,0.58310243060153,11.7298101724592));
#13750=CARTESIAN_POINT('Ctrl Pts',(-9.65136659729228,0.293655596344739,
11.7418133592485));
#13751=CARTESIAN_POINT('Ctrl Pts',(-9.67581103310568,0.197813707970993,
11.745787864934));
#13752=CARTESIAN_POINT('Ctrl Pts',(-9.68822500000013,0.0989100500908544,
11.7497623706194));
#13753=CARTESIAN_POINT('Ctrl Pts',(-9.688225,-1.54454227185852E-12,11.7537368763049));
#13754=CARTESIAN_POINT('Origin',(-8.5,0.,1.8));
#13755=CARTESIAN_POINT('',(-9.688225,2.3214763444912E-13,12.0962631236952));
#13756=CARTESIAN_POINT('',(-9.688225,-1.51884060883845E-12,12.0537368763049));
#13757=CARTESIAN_POINT('',(-9.688225,-1.45515594291686E-16,1.8));
#13758=CARTESIAN_POINT('Ctrl Pts',(-9.688225,2.3214763444912E-13,12.0962631236952));
#13759=CARTESIAN_POINT('Ctrl Pts',(-9.68822499999994,0.298712821306314,
12.0842599369059));
#13760=CARTESIAN_POINT('Ctrl Pts',(-9.57054245632575,0.595858078271716,
12.0722567501165));
#13761=CARTESIAN_POINT('Ctrl Pts',(-9.36601586214921,0.813569405232864,
12.0602535633272));
#13762=CARTESIAN_POINT('Ctrl Pts',(-9.16148926797267,1.03128073219401,12.0482503765379));
#13763=CARTESIAN_POINT('Ctrl Pts',(-8.87226522412829,1.16727314847141,12.0362471897486));
#13764=CARTESIAN_POINT('Ctrl Pts',(-8.57413435701434,1.18591009260191,12.0242440029593));
#13765=CARTESIAN_POINT('Ctrl Pts',(-8.27600348990039,1.20454703673241,12.0122408161699));
#13766=CARTESIAN_POINT('Ctrl Pts',(-7.97209482032082,1.10563290540104,12.0002376293806));
#13767=CARTESIAN_POINT('Ctrl Pts',(-7.74204705372053,0.915087963996507,
11.9882344425913));
#13768=CARTESIAN_POINT('Ctrl Pts',(-7.51199928712024,0.724543022591976,
11.976231255802));
#13769=CARTESIAN_POINT('Ctrl Pts',(-7.35822688079632,0.444367128061392,
11.9642280690127));
#13770=CARTESIAN_POINT('Ctrl Pts',(-7.32102560975816,0.14797985599023,11.9522248822234));
#13771=CARTESIAN_POINT('Ctrl Pts',(-7.28382433872001,-0.148407416080933,
11.940221695434));
#13772=CARTESIAN_POINT('Ctrl Pts',(-7.36358464744638,-0.457895344721995,
11.9282185086447));
#13773=CARTESIAN_POINT('Ctrl Pts',(-7.53940549437884,-0.69938318995772,
11.9162153218554));
#13774=CARTESIAN_POINT('Ctrl Pts',(-7.71522634131129,-0.940871035193444,
11.9042121350661));
#13775=CARTESIAN_POINT('Ctrl Pts',(-7.98526240565784,-1.11182427083082,
11.8922089482768));
#13776=CARTESIAN_POINT('Ctrl Pts',(-8.27875123560116,-1.16744491727747,
11.8802057614875));
#13777=CARTESIAN_POINT('Ctrl Pts',(-8.57224006554447,-1.22306556372411,
11.8682025746981));
#13778=CARTESIAN_POINT('Ctrl Pts',(-8.88610136059937,-1.16276985667025,
11.8561993879088));
#13779=CARTESIAN_POINT('Ctrl Pts',(-9.1380883482009,-1.00235817476352,11.8441962011195));
#13780=CARTESIAN_POINT('Ctrl Pts',(-9.39007533580243,-0.841946492856783,
11.8321930143302));
#13781=CARTESIAN_POINT('Ctrl Pts',(-9.57754329642133,-0.583102430602978,
11.8201898275409));
#13782=CARTESIAN_POINT('Ctrl Pts',(-9.65136659729189,-0.293655596346298,
11.8081866407515));
#13783=CARTESIAN_POINT('Ctrl Pts',(-9.67581103310544,-0.197813707972497,
11.8042121350661));
#13784=CARTESIAN_POINT('Ctrl Pts',(-9.68822500000002,-0.0989100500922825,
11.8002376293806));
#13785=CARTESIAN_POINT('Ctrl Pts',(-9.688225,2.06501482580279E-13,11.7962631236952));
#13786=CARTESIAN_POINT('Ctrl Pts',(-9.688225,-1.54454227185852E-12,11.7537368763049));
#13787=CARTESIAN_POINT('Ctrl Pts',(-9.68822499999961,-0.298712821307638,
11.7657400630942));
#13788=CARTESIAN_POINT('Ctrl Pts',(-9.57054245632509,-0.59585807827292,
11.7777432498835));
#13789=CARTESIAN_POINT('Ctrl Pts',(-9.36601586214829,-0.813569405233845,
11.7897464366729));
#13790=CARTESIAN_POINT('Ctrl Pts',(-9.1614892679715,-1.03128073219477,11.8017496234622));
#13791=CARTESIAN_POINT('Ctrl Pts',(-8.87226522412695,-1.16727314847184,
11.8137528102515));
#13792=CARTESIAN_POINT('Ctrl Pts',(-8.57413435701296,-1.185910092602,11.8257559970408));
#13793=CARTESIAN_POINT('Ctrl Pts',(-8.27600348989898,-1.20454703673215,
11.8377591838301));
#13794=CARTESIAN_POINT('Ctrl Pts',(-7.97209482031952,-1.10563290540042,
11.8497623706194));
#13795=CARTESIAN_POINT('Ctrl Pts',(-7.74204705371944,-0.915087963995605,
11.8617655574088));
#13796=CARTESIAN_POINT('Ctrl Pts',(-7.51199928711937,-0.724543022590794,
11.8737687441981));
#13797=CARTESIAN_POINT('Ctrl Pts',(-7.35822688079578,-0.444367128060013,
11.8857719309874));
#13798=CARTESIAN_POINT('Ctrl Pts',(-7.32102560975798,-0.147979855988794,
11.8977751177767));
#13799=CARTESIAN_POINT('Ctrl Pts',(-7.28382433872019,0.148407416082425,
11.909778304566));
#13800=CARTESIAN_POINT('Ctrl Pts',(-7.36358464744695,0.457895344723403,
11.9217814913554));
#13801=CARTESIAN_POINT('Ctrl Pts',(-7.53940549437971,0.699383189958917,
11.9337846781447));
#13802=CARTESIAN_POINT('Ctrl Pts',(-7.71522634131247,0.940871035194431,
11.945787864934));
#13803=CARTESIAN_POINT('Ctrl Pts',(-7.98526240565925,1.11182427083148,11.9577910517233));
#13804=CARTESIAN_POINT('Ctrl Pts',(-8.27875123560265,1.16744491727775,11.9697942385126));
#13805=CARTESIAN_POINT('Ctrl Pts',(-8.57224006554604,1.22306556372402,11.9817974253019));
#13806=CARTESIAN_POINT('Ctrl Pts',(-8.88610136060088,1.16276985666975,11.9938006120913));
#13807=CARTESIAN_POINT('Ctrl Pts',(-9.13808834820221,1.00235817476268,12.0058037988806));
#13808=CARTESIAN_POINT('Ctrl Pts',(-9.39007533580353,0.841946492855617,
12.0178069856699));
#13809=CARTESIAN_POINT('Ctrl Pts',(-9.5775432964221,0.583102430601553,12.0298101724592));
#13810=CARTESIAN_POINT('Ctrl Pts',(-9.65136659729228,0.293655596344764,
12.0418133592485));
#13811=CARTESIAN_POINT('Ctrl Pts',(-9.67581103310568,0.197813707971018,
12.045787864934));
#13812=CARTESIAN_POINT('Ctrl Pts',(-9.68822500000013,0.0989100500908801,
12.0497623706194));
#13813=CARTESIAN_POINT('Ctrl Pts',(-9.688225,-1.51884060883845E-12,12.0537368763049));
#13814=CARTESIAN_POINT('Origin',(-8.5,0.,1.8));
#13815=CARTESIAN_POINT('',(-9.68878804160158,0.000373206645753347,12.3962631236952));
#13816=CARTESIAN_POINT('',(-9.688225,-1.49330547927207E-12,12.3537368763049));
#13817=CARTESIAN_POINT('',(-9.688225,-1.45515594291686E-16,1.8));
#13818=CARTESIAN_POINT('Ctrl Pts',(-9.688225,2.23931984066894E-13,12.3962631236952));
#13819=CARTESIAN_POINT('Ctrl Pts',(-9.68822499999994,0.298712821306317,
12.3842599369059));
#13820=CARTESIAN_POINT('Ctrl Pts',(-9.57054245632575,0.595858078271731,
12.3722567501165));
#13821=CARTESIAN_POINT('Ctrl Pts',(-9.3660158621492,0.813569405232883,12.3602535633272));
#13822=CARTESIAN_POINT('Ctrl Pts',(-9.16148926797264,1.03128073219403,12.3482503765379));
#13823=CARTESIAN_POINT('Ctrl Pts',(-8.87226522412824,1.16727314847143,12.3362471897486));
#13824=CARTESIAN_POINT('Ctrl Pts',(-8.57413435701428,1.18591009260191,12.3242440029593));
#13825=CARTESIAN_POINT('Ctrl Pts',(-8.27600348990032,1.2045470367324,12.3122408161699));
#13826=CARTESIAN_POINT('Ctrl Pts',(-7.97209482032075,1.105632905401,12.3002376293806));
#13827=CARTESIAN_POINT('Ctrl Pts',(-7.74204705372046,0.915087963996447,
12.2882344425913));
#13828=CARTESIAN_POINT('Ctrl Pts',(-7.51199928712017,0.724543022591892,
12.276231255802));
#13829=CARTESIAN_POINT('Ctrl Pts',(-7.35822688079627,0.444367128061282,
12.2642280690127));
#13830=CARTESIAN_POINT('Ctrl Pts',(-7.32102560975815,0.147979855990104,
12.2522248822234));
#13831=CARTESIAN_POINT('Ctrl Pts',(-7.28382433872002,-0.148407416081074,
12.240221695434));
#13832=CARTESIAN_POINT('Ctrl Pts',(-7.36358464744644,-0.45789534472214,
12.2282185086447));
#13833=CARTESIAN_POINT('Ctrl Pts',(-7.53940549437893,-0.69938318995785,
12.2162153218554));
#13834=CARTESIAN_POINT('Ctrl Pts',(-7.71522634131143,-0.940871035193559,
12.2042121350661));
#13835=CARTESIAN_POINT('Ctrl Pts',(-7.98526240565801,-1.1118242708309,12.1922089482768));
#13836=CARTESIAN_POINT('Ctrl Pts',(-8.27875123560135,-1.1674449172775,12.1802057614874));
#13837=CARTESIAN_POINT('Ctrl Pts',(-8.57224006554469,-1.2230655637241,12.1682025746981));
#13838=CARTESIAN_POINT('Ctrl Pts',(-8.88610136059958,-1.16276985667018,
12.1561993879088));
#13839=CARTESIAN_POINT('Ctrl Pts',(-9.13808834820109,-1.00235817476339,
12.1441962011195));
#13840=CARTESIAN_POINT('Ctrl Pts',(-9.3900753358026,-0.841946492856606,
12.1321930143302));
#13841=CARTESIAN_POINT('Ctrl Pts',(-9.57754329642145,-0.583102430602751,
12.1201898275409));
#13842=CARTESIAN_POINT('Ctrl Pts',(-9.65136659729195,-0.293655596346044,
12.1081866407515));
#13843=CARTESIAN_POINT('Ctrl Pts',(-9.67581103310546,-0.197813707972314,
12.1042121350661));
#13844=CARTESIAN_POINT('Ctrl Pts',(-9.68822500000002,-0.098910050092178,
12.1002376293806));
#13845=CARTESIAN_POINT('Ctrl Pts',(-9.688225,2.3214763444912E-13,12.0962631236952));
#13846=CARTESIAN_POINT('Ctrl Pts',(-9.688225,-1.51884060883845E-12,12.0537368763049));
#13847=CARTESIAN_POINT('Ctrl Pts',(-9.68822499999962,-0.298712821307624,
12.0657400630942));
#13848=CARTESIAN_POINT('Ctrl Pts',(-9.57054245632509,-0.595858078272919,
12.0777432498835));
#13849=CARTESIAN_POINT('Ctrl Pts',(-9.36601586214829,-0.813569405233851,
12.0897464366729));
#13850=CARTESIAN_POINT('Ctrl Pts',(-9.16148926797148,-1.03128073219478,
12.1017496234622));
#13851=CARTESIAN_POINT('Ctrl Pts',(-8.87226522412692,-1.16727314847185,
12.1137528102515));
#13852=CARTESIAN_POINT('Ctrl Pts',(-8.57413435701292,-1.185910092602,12.1257559970408));
#13853=CARTESIAN_POINT('Ctrl Pts',(-8.27600348989893,-1.20454703673215,
12.1377591838301));
#13854=CARTESIAN_POINT('Ctrl Pts',(-7.97209482031946,-1.10563290540039,
12.1497623706194));
#13855=CARTESIAN_POINT('Ctrl Pts',(-7.74204705371938,-0.915087963995556,
12.1617655574088));
#13856=CARTESIAN_POINT('Ctrl Pts',(-7.51199928711931,-0.724543022590723,
12.1737687441981));
#13857=CARTESIAN_POINT('Ctrl Pts',(-7.35822688079574,-0.444367128059919,
12.1857719309874));
#13858=CARTESIAN_POINT('Ctrl Pts',(-7.32102560975797,-0.147979855988685,
12.1977751177767));
#13859=CARTESIAN_POINT('Ctrl Pts',(-7.2838243387202,0.148407416082549,12.209778304566));
#13860=CARTESIAN_POINT('Ctrl Pts',(-7.36358464744699,0.457895344723531,
12.2217814913554));
#13861=CARTESIAN_POINT('Ctrl Pts',(-7.53940549437979,0.699383189959033,
12.2337846781447));
#13862=CARTESIAN_POINT('Ctrl Pts',(-7.71522634131259,0.940871035194535,
12.245787864934));
#13863=CARTESIAN_POINT('Ctrl Pts',(-7.9852624056594,1.11182427083155,12.2577910517233));
#13864=CARTESIAN_POINT('Ctrl Pts',(-8.27875123560282,1.16744491727778,12.2697942385126));
#13865=CARTESIAN_POINT('Ctrl Pts',(-8.57224006554624,1.22306556372401,12.2817974253019));
#13866=CARTESIAN_POINT('Ctrl Pts',(-8.88610136060107,1.16276985666969,12.2938006120913));
#13867=CARTESIAN_POINT('Ctrl Pts',(-9.13808834820238,1.00235817476257,12.3058037988806));
#13868=CARTESIAN_POINT('Ctrl Pts',(-9.39007533580369,0.841946492855453,
12.3178069856699));
#13869=CARTESIAN_POINT('Ctrl Pts',(-9.57754329642222,0.583102430601342,
12.3298101724592));
#13870=CARTESIAN_POINT('Ctrl Pts',(-9.65136659729234,0.293655596344527,
12.3418133592485));
#13871=CARTESIAN_POINT('Ctrl Pts',(-9.6758110331057,0.197813707970863,12.345787864934));
#13872=CARTESIAN_POINT('Ctrl Pts',(-9.68822500000012,0.0989100500908155,
12.3497623706194));
#13873=CARTESIAN_POINT('Ctrl Pts',(-9.688225,-1.49330547927207E-12,12.3537368763049));
#13874=CARTESIAN_POINT('Origin',(-8.5,0.,1.8));
#13875=CARTESIAN_POINT('',(-9.68731827199145,0.000299612246693184,12.6962631236952));
#13876=CARTESIAN_POINT('',(-9.688225,-1.46765932740323E-12,12.6537368763049));
#13877=CARTESIAN_POINT('',(-9.688225,-1.45515594291686E-16,1.8));
#13878=CARTESIAN_POINT('Ctrl Pts',(-9.68662866502971,0.000527480679553827,
12.6962631236952));
#13879=CARTESIAN_POINT('Ctrl Pts',(-9.68740960275973,0.161591526755359,
12.6898105777584));
#13880=CARTESIAN_POINT('Ctrl Pts',(-9.65693800757816,0.322407861474271,
12.6833580318217));
#13881=CARTESIAN_POINT('Ctrl Pts',(-9.59386268769377,0.469313525857254,
12.676905485885));
#13882=CARTESIAN_POINT('Ctrl Pts',(-9.43836427799808,0.831477320328926,
12.6609981447334));
#13883=CARTESIAN_POINT('Ctrl Pts',(-9.08471307556792,1.10909745603158,12.6450908035818));
#13884=CARTESIAN_POINT('Ctrl Pts',(-8.69629196213472,1.17401378965972,12.6291834624301));
#13885=CARTESIAN_POINT('Ctrl Pts',(-8.30787084870153,1.23893012328785,12.6132761212785));
#13886=CARTESIAN_POINT('Ctrl Pts',(-7.88467982426531,1.09114265484149,12.5973687801269));
#13887=CARTESIAN_POINT('Ctrl Pts',(-7.6190606764032,0.799649543688172,12.5814614389753));
#13888=CARTESIAN_POINT('Ctrl Pts',(-7.48625110247213,0.653902988111497,
12.5735077683995));
#13889=CARTESIAN_POINT('Ctrl Pts',(-7.39283449768459,0.472230021858075,
12.5655540978237));
#13890=CARTESIAN_POINT('Ctrl Pts',(-7.34613116947634,0.279251812905948,
12.5576004272478));
#13891=CARTESIAN_POINT('Ctrl Pts',(-7.29942784126808,0.0862736039538323,
12.549646756672));
#13892=CARTESIAN_POINT('Ctrl Pts',(-7.2994377896391,-0.118009847696987,
12.5416930860962));
#13893=CARTESIAN_POINT('Ctrl Pts',(-7.35090869635395,-0.308354763973108,
12.5337394155204));
#13894=CARTESIAN_POINT('Ctrl Pts',(-7.45385050978364,-0.689044596525339,
12.5178320743688));
#13895=CARTESIAN_POINT('Ctrl Pts',(-7.76263615658864,-1.01398028757878,
12.5019247332172));
#13896=CARTESIAN_POINT('Ctrl Pts',(-8.13775744624663,-1.13385150921984,
12.4860173920656));
#13897=CARTESIAN_POINT('Ctrl Pts',(-8.51287873590465,-1.2537227308609,12.4701100509139));
#13898=CARTESIAN_POINT('Ctrl Pts',(-8.95433566841568,-1.16852948308955,
12.4542027097623));
#13899=CARTESIAN_POINT('Ctrl Pts',(-9.25822456392514,-0.917543609722033,
12.4382953686107));
#13900=CARTESIAN_POINT('Ctrl Pts',(-9.52588153985455,-0.696482159767021,
12.4242846203055));
#13901=CARTESIAN_POINT('Ctrl Pts',(-9.6868187133487,-0.346805396004457,
12.4102738720003));
#13902=CARTESIAN_POINT('Ctrl Pts',(-9.68938150757543,0.000766579790317107,
12.3962631236952));
#13903=CARTESIAN_POINT('Ctrl Pts',(-9.688225,-1.49330547927207E-12,12.3537368763049));
#13904=CARTESIAN_POINT('Ctrl Pts',(-9.68822499999962,-0.298712821307587,
12.3657400630942));
#13905=CARTESIAN_POINT('Ctrl Pts',(-9.57054245632511,-0.595858078272874,
12.3777432498835));
#13906=CARTESIAN_POINT('Ctrl Pts',(-9.36601586214833,-0.813569405233808,
12.3897464366729));
#13907=CARTESIAN_POINT('Ctrl Pts',(-9.16148926797154,-1.03128073219474,
12.4017496234622));
#13908=CARTESIAN_POINT('Ctrl Pts',(-8.872265224127,-1.16727314847182,12.4137528102515));
#13909=CARTESIAN_POINT('Ctrl Pts',(-8.57413435701301,-1.18591009260199,
12.4257559970408));
#13910=CARTESIAN_POINT('Ctrl Pts',(-8.27600348989903,-1.20454703673216,
12.4377591838301));
#13911=CARTESIAN_POINT('Ctrl Pts',(-7.97209482031957,-1.10563290540044,
12.4497623706194));
#13912=CARTESIAN_POINT('Ctrl Pts',(-7.74204705371948,-0.915087963995637,
12.4617655574088));
#13913=CARTESIAN_POINT('Ctrl Pts',(-7.5119992871194,-0.724543022590836,
12.4737687441981));
#13914=CARTESIAN_POINT('Ctrl Pts',(-7.3582268807958,-0.444367128060062,
12.4857719309874));
#13915=CARTESIAN_POINT('Ctrl Pts',(-7.32102560975799,-0.147979855988844,
12.4977751177767));
#13916=CARTESIAN_POINT('Ctrl Pts',(-7.28382433872018,0.148407416082373,
12.509778304566));
#13917=CARTESIAN_POINT('Ctrl Pts',(-7.36358464744693,0.457895344723354,
12.5217814913554));
#13918=CARTESIAN_POINT('Ctrl Pts',(-7.53940549437968,0.699383189958875,
12.5337846781447));
#13919=CARTESIAN_POINT('Ctrl Pts',(-7.71522634131243,0.940871035194397,
12.545787864934));
#13920=CARTESIAN_POINT('Ctrl Pts',(-7.9852624056592,1.11182427083145,12.5577910517233));
#13921=CARTESIAN_POINT('Ctrl Pts',(-8.2787512356026,1.16744491727774,12.5697942385126));
#13922=CARTESIAN_POINT('Ctrl Pts',(-8.57224006554599,1.22306556372402,12.5817974253019));
#13923=CARTESIAN_POINT('Ctrl Pts',(-8.88610136060083,1.16276985666977,12.5938006120913));
#13924=CARTESIAN_POINT('Ctrl Pts',(-9.13808834820216,1.00235817476271,12.6058037988806));
#13925=CARTESIAN_POINT('Ctrl Pts',(-9.3900753358035,0.841946492855655,12.6178069856699));
#13926=CARTESIAN_POINT('Ctrl Pts',(-9.57754329642207,0.5831024306016,12.6298101724592));
#13927=CARTESIAN_POINT('Ctrl Pts',(-9.65136659729227,0.293655596344814,
12.6418133592485));
#13928=CARTESIAN_POINT('Ctrl Pts',(-9.67581103310567,0.19781370797108,12.645787864934));
#13929=CARTESIAN_POINT('Ctrl Pts',(-9.68822500000012,0.0989100500909537,
12.6497623706194));
#13930=CARTESIAN_POINT('Ctrl Pts',(-9.688225,-1.43385303630339E-12,12.6537368763049));
#13931=CARTESIAN_POINT('Origin',(-8.5,0.,1.8));
#13932=CARTESIAN_POINT('',(-9.688225,3.08975067753181E-13,12.9962631236952));
#13933=CARTESIAN_POINT('',(-9.688225,-1.44201317553438E-12,12.9537368763049));
#13934=CARTESIAN_POINT('',(-9.688225,-1.45515594291686E-16,1.8));
#13935=CARTESIAN_POINT('Ctrl Pts',(-9.688225,3.42836870004248E-13,12.9962631236952));
#13936=CARTESIAN_POINT('Ctrl Pts',(-9.68822499999991,0.298712821306448,
12.9842599369058));
#13937=CARTESIAN_POINT('Ctrl Pts',(-9.57054245632568,0.59585807827186,12.9722567501165));
#13938=CARTESIAN_POINT('Ctrl Pts',(-9.36601586214909,0.813569405232994,
12.9602535633272));
#13939=CARTESIAN_POINT('Ctrl Pts',(-9.1614892679725,1.03128073219413,12.9482503765379));
#13940=CARTESIAN_POINT('Ctrl Pts',(-8.87226522412807,1.16727314847148,12.9362471897486));
#13941=CARTESIAN_POINT('Ctrl Pts',(-8.57413435701409,1.18591009260193,12.9242440029593));
#13942=CARTESIAN_POINT('Ctrl Pts',(-8.27600348990012,1.20454703673237,12.9122408161699));
#13943=CARTESIAN_POINT('Ctrl Pts',(-7.97209482032055,1.10563290540091,12.9002376293806));
#13944=CARTESIAN_POINT('Ctrl Pts',(-7.74204705372029,0.915087963996307,
12.8882344425913));
#13945=CARTESIAN_POINT('Ctrl Pts',(-7.51199928712003,0.724543022591702,
12.876231255802));
#13946=CARTESIAN_POINT('Ctrl Pts',(-7.35822688079618,0.444367128061049,
12.8642280690127));
#13947=CARTESIAN_POINT('Ctrl Pts',(-7.32102560975812,0.147979855989852,
12.8522248822233));
#13948=CARTESIAN_POINT('Ctrl Pts',(-7.28382433872005,-0.148407416081345,
12.840221695434));
#13949=CARTESIAN_POINT('Ctrl Pts',(-7.36358464744654,-0.457895344722406,
12.8282185086447));
#13950=CARTESIAN_POINT('Ctrl Pts',(-7.5394054943791,-0.699383189958082,
12.8162153218554));
#13951=CARTESIAN_POINT('Ctrl Pts',(-7.71522634131166,-0.940871035193758,
12.8042121350661));
#13952=CARTESIAN_POINT('Ctrl Pts',(-7.9852624056583,-1.11182427083104,12.7922089482768));
#13953=CARTESIAN_POINT('Ctrl Pts',(-8.27875123560167,-1.16744491727756,
12.7802057614874));
#13954=CARTESIAN_POINT('Ctrl Pts',(-8.57224006554503,-1.22306556372408,
12.7682025746981));
#13955=CARTESIAN_POINT('Ctrl Pts',(-8.88610136059992,-1.16276985667007,
12.7561993879088));
#13956=CARTESIAN_POINT('Ctrl Pts',(-9.13808834820139,-1.0023581747632,12.7441962011195));
#13957=CARTESIAN_POINT('Ctrl Pts',(-9.39007533580286,-0.841946492856334,
12.7321930143302));
#13958=CARTESIAN_POINT('Ctrl Pts',(-9.57754329642164,-0.583102430602409,
12.7201898275408));
#13959=CARTESIAN_POINT('Ctrl Pts',(-9.65136659729205,-0.293655596345667,
12.7081866407515));
#13960=CARTESIAN_POINT('Ctrl Pts',(-9.6758110331055,-0.197813707972038,
12.7042121350661));
#13961=CARTESIAN_POINT('Ctrl Pts',(-9.68822500000002,-0.0989100500920141,
12.7002376293806));
#13962=CARTESIAN_POINT('Ctrl Pts',(-9.688225,2.83439938186802E-13,12.6962631236952));
#13963=CARTESIAN_POINT('Ctrl Pts',(-9.688225,-1.43385303630339E-12,12.6537368763049));
#13964=CARTESIAN_POINT('Ctrl Pts',(-9.68822499999964,-0.298712821307539,
12.6657400630942));
#13965=CARTESIAN_POINT('Ctrl Pts',(-9.57054245632513,-0.595858078272843,
12.6777432498835));
#13966=CARTESIAN_POINT('Ctrl Pts',(-9.36601586214834,-0.813569405233789,
12.6897464366729));
#13967=CARTESIAN_POINT('Ctrl Pts',(-9.16148926797156,-1.03128073219474,
12.7017496234622));
#13968=CARTESIAN_POINT('Ctrl Pts',(-8.872265224127,-1.16727314847183,12.7137528102515));
#13969=CARTESIAN_POINT('Ctrl Pts',(-8.574134357013,-1.18591009260199,12.7257559970408));
#13970=CARTESIAN_POINT('Ctrl Pts',(-8.27600348989901,-1.20454703673216,
12.7377591838301));
#13971=CARTESIAN_POINT('Ctrl Pts',(-7.97209482031954,-1.10563290540043,
12.7497623706194));
#13972=CARTESIAN_POINT('Ctrl Pts',(-7.74204705371945,-0.91508796399561,
12.7617655574088));
#13973=CARTESIAN_POINT('Ctrl Pts',(-7.51199928711936,-0.724543022590794,
12.7737687441981));
#13974=CARTESIAN_POINT('Ctrl Pts',(-7.35822688079577,-0.44436712806,12.7857719309874));
#13975=CARTESIAN_POINT('Ctrl Pts',(-7.32102560975798,-0.147979855988769,
12.7977751177767));
#13976=CARTESIAN_POINT('Ctrl Pts',(-7.28382433872019,0.148407416082461,
12.809778304566));
#13977=CARTESIAN_POINT('Ctrl Pts',(-7.36358464744696,0.457895344723449,
12.8217814913554));
#13978=CARTESIAN_POINT('Ctrl Pts',(-7.53940549437974,0.699383189958964,
12.8337846781447));
#13979=CARTESIAN_POINT('Ctrl Pts',(-7.71522634131253,0.940871035194479,
12.845787864934));
#13980=CARTESIAN_POINT('Ctrl Pts',(-7.98526240565932,1.11182427083151,12.8577910517233));
#13981=CARTESIAN_POINT('Ctrl Pts',(-8.27875123560274,1.16744491727776,12.8697942385126));
#13982=CARTESIAN_POINT('Ctrl Pts',(-8.57224006554615,1.22306556372401,12.8817974253019));
#13983=CARTESIAN_POINT('Ctrl Pts',(-8.88610136060099,1.16276985666972,12.8938006120913));
#13984=CARTESIAN_POINT('Ctrl Pts',(-9.13808834820231,1.00235817476262,12.9058037988806));
#13985=CARTESIAN_POINT('Ctrl Pts',(-9.39007533580363,0.841946492855517,
12.9178069856699));
#13986=CARTESIAN_POINT('Ctrl Pts',(-9.57754329642218,0.583102430601419,
12.9298101724592));
#13987=CARTESIAN_POINT('Ctrl Pts',(-9.65136659729232,0.293655596344609,
12.9418133592485));
#13988=CARTESIAN_POINT('Ctrl Pts',(-9.67581103310568,0.197813707970937,
12.945787864934));
#13989=CARTESIAN_POINT('Ctrl Pts',(-9.68822500000012,0.098910050090878,
12.9497623706194));
#13990=CARTESIAN_POINT('Ctrl Pts',(-9.688225,-1.44201317553438E-12,12.9537368763049));
#13991=CARTESIAN_POINT('Origin',(-8.5,0.,1.8));
#13992=CARTESIAN_POINT('',(-9.688225,3.34621219622022E-13,13.2962631236952));
#13993=CARTESIAN_POINT('',(-9.688225,-1.41642253481677E-12,13.2537368763049));
#13994=CARTESIAN_POINT('',(-9.688225,-1.45515594291686E-16,1.8));
#13995=CARTESIAN_POINT('Ctrl Pts',(-9.688225,3.34621219622022E-13,13.2962631236952));
#13996=CARTESIAN_POINT('Ctrl Pts',(-9.68822499999992,0.298712821306428,
13.2842599369058));
#13997=CARTESIAN_POINT('Ctrl Pts',(-9.57054245632569,0.59585807827183,13.2722567501165));
#13998=CARTESIAN_POINT('Ctrl Pts',(-9.36601586214912,0.813569405232963,
13.2602535633272));
#13999=CARTESIAN_POINT('Ctrl Pts',(-9.16148926797255,1.0312807321941,13.2482503765379));
#14000=CARTESIAN_POINT('Ctrl Pts',(-8.87226522412814,1.16727314847146,13.2362471897486));
#14001=CARTESIAN_POINT('Ctrl Pts',(-8.57413435701417,1.18591009260192,13.2242440029593));
#14002=CARTESIAN_POINT('Ctrl Pts',(-8.27600348990021,1.20454703673238,13.2122408161699));
#14003=CARTESIAN_POINT('Ctrl Pts',(-7.97209482032064,1.10563290540095,13.2002376293806));
#14004=CARTESIAN_POINT('Ctrl Pts',(-7.74204705372037,0.915087963996377,
13.1882344425913));
#14005=CARTESIAN_POINT('Ctrl Pts',(-7.5119992871201,0.7245430225918,13.176231255802));
#14006=CARTESIAN_POINT('Ctrl Pts',(-7.35822688079623,0.444367128061175,
13.1642280690127));
#14007=CARTESIAN_POINT('Ctrl Pts',(-7.32102560975813,0.147979855989994,
13.1522248822233));
#14008=CARTESIAN_POINT('Ctrl Pts',(-7.28382433872004,-0.148407416081187,
13.140221695434));
#14009=CARTESIAN_POINT('Ctrl Pts',(-7.36358464744648,-0.457895344722246,
13.1282185086447));
#14010=CARTESIAN_POINT('Ctrl Pts',(-7.539405494379,-0.699383189957939,13.1162153218554));
#14011=CARTESIAN_POINT('Ctrl Pts',(-7.71522634131152,-0.940871035193632,
13.1042121350661));
#14012=CARTESIAN_POINT('Ctrl Pts',(-7.98526240565812,-1.11182427083095,
13.0922089482768));
#14013=CARTESIAN_POINT('Ctrl Pts',(-8.27875123560146,-1.16744491727752,
13.0802057614874));
#14014=CARTESIAN_POINT('Ctrl Pts',(-8.5722400655448,-1.22306556372409,13.0682025746981));
#14015=CARTESIAN_POINT('Ctrl Pts',(-8.88610136059969,-1.16276985667015,
13.0561993879088));
#14016=CARTESIAN_POINT('Ctrl Pts',(-9.13808834820118,-1.00235817476333,
13.0441962011195));
#14017=CARTESIAN_POINT('Ctrl Pts',(-9.39007533580268,-0.841946492856523,
13.0321930143302));
#14018=CARTESIAN_POINT('Ctrl Pts',(-9.57754329642151,-0.583102430602651,
13.0201898275409));
#14019=CARTESIAN_POINT('Ctrl Pts',(-9.65136659729198,-0.293655596345937,
13.0081866407515));
#14020=CARTESIAN_POINT('Ctrl Pts',(-9.67581103310548,-0.197813707972205,
13.0042121350661));
#14021=CARTESIAN_POINT('Ctrl Pts',(-9.68822500000003,-0.0989100500920673,
13.0002376293806));
#14022=CARTESIAN_POINT('Ctrl Pts',(-9.688225,3.42836870004248E-13,12.9962631236952));
#14023=CARTESIAN_POINT('Ctrl Pts',(-9.688225,-1.44201317553438E-12,12.9537368763049));
#14024=CARTESIAN_POINT('Ctrl Pts',(-9.68822499999964,-0.298712821307535,
12.9657400630942));
#14025=CARTESIAN_POINT('Ctrl Pts',(-9.57054245632514,-0.595858078272828,
12.9777432498835));
#14026=CARTESIAN_POINT('Ctrl Pts',(-9.36601586214836,-0.81356940523377,
12.9897464366729));
#14027=CARTESIAN_POINT('Ctrl Pts',(-9.16148926797158,-1.03128073219471,
13.0017496234622));
#14028=CARTESIAN_POINT('Ctrl Pts',(-8.87226522412705,-1.16727314847181,
13.0137528102515));
#14029=CARTESIAN_POINT('Ctrl Pts',(-8.57413435701307,-1.18591009260199,
13.0257559970408));
#14030=CARTESIAN_POINT('Ctrl Pts',(-8.27600348989908,-1.20454703673217,
13.0377591838301));
#14031=CARTESIAN_POINT('Ctrl Pts',(-7.97209482031961,-1.10563290540046,
13.0497623706194));
#14032=CARTESIAN_POINT('Ctrl Pts',(-7.74204705371952,-0.91508796399567,
13.0617655574088));
#14033=CARTESIAN_POINT('Ctrl Pts',(-7.51199928711943,-0.724543022590879,
13.0737687441981));
#14034=CARTESIAN_POINT('Ctrl Pts',(-7.35822688079581,-0.444367128060111,
13.0857719309874));
#14035=CARTESIAN_POINT('Ctrl Pts',(-7.321025609758,-0.147979855988895,13.0977751177767));
#14036=CARTESIAN_POINT('Ctrl Pts',(-7.28382433872018,0.14840741608232,13.109778304566));
#14037=CARTESIAN_POINT('Ctrl Pts',(-7.36358464744691,0.457895344723305,
13.1217814913553));
#14038=CARTESIAN_POINT('Ctrl Pts',(-7.53940549437965,0.699383189958834,
13.1337846781447));
#14039=CARTESIAN_POINT('Ctrl Pts',(-7.71522634131239,0.940871035194364,
13.145787864934));
#14040=CARTESIAN_POINT('Ctrl Pts',(-7.98526240565915,1.11182427083143,13.1577910517233));
#14041=CARTESIAN_POINT('Ctrl Pts',(-8.27875123560255,1.16744491727773,13.1697942385126));
#14042=CARTESIAN_POINT('Ctrl Pts',(-8.57224006554594,1.22306556372402,13.1817974253019));
#14043=CARTESIAN_POINT('Ctrl Pts',(-8.88610136060078,1.16276985666979,13.1938006120913));
#14044=CARTESIAN_POINT('Ctrl Pts',(-9.13808834820212,1.00235817476274,13.2058037988806));
#14045=CARTESIAN_POINT('Ctrl Pts',(-9.39007533580346,0.841946492855694,
13.2178069856699));
#14046=CARTESIAN_POINT('Ctrl Pts',(-9.57754329642205,0.583102430601646,
13.2298101724592));
#14047=CARTESIAN_POINT('Ctrl Pts',(-9.65136659729225,0.293655596344863,
13.2418133592485));
#14048=CARTESIAN_POINT('Ctrl Pts',(-9.67581103310566,0.19781370797112,13.245787864934));
#14049=CARTESIAN_POINT('Ctrl Pts',(-9.68822500000012,0.0989100500909825,
13.2497623706194));
#14050=CARTESIAN_POINT('Ctrl Pts',(-9.688225,-1.41642253481677E-12,13.2537368763049));
#14051=CARTESIAN_POINT('Origin',(-8.5,0.,1.8));
#14052=CARTESIAN_POINT('',(-9.688225,3.60267371490863E-13,13.5962631236952));
#14053=CARTESIAN_POINT('',(-9.688225,-1.39083189409916E-12,13.5537368763049));
#14054=CARTESIAN_POINT('',(-9.688225,-1.45515594291686E-16,1.8));
#14055=CARTESIAN_POINT('Ctrl Pts',(-9.688225,3.93907129137006E-13,13.5962631236952));
#14056=CARTESIAN_POINT('Ctrl Pts',(-9.6882249999999,0.29871282130651,13.5842599369058));
#14057=CARTESIAN_POINT('Ctrl Pts',(-9.57054245632564,0.595858078271928,
13.5722567501165));
#14058=CARTESIAN_POINT('Ctrl Pts',(-9.36601586214903,0.813569405233056,
13.5602535633272));
#14059=CARTESIAN_POINT('Ctrl Pts',(-9.16148926797242,1.03128073219418,13.5482503765379));
#14060=CARTESIAN_POINT('Ctrl Pts',(-8.87226522412797,1.16727314847152,13.5362471897486));
#14061=CARTESIAN_POINT('Ctrl Pts',(-8.57413435701398,1.18591009260193,13.5242440029592));
#14062=CARTESIAN_POINT('Ctrl Pts',(-8.27600348989999,1.20454703673235,13.5122408161699));
#14063=CARTESIAN_POINT('Ctrl Pts',(-7.97209482032042,1.10563290540085,13.5002376293806));
#14064=CARTESIAN_POINT('Ctrl Pts',(-7.74204705372017,0.91508796399621,13.4882344425913));
#14065=CARTESIAN_POINT('Ctrl Pts',(-7.51199928711992,0.724543022591568,
13.476231255802));
#14066=CARTESIAN_POINT('Ctrl Pts',(-7.35822688079611,0.444367128060881,
13.4642280690127));
#14067=CARTESIAN_POINT('Ctrl Pts',(-7.32102560975809,0.147979855989667,
13.4522248822233));
#14068=CARTESIAN_POINT('Ctrl Pts',(-7.28382433872008,-0.148407416081547,
13.440221695434));
#14069=CARTESIAN_POINT('Ctrl Pts',(-7.36358464744662,-0.457895344722607,
13.4282185086447));
#14070=CARTESIAN_POINT('Ctrl Pts',(-7.53940549437923,-0.69938318995826,
13.4162153218554));
#14071=CARTESIAN_POINT('Ctrl Pts',(-7.71522634131184,-0.940871035193913,
13.4042121350661));
#14072=CARTESIAN_POINT('Ctrl Pts',(-7.98526240565853,-1.11182427083115,
13.3922089482767));
#14073=CARTESIAN_POINT('Ctrl Pts',(-8.27875123560191,-1.16744491727761,
13.3802057614874));
#14074=CARTESIAN_POINT('Ctrl Pts',(-8.5722400655453,-1.22306556372407,13.3682025746981));
#14075=CARTESIAN_POINT('Ctrl Pts',(-8.8861013606002,-1.16276985666999,13.3561993879088));
#14076=CARTESIAN_POINT('Ctrl Pts',(-9.13808834820163,-1.00235817476305,
13.3441962011195));
#14077=CARTESIAN_POINT('Ctrl Pts',(-9.39007533580307,-0.841946492856113,
13.3321930143301));
#14078=CARTESIAN_POINT('Ctrl Pts',(-9.5775432964218,-0.583102430602129,
13.3201898275408));
#14079=CARTESIAN_POINT('Ctrl Pts',(-9.65136659729213,-0.293655596345355,
13.3081866407515));
#14080=CARTESIAN_POINT('Ctrl Pts',(-9.67581103310553,-0.197813707971808,
13.3042121350661));
#14081=CARTESIAN_POINT('Ctrl Pts',(-9.68822500000003,-0.0989100500918729,
13.3002376293806));
#14082=CARTESIAN_POINT('Ctrl Pts',(-9.688225,3.34621219622022E-13,13.2962631236952));
#14083=CARTESIAN_POINT('Ctrl Pts',(-9.688225,-1.41642253481677E-12,13.2537368763049));
#14084=CARTESIAN_POINT('Ctrl Pts',(-9.68822499999964,-0.298712821307499,
13.2657400630942));
#14085=CARTESIAN_POINT('Ctrl Pts',(-9.57054245632516,-0.595858078272782,
13.2777432498835));
#14086=CARTESIAN_POINT('Ctrl Pts',(-9.3660158621484,-0.813569405233727,
13.2897464366728));
#14087=CARTESIAN_POINT('Ctrl Pts',(-9.16148926797164,-1.03128073219467,
13.3017496234622));
#14088=CARTESIAN_POINT('Ctrl Pts',(-8.87226522412713,-1.16727314847178,
13.3137528102515));
#14089=CARTESIAN_POINT('Ctrl Pts',(-8.57413435701316,-1.18591009260198,
13.3257559970408));
#14090=CARTESIAN_POINT('Ctrl Pts',(-8.27600348989919,-1.20454703673219,
13.3377591838301));
#14091=CARTESIAN_POINT('Ctrl Pts',(-7.97209482031972,-1.10563290540051,
13.3497623706194));
#14092=CARTESIAN_POINT('Ctrl Pts',(-7.74204705371962,-0.915087963995751,
13.3617655574088));
#14093=CARTESIAN_POINT('Ctrl Pts',(-7.51199928711951,-0.724543022590991,
13.3737687441981));
#14094=CARTESIAN_POINT('Ctrl Pts',(-7.35822688079587,-0.444367128060254,
13.3857719309874));
#14095=CARTESIAN_POINT('Ctrl Pts',(-7.32102560975802,-0.147979855989055,
13.3977751177767));
#14096=CARTESIAN_POINT('Ctrl Pts',(-7.28382433872016,0.148407416082145,
13.409778304566));
#14097=CARTESIAN_POINT('Ctrl Pts',(-7.36358464744684,0.457895344723128,
13.4217814913553));
#14098=CARTESIAN_POINT('Ctrl Pts',(-7.53940549437953,0.699383189958677,
13.4337846781447));
#14099=CARTESIAN_POINT('Ctrl Pts',(-7.71522634131223,0.940871035194226,
13.445787864934));
#14100=CARTESIAN_POINT('Ctrl Pts',(-7.98526240565895,1.11182427083133,13.4577910517233));
#14101=CARTESIAN_POINT('Ctrl Pts',(-8.27875123560232,1.16744491727769,13.4697942385126));
#14102=CARTESIAN_POINT('Ctrl Pts',(-8.57224006554569,1.22306556372404,13.4817974253019));
#14103=CARTESIAN_POINT('Ctrl Pts',(-8.88610136060053,1.16276985666987,13.4938006120912));
#14104=CARTESIAN_POINT('Ctrl Pts',(-9.1380883482019,1.00235817476288,13.5058037988806));
#14105=CARTESIAN_POINT('Ctrl Pts',(-9.39007533580327,0.841946492855896,
13.5178069856699));
#14106=CARTESIAN_POINT('Ctrl Pts',(-9.57754329642191,0.583102430601903,
13.5298101724592));
#14107=CARTESIAN_POINT('Ctrl Pts',(-9.65136659729218,0.29365559634515,13.5418133592485));
#14108=CARTESIAN_POINT('Ctrl Pts',(-9.67581103310563,0.197813707971336,
13.545787864934));
#14109=CARTESIAN_POINT('Ctrl Pts',(-9.68822500000011,0.0989100500911206,
13.5497623706194));
#14110=CARTESIAN_POINT('Ctrl Pts',(-9.688225,-1.35702560299933E-12,13.5537368763049));
#14111=CARTESIAN_POINT('Origin',(-8.5,0.,1.8));
#14112=CARTESIAN_POINT('',(-9.688225,3.85913523359704E-13,13.8962631236952));
#14113=CARTESIAN_POINT('',(-9.6873777234388,-0.000235261270365428,13.8537368763049));
#14114=CARTESIAN_POINT('',(-9.688225,-1.45515594291686E-16,1.8));
#14115=CARTESIAN_POINT('Ctrl Pts',(-9.688225,4.53415083256914E-13,13.8962631236952));
#14116=CARTESIAN_POINT('Ctrl Pts',(-9.68822499999989,0.298712821306558,
13.8842599369058));
#14117=CARTESIAN_POINT('Ctrl Pts',(-9.57054245632563,0.595858078271959,
13.8722567501165));
#14118=CARTESIAN_POINT('Ctrl Pts',(-9.36601586214902,0.813569405233075,
13.8602535633272));
#14119=CARTESIAN_POINT('Ctrl Pts',(-9.16148926797241,1.03128073219419,13.8482503765379));
#14120=CARTESIAN_POINT('Ctrl Pts',(-8.87226522412796,1.16727314847152,13.8362471897486));
#14121=CARTESIAN_POINT('Ctrl Pts',(-8.57413435701398,1.18591009260193,13.8242440029592));
#14122=CARTESIAN_POINT('Ctrl Pts',(-8.2760034899,1.20454703673235,13.8122408161699));
#14123=CARTESIAN_POINT('Ctrl Pts',(-7.97209482032045,1.10563290540086,13.8002376293806));
#14124=CARTESIAN_POINT('Ctrl Pts',(-7.7420470537202,0.915087963996236,13.7882344425913));
#14125=CARTESIAN_POINT('Ctrl Pts',(-7.51199928711996,0.72454302259161,13.776231255802));
#14126=CARTESIAN_POINT('Ctrl Pts',(-7.35822688079613,0.444367128060942,
13.7642280690127));
#14127=CARTESIAN_POINT('Ctrl Pts',(-7.3210256097581,0.147979855989742,13.7522248822233));
#14128=CARTESIAN_POINT('Ctrl Pts',(-7.28382433872007,-0.148407416081458,
13.740221695434));
#14129=CARTESIAN_POINT('Ctrl Pts',(-7.36358464744658,-0.457895344722512,
13.7282185086447));
#14130=CARTESIAN_POINT('Ctrl Pts',(-7.53940549437917,-0.699383189958172,
13.7162153218554));
#14131=CARTESIAN_POINT('Ctrl Pts',(-7.71522634131175,-0.940871035193831,
13.7042121350661));
#14132=CARTESIAN_POINT('Ctrl Pts',(-7.98526240565841,-1.11182427083109,
13.6922089482767));
#14133=CARTESIAN_POINT('Ctrl Pts',(-8.27875123560177,-1.16744491727758,
13.6802057614874));
#14134=CARTESIAN_POINT('Ctrl Pts',(-8.57224006554514,-1.22306556372407,
13.6682025746981));
#14135=CARTESIAN_POINT('Ctrl Pts',(-8.88610136060003,-1.16276985667004,
13.6561993879088));
#14136=CARTESIAN_POINT('Ctrl Pts',(-9.13808834820149,-1.00235817476314,
13.6441962011195));
#14137=CARTESIAN_POINT('Ctrl Pts',(-9.39007533580294,-0.841946492856251,
13.6321930143302));
#14138=CARTESIAN_POINT('Ctrl Pts',(-9.57754329642169,-0.583102430602309,
13.6201898275408));
#14139=CARTESIAN_POINT('Ctrl Pts',(-9.65136659729208,-0.29365559634556,
13.6081866407515));
#14140=CARTESIAN_POINT('Ctrl Pts',(-9.67581103310551,-0.197813707971929,
13.6042121350661));
#14141=CARTESIAN_POINT('Ctrl Pts',(-9.68822500000003,-0.0989100500919037,
13.6002376293806));
#14142=CARTESIAN_POINT('Ctrl Pts',(-9.688225,3.93907129137006E-13,13.5962631236952));
#14143=CARTESIAN_POINT('Ctrl Pts',(-9.688225,-1.35702560299933E-12,13.5537368763049));
#14144=CARTESIAN_POINT('Ctrl Pts',(-9.68822499999966,-0.298712821307417,
13.5657400630942));
#14145=CARTESIAN_POINT('Ctrl Pts',(-9.57054245632521,-0.595858078272685,
13.5777432498835));
#14146=CARTESIAN_POINT('Ctrl Pts',(-9.36601586214849,-0.813569405233634,
13.5897464366728));
#14147=CARTESIAN_POINT('Ctrl Pts',(-9.16148926797177,-1.03128073219458,
13.6017496234622));
#14148=CARTESIAN_POINT('Ctrl Pts',(-8.8722652241273,-1.16727314847172,13.6137528102515));
#14149=CARTESIAN_POINT('Ctrl Pts',(-8.57413435701335,-1.18591009260197,
13.6257559970408));
#14150=CARTESIAN_POINT('Ctrl Pts',(-8.27600348989941,-1.20454703673222,
13.6377591838301));
#14151=CARTESIAN_POINT('Ctrl Pts',(-7.97209482031995,-1.10563290540061,
13.6497623706194));
#14152=CARTESIAN_POINT('Ctrl Pts',(-7.74204705371982,-0.915087963995918,
13.6617655574087));
#14153=CARTESIAN_POINT('Ctrl Pts',(-7.51199928711969,-0.724543022591224,
13.6737687441981));
#14154=CARTESIAN_POINT('Ctrl Pts',(-7.35822688079599,-0.444367128060549,
13.6857719309874));
#14155=CARTESIAN_POINT('Ctrl Pts',(-7.32102560975806,-0.147979855989382,
13.6977751177767));
#14156=CARTESIAN_POINT('Ctrl Pts',(-7.28382433872012,0.148407416081785,
13.709778304566));
#14157=CARTESIAN_POINT('Ctrl Pts',(-7.3635846474467,0.457895344722766,13.7217814913553));
#14158=CARTESIAN_POINT('Ctrl Pts',(-7.5394054943793,0.699383189958356,13.7337846781446));
#14159=CARTESIAN_POINT('Ctrl Pts',(-7.7152263413119,0.940871035193946,13.745787864934));
#14160=CARTESIAN_POINT('Ctrl Pts',(-7.98526240565854,1.11182427083114,13.7577910517233));
#14161=CARTESIAN_POINT('Ctrl Pts',(-8.27875123560186,1.1674449172776,13.7697942385126));
#14162=CARTESIAN_POINT('Ctrl Pts',(-8.57224006554519,1.22306556372406,13.7817974253019));
#14163=CARTESIAN_POINT('Ctrl Pts',(-8.88610136060003,1.16276985667003,13.7938006120912));
#14164=CARTESIAN_POINT('Ctrl Pts',(-9.13808834820145,1.00235817476317,13.8058037988805));
#14165=CARTESIAN_POINT('Ctrl Pts',(-9.39007533580287,0.841946492856307,
13.8178069856699));
#14166=CARTESIAN_POINT('Ctrl Pts',(-9.57754329642162,0.583102430602426,
13.8298101724592));
#14167=CARTESIAN_POINT('Ctrl Pts',(-9.65136659729203,0.293655596345731,
13.8418133592485));
#14168=CARTESIAN_POINT('Ctrl Pts',(-9.67581103310558,0.197813707971733,
13.845787864934));
#14169=CARTESIAN_POINT('Ctrl Pts',(-9.68822500000011,0.0989100500913151,
13.8497623706194));
#14170=CARTESIAN_POINT('Ctrl Pts',(-9.688225,-1.36513023107909E-12,13.8537368763049));
#14171=CARTESIAN_POINT('Origin',(-8.5,0.,1.8));
#14172=CARTESIAN_POINT('',(-9.688225,3.77808895279941E-13,14.1962631236952));
#14173=CARTESIAN_POINT('',(-9.68865868051598,-0.000343891003544964,14.1537368763049));
#14174=CARTESIAN_POINT('',(-9.688225,-1.45515594291686E-16,1.8));
#14175=CARTESIAN_POINT('Ctrl Pts',(-9.688225,3.77808895279941E-13,14.1962631236952));
#14176=CARTESIAN_POINT('Ctrl Pts',(-9.68822499999991,0.29871282130646,14.1842599369058));
#14177=CARTESIAN_POINT('Ctrl Pts',(-9.57054245632568,0.595858078271847,
14.1722567501165));
#14178=CARTESIAN_POINT('Ctrl Pts',(-9.36601586214911,0.81356940523297,14.1602535633272));
#14179=CARTESIAN_POINT('Ctrl Pts',(-9.16148926797255,1.03128073219409,14.1482503765379));
#14180=CARTESIAN_POINT('Ctrl Pts',(-8.87226522412815,1.16727314847145,14.1362471897486));
#14181=CARTESIAN_POINT('Ctrl Pts',(-8.5741343570142,1.18591009260192,14.1242440029593));
#14182=CARTESIAN_POINT('Ctrl Pts',(-8.27600348990024,1.20454703673238,14.1122408161699));
#14183=CARTESIAN_POINT('Ctrl Pts',(-7.97209482032069,1.10563290540097,14.1002376293806));
#14184=CARTESIAN_POINT('Ctrl Pts',(-7.74204705372042,0.915087963996414,
14.0882344425913));
#14185=CARTESIAN_POINT('Ctrl Pts',(-7.51199928712015,0.724543022591856,
14.076231255802));
#14186=CARTESIAN_POINT('Ctrl Pts',(-7.35822688079626,0.444367128061253,
14.0642280690127));
#14187=CARTESIAN_POINT('Ctrl Pts',(-7.32102560975814,0.147979855990085,
14.0522248822234));
#14188=CARTESIAN_POINT('Ctrl Pts',(-7.28382433872003,-0.148407416081082,
14.040221695434));
#14189=CARTESIAN_POINT('Ctrl Pts',(-7.36358464744644,-0.457895344722135,
14.0282185086447));
#14190=CARTESIAN_POINT('Ctrl Pts',(-7.53940549437892,-0.699383189957837,
14.0162153218554));
#14191=CARTESIAN_POINT('Ctrl Pts',(-7.71522634131141,-0.94087103519354,
14.0042121350661));
#14192=CARTESIAN_POINT('Ctrl Pts',(-7.98526240565798,-1.11182427083088,
13.9922089482768));
#14193=CARTESIAN_POINT('Ctrl Pts',(-8.2787512356013,-1.16744491727749,13.9802057614874));
#14194=CARTESIAN_POINT('Ctrl Pts',(-8.57224006554462,-1.2230655637241,13.9682025746981));
#14195=CARTESIAN_POINT('Ctrl Pts',(-8.88610136059951,-1.1627698566702,13.9561993879088));
#14196=CARTESIAN_POINT('Ctrl Pts',(-9.13808834820102,-1.00235817476344,
13.9441962011195));
#14197=CARTESIAN_POINT('Ctrl Pts',(-9.39007533580253,-0.841946492856674,
13.9321930143302));
#14198=CARTESIAN_POINT('Ctrl Pts',(-9.5775432964214,-0.583102430602846,
13.9201898275409));
#14199=CARTESIAN_POINT('Ctrl Pts',(-9.65136659729192,-0.293655596346157,
13.9081866407515));
#14200=CARTESIAN_POINT('Ctrl Pts',(-9.67581103310547,-0.19781370797232,
13.9042121350661));
#14201=CARTESIAN_POINT('Ctrl Pts',(-9.68822500000004,-0.0989100500920693,
13.9002376293806));
#14202=CARTESIAN_POINT('Ctrl Pts',(-9.688225,4.53415083256914E-13,13.8962631236952));
#14203=CARTESIAN_POINT('Ctrl Pts',(-9.68655655853903,-0.000463272172757516,
13.8537368763049));
#14204=CARTESIAN_POINT('Ctrl Pts',(-9.68727352946558,-0.166355206423755,
13.8603818955633));
#14205=CARTESIAN_POINT('Ctrl Pts',(-9.65488880874086,-0.332016339541931,
13.8670269148217));
#14206=CARTESIAN_POINT('Ctrl Pts',(-9.58810721516616,-0.482507464589454,
13.8736719340801));
#14207=CARTESIAN_POINT('Ctrl Pts',(-9.42824047131953,-0.842764308599199,
13.8895792752318));
#14208=CARTESIAN_POINT('Ctrl Pts',(-9.07125782470074,-1.1160873825261,13.9054866163834));
#14209=CARTESIAN_POINT('Ctrl Pts',(-8.68208007088468,-1.17630173021062,
13.921393957535));
#14210=CARTESIAN_POINT('Ctrl Pts',(-8.29290231706859,-1.23651607789514,
13.9373012986866));
#14211=CARTESIAN_POINT('Ctrl Pts',(-7.87152945605521,-1.08362169933721,
13.9532086398383));
#14212=CARTESIAN_POINT('Ctrl Pts',(-7.60945480461122,-0.78893772856281,
13.9691159809899));
#14213=CARTESIAN_POINT('Ctrl Pts',(-7.47841747888923,-0.641595743175621,
13.9770696515657));
#14214=CARTESIAN_POINT('Ctrl Pts',(-7.38720470555958,-0.458806359734322,
13.9850233221415));
#14215=CARTESIAN_POINT('Ctrl Pts',(-7.34283850902019,-0.265277471449604,
13.9929769927173));
#14216=CARTESIAN_POINT('Ctrl Pts',(-7.2984723124808,-0.0717485831648862,
14.0009306632931));
#14217=CARTESIAN_POINT('Ctrl Pts',(-7.30095269273168,0.132519809963242,
14.0088843338689));
#14218=CARTESIAN_POINT('Ctrl Pts',(-7.35472170729873,0.322228361332696,
14.0168380044447));
#14219=CARTESIAN_POINT('Ctrl Pts',(-7.46225973643285,0.701645464071678,
14.0327453455964));
#14220=CARTESIAN_POINT('Ctrl Pts',(-7.7749523028318,1.02282319977593,14.048652686748));
#14221=CARTESIAN_POINT('Ctrl Pts',(-8.1514957837131,1.13814925380642,14.0645600278996));
#14222=CARTESIAN_POINT('Ctrl Pts',(-8.52803926459432,1.25347530783689,14.0804673690512));
#14223=CARTESIAN_POINT('Ctrl Pts',(-8.96843365995786,1.16294968019372,14.0963747102028));
#14224=CARTESIAN_POINT('Ctrl Pts',(-9.2692651211118,0.908307182907879,14.1122820513545));
#14225=CARTESIAN_POINT('Ctrl Pts',(-9.53058923645479,0.687106165312514,
14.1261003263379));
#14226=CARTESIAN_POINT('Ctrl Pts',(-9.6866002114824,0.342063792426944,14.1399186013214));
#14227=CARTESIAN_POINT('Ctrl Pts',(-9.68926336417008,-0.000823380536053999,
14.1537368763049));
#14228=CARTESIAN_POINT('Origin',(-8.5,0.,1.8));
#14229=CARTESIAN_POINT('',(-9.688225,4.03344024846319E-13,14.4962631236952));
#14230=CARTESIAN_POINT('',(-9.688225,-1.31394894964387E-12,14.4537368763049));
#14231=CARTESIAN_POINT('',(-9.688225,-1.45515594291686E-16,1.8));
#14232=CARTESIAN_POINT('Ctrl Pts',(-9.688225,4.03344024846319E-13,14.4962631236952));
#14233=CARTESIAN_POINT('Ctrl Pts',(-9.6882249999999,0.298712821306486,14.4842599369058));
#14234=CARTESIAN_POINT('Ctrl Pts',(-9.57054245632567,0.59585807827187,14.4722567501165));
#14235=CARTESIAN_POINT('Ctrl Pts',(-9.3660158621491,0.813569405232989,14.4602535633272));
#14236=CARTESIAN_POINT('Ctrl Pts',(-9.16148926797252,1.03128073219411,14.4482503765379));
#14237=CARTESIAN_POINT('Ctrl Pts',(-8.87226522412812,1.16727314847146,14.4362471897486));
#14238=CARTESIAN_POINT('Ctrl Pts',(-8.57413435701417,1.18591009260192,14.4242440029593));
#14239=CARTESIAN_POINT('Ctrl Pts',(-8.27600348990022,1.20454703673238,14.4122408161699));
#14240=CARTESIAN_POINT('Ctrl Pts',(-7.97209482032066,1.10563290540096,14.4002376293806));
#14241=CARTESIAN_POINT('Ctrl Pts',(-7.7420470537204,0.915087963996397,14.3882344425913));
#14242=CARTESIAN_POINT('Ctrl Pts',(-7.51199928712013,0.724543022591834,
14.376231255802));
#14243=CARTESIAN_POINT('Ctrl Pts',(-7.35822688079625,0.444367128061228,
14.3642280690127));
#14244=CARTESIAN_POINT('Ctrl Pts',(-7.32102560975814,0.14797985599006,14.3522248822234));
#14245=CARTESIAN_POINT('Ctrl Pts',(-7.28382433872003,-0.148407416081108,
14.340221695434));
#14246=CARTESIAN_POINT('Ctrl Pts',(-7.36358464744645,-0.457895344722159,
14.3282185086447));
#14247=CARTESIAN_POINT('Ctrl Pts',(-7.53940549437894,-0.699383189957858,
14.3162153218554));
#14248=CARTESIAN_POINT('Ctrl Pts',(-7.71522634131143,-0.940871035193557,
14.3042121350661));
#14249=CARTESIAN_POINT('Ctrl Pts',(-7.985262405658,-1.1118242708309,14.2922089482768));
#14250=CARTESIAN_POINT('Ctrl Pts',(-8.27875123560133,-1.1674449172775,14.2802057614874));
#14251=CARTESIAN_POINT('Ctrl Pts',(-8.57224006554465,-1.2230655637241,14.2682025746981));
#14252=CARTESIAN_POINT('Ctrl Pts',(-8.88610136059954,-1.16276985667019,
14.2561993879088));
#14253=CARTESIAN_POINT('Ctrl Pts',(-9.13808834820104,-1.00235817476342,
14.2441962011195));
#14254=CARTESIAN_POINT('Ctrl Pts',(-9.39007533580255,-0.841946492856655,
14.2321930143302));
#14255=CARTESIAN_POINT('Ctrl Pts',(-9.57754329642141,-0.583102430602823,
14.2201898275409));
#14256=CARTESIAN_POINT('Ctrl Pts',(-9.65136659729193,-0.293655596346132,
14.2081866407515));
#14257=CARTESIAN_POINT('Ctrl Pts',(-9.67581103310546,-0.197813707972328,
14.2042121350661));
#14258=CARTESIAN_POINT('Ctrl Pts',(-9.68822500000003,-0.0989100500921112,
14.2002376293806));
#14259=CARTESIAN_POINT('Ctrl Pts',(-9.688225,3.77808895279941E-13,14.1962631236952));
#14260=CARTESIAN_POINT('Ctrl Pts',(-9.688225,-1.27203803046427E-12,14.1537368763049));
#14261=CARTESIAN_POINT('Ctrl Pts',(-9.68822499999968,-0.298712821307377,
14.1657400630942));
#14262=CARTESIAN_POINT('Ctrl Pts',(-9.57054245632521,-0.595858078272697,
14.1777432498835));
#14263=CARTESIAN_POINT('Ctrl Pts',(-9.36601586214845,-0.813569405233671,
14.1897464366728));
#14264=CARTESIAN_POINT('Ctrl Pts',(-9.1614892679717,-1.03128073219465,14.2017496234622));
#14265=CARTESIAN_POINT('Ctrl Pts',(-8.87226522412716,-1.16727314847177,
14.2137528102515));
#14266=CARTESIAN_POINT('Ctrl Pts',(-8.57413435701317,-1.18591009260198,
14.2257559970408));
#14267=CARTESIAN_POINT('Ctrl Pts',(-8.27600348989917,-1.20454703673219,
14.2377591838301));
#14268=CARTESIAN_POINT('Ctrl Pts',(-7.97209482031969,-1.1056329054005,14.2497623706194));
#14269=CARTESIAN_POINT('Ctrl Pts',(-7.74204705371957,-0.915087963995714,
14.2617655574088));
#14270=CARTESIAN_POINT('Ctrl Pts',(-7.51199928711946,-0.724543022590929,
14.2737687441981));
#14271=CARTESIAN_POINT('Ctrl Pts',(-7.35822688079583,-0.444367128060156,
14.2857719309874));
#14272=CARTESIAN_POINT('Ctrl Pts',(-7.321025609758,-0.14797985598893,14.2977751177767));
#14273=CARTESIAN_POINT('Ctrl Pts',(-7.28382433872017,0.148407416082296,
14.309778304566));
#14274=CARTESIAN_POINT('Ctrl Pts',(-7.3635846474469,0.457895344723294,14.3217814913553));
#14275=CARTESIAN_POINT('Ctrl Pts',(-7.53940549437965,0.699383189958833,
14.3337846781447));
#14276=CARTESIAN_POINT('Ctrl Pts',(-7.7152263413124,0.940871035194372,14.345787864934));
#14277=CARTESIAN_POINT('Ctrl Pts',(-7.98526240565917,1.11182427083144,14.3577910517233));
#14278=CARTESIAN_POINT('Ctrl Pts',(-8.27875123560258,1.16744491727773,14.3697942385126));
#14279=CARTESIAN_POINT('Ctrl Pts',(-8.57224006554599,1.22306556372402,14.3817974253019));
#14280=CARTESIAN_POINT('Ctrl Pts',(-8.88610136060083,1.16276985666977,14.3938006120913));
#14281=CARTESIAN_POINT('Ctrl Pts',(-9.13808834820217,1.0023581747627,14.4058037988806));
#14282=CARTESIAN_POINT('Ctrl Pts',(-9.39007533580352,0.841946492855638,
14.4178069856699));
#14283=CARTESIAN_POINT('Ctrl Pts',(-9.5775432964221,0.583102430601566,14.4298101724592));
#14284=CARTESIAN_POINT('Ctrl Pts',(-9.65136659729228,0.293655596344766,
14.4418133592485));
#14285=CARTESIAN_POINT('Ctrl Pts',(-9.67581103310566,0.197813707971086,
14.445787864934));
#14286=CARTESIAN_POINT('Ctrl Pts',(-9.68822500000011,0.0989100500910174,
14.4497623706194));
#14287=CARTESIAN_POINT('Ctrl Pts',(-9.688225,-1.31394894964387E-12,14.4537368763049));
#14288=CARTESIAN_POINT('Origin',(-8.5,0.,1.8));
#14289=CARTESIAN_POINT('',(-9.688225,4.28879154412698E-13,14.7962631236952));
#14290=CARTESIAN_POINT('',(-9.688225,-1.28830279777503E-12,14.7537368763049));
#14291=CARTESIAN_POINT('',(-9.688225,-1.45515594291686E-16,1.8));
#14292=CARTESIAN_POINT('Ctrl Pts',(-9.688225,4.96602758914833E-13,14.7962631236952));
#14293=CARTESIAN_POINT('Ctrl Pts',(-9.68822499999988,0.298712821306624,
14.7842599369058));
#14294=CARTESIAN_POINT('Ctrl Pts',(-9.57054245632558,0.595858078272043,
14.7722567501165));
#14295=CARTESIAN_POINT('Ctrl Pts',(-9.36601586214894,0.813569405233155,
14.7602535633272));
#14296=CARTESIAN_POINT('Ctrl Pts',(-9.16148926797229,1.03128073219427,14.7482503765379));
#14297=CARTESIAN_POINT('Ctrl Pts',(-8.87226522412781,1.16727314847157,14.7362471897486));
#14298=CARTESIAN_POINT('Ctrl Pts',(-8.57413435701381,1.18591009260194,14.7242440029592));
#14299=CARTESIAN_POINT('Ctrl Pts',(-8.2760034898998,1.20454703673231,14.7122408161699));
#14300=CARTESIAN_POINT('Ctrl Pts',(-7.97209482032024,1.10563290540077,14.7002376293806));
#14301=CARTESIAN_POINT('Ctrl Pts',(-7.74204705372001,0.915087963996079,
14.6882344425913));
#14302=CARTESIAN_POINT('Ctrl Pts',(-7.51199928711979,0.724543022591391,
14.676231255802));
#14303=CARTESIAN_POINT('Ctrl Pts',(-7.35822688079602,0.444367128060664,
14.6642280690126));
#14304=CARTESIAN_POINT('Ctrl Pts',(-7.32102560975806,0.147979855989431,
14.6522248822233));
#14305=CARTESIAN_POINT('Ctrl Pts',(-7.2838243387201,-0.148407416081801,
14.640221695434));
#14306=CARTESIAN_POINT('Ctrl Pts',(-7.36358464744672,-0.457895344722858,
14.6282185086447));
#14307=CARTESIAN_POINT('Ctrl Pts',(-7.53940549437939,-0.699383189958479,
14.6162153218554));
#14308=CARTESIAN_POINT('Ctrl Pts',(-7.71522634131207,-0.940871035194101,
14.604212135066));
#14309=CARTESIAN_POINT('Ctrl Pts',(-7.9852624056588,-1.11182427083128,14.5922089482767));
#14310=CARTESIAN_POINT('Ctrl Pts',(-8.27875123560221,-1.16744491727767,
14.5802057614874));
#14311=CARTESIAN_POINT('Ctrl Pts',(-8.57224006554563,-1.22306556372405,
14.5682025746981));
#14312=CARTESIAN_POINT('Ctrl Pts',(-8.88610136060052,-1.16276985666988,
14.5561993879088));
#14313=CARTESIAN_POINT('Ctrl Pts',(-9.13808834820192,-1.00235817476287,
14.5441962011195));
#14314=CARTESIAN_POINT('Ctrl Pts',(-9.39007533580332,-0.841946492855853,
14.5321930143301));
#14315=CARTESIAN_POINT('Ctrl Pts',(-9.57754329642198,-0.583102430601802,
14.5201898275408));
#14316=CARTESIAN_POINT('Ctrl Pts',(-9.65136659729222,-0.293655596344994,
14.5081866407515));
#14317=CARTESIAN_POINT('Ctrl Pts',(-9.67581103310556,-0.197813707971537,
14.5042121350661));
#14318=CARTESIAN_POINT('Ctrl Pts',(-9.68822500000003,-0.0989100500917029,
14.5002376293806));
#14319=CARTESIAN_POINT('Ctrl Pts',(-9.688225,4.03344024846319E-13,14.4962631236952));
#14320=CARTESIAN_POINT('Ctrl Pts',(-9.688225,-1.31394894964387E-12,14.4537368763049));
#14321=CARTESIAN_POINT('Ctrl Pts',(-9.68822499999967,-0.298712821307396,
14.4657400630942));
#14322=CARTESIAN_POINT('Ctrl Pts',(-9.57054245632521,-0.59585807827269,
14.4777432498835));
#14323=CARTESIAN_POINT('Ctrl Pts',(-9.36601586214847,-0.813569405233652,
14.4897464366728));
#14324=CARTESIAN_POINT('Ctrl Pts',(-9.16148926797173,-1.03128073219461,
14.5017496234622));
#14325=CARTESIAN_POINT('Ctrl Pts',(-8.87226522412723,-1.16727314847175,
14.5137528102515));
#14326=CARTESIAN_POINT('Ctrl Pts',(-8.57413435701326,-1.18591009260198,
14.5257559970408));
#14327=CARTESIAN_POINT('Ctrl Pts',(-8.27600348989929,-1.20454703673221,
14.5377591838301));
#14328=CARTESIAN_POINT('Ctrl Pts',(-7.97209482031982,-1.10563290540056,
14.5497623706194));
#14329=CARTESIAN_POINT('Ctrl Pts',(-7.7420470537197,-0.915087963995816,
14.5617655574087));
#14330=CARTESIAN_POINT('Ctrl Pts',(-7.51199928711958,-0.724543022591077,
14.5737687441981));
#14331=CARTESIAN_POINT('Ctrl Pts',(-7.35822688079591,-0.444367128060353,
14.5857719309874));
#14332=CARTESIAN_POINT('Ctrl Pts',(-7.32102560975803,-0.147979855989156,
14.5977751177767));
#14333=CARTESIAN_POINT('Ctrl Pts',(-7.28382433872015,0.14840741608204,14.609778304566));
#14334=CARTESIAN_POINT('Ctrl Pts',(-7.3635846474468,0.45789534472303,14.6217814913553));
#14335=CARTESIAN_POINT('Ctrl Pts',(-7.53940549437947,0.699383189958594,
14.6337846781447));
#14336=CARTESIAN_POINT('Ctrl Pts',(-7.71522634131215,0.940871035194158,
14.645787864934));
#14337=CARTESIAN_POINT('Ctrl Pts',(-7.98526240565885,1.11182427083129,14.6577910517233));
#14338=CARTESIAN_POINT('Ctrl Pts',(-8.27875123560222,1.16744491727767,14.6697942385126));
#14339=CARTESIAN_POINT('Ctrl Pts',(-8.57224006554559,1.22306556372404,14.6817974253019));
#14340=CARTESIAN_POINT('Ctrl Pts',(-8.88610136060043,1.1627698566699,14.6938006120912));
#14341=CARTESIAN_POINT('Ctrl Pts',(-9.13808834820181,1.00235817476294,14.7058037988806));
#14342=CARTESIAN_POINT('Ctrl Pts',(-9.39007533580319,0.841946492855973,
14.7178069856699));
#14343=CARTESIAN_POINT('Ctrl Pts',(-9.57754329642186,0.583102430601997,
14.7298101724592));
#14344=CARTESIAN_POINT('Ctrl Pts',(-9.65136659729215,0.293655596345249,
14.7418133592485));
#14345=CARTESIAN_POINT('Ctrl Pts',(-9.67581103310561,0.197813707971427,
14.745787864934));
#14346=CARTESIAN_POINT('Ctrl Pts',(-9.68822500000011,0.0989100500912006,
14.7497623706194));
#14347=CARTESIAN_POINT('Ctrl Pts',(-9.688225,-1.28830279777503E-12,14.7537368763049));
#14348=CARTESIAN_POINT('Origin',(-8.5,0.,1.8));
#14349=CARTESIAN_POINT('',(-9.688225,4.54525306281539E-13,15.0962631236952));
#14350=CARTESIAN_POINT('',(-9.688225,-1.26271215705742E-12,15.0537368763049));
#14351=CARTESIAN_POINT('',(-9.688225,-1.45515594291686E-16,1.8));
#14352=CARTESIAN_POINT('Ctrl Pts',(-9.688225,4.54525306281539E-13,15.0962631236952));
#14353=CARTESIAN_POINT('Ctrl Pts',(-9.68822499999989,0.298712821306559,
15.0842599369058));
#14354=CARTESIAN_POINT('Ctrl Pts',(-9.57054245632562,0.595858078271961,
15.0722567501165));
#14355=CARTESIAN_POINT('Ctrl Pts',(-9.36601586214901,0.813569405233076,
15.0602535633272));
#14356=CARTESIAN_POINT('Ctrl Pts',(-9.1614892679724,1.03128073219419,15.0482503765379));
#14357=CARTESIAN_POINT('Ctrl Pts',(-8.87226522412796,1.16727314847152,15.0362471897486));
#14358=CARTESIAN_POINT('Ctrl Pts',(-8.57413435701398,1.18591009260193,15.0242440029593));
#14359=CARTESIAN_POINT('Ctrl Pts',(-8.2760034899,1.20454703673235,15.0122408161699));
#14360=CARTESIAN_POINT('Ctrl Pts',(-7.97209482032045,1.10563290540086,15.0002376293806));
#14361=CARTESIAN_POINT('Ctrl Pts',(-7.7420470537202,0.915087963996235,14.9882344425913));
#14362=CARTESIAN_POINT('Ctrl Pts',(-7.51199928711996,0.724543022591609,
14.976231255802));
#14363=CARTESIAN_POINT('Ctrl Pts',(-7.35822688079613,0.444367128060941,
14.9642280690127));
#14364=CARTESIAN_POINT('Ctrl Pts',(-7.3210256097581,0.147979855989741,14.9522248822233));
#14365=CARTESIAN_POINT('Ctrl Pts',(-7.28382433872007,-0.148407416081459,
14.940221695434));
#14366=CARTESIAN_POINT('Ctrl Pts',(-7.36358464744658,-0.457895344722513,
14.9282185086447));
#14367=CARTESIAN_POINT('Ctrl Pts',(-7.53940549437917,-0.699383189958172,
14.9162153218554));
#14368=CARTESIAN_POINT('Ctrl Pts',(-7.71522634131175,-0.940871035193832,
14.9042121350661));
#14369=CARTESIAN_POINT('Ctrl Pts',(-7.98526240565841,-1.11182427083109,
14.8922089482767));
#14370=CARTESIAN_POINT('Ctrl Pts',(-8.27875123560177,-1.16744491727758,
14.8802057614874));
#14371=CARTESIAN_POINT('Ctrl Pts',(-8.57224006554514,-1.22306556372407,
14.8682025746981));
#14372=CARTESIAN_POINT('Ctrl Pts',(-8.88610136060003,-1.16276985667004,
14.8561993879088));
#14373=CARTESIAN_POINT('Ctrl Pts',(-9.13808834820149,-1.00235817476314,
14.8441962011195));
#14374=CARTESIAN_POINT('Ctrl Pts',(-9.39007533580294,-0.841946492856251,
14.8321930143302));
#14375=CARTESIAN_POINT('Ctrl Pts',(-9.5775432964217,-0.583102430602308,
14.8201898275408));
#14376=CARTESIAN_POINT('Ctrl Pts',(-9.65136659729208,-0.293655596345558,
14.8081866407515));
#14377=CARTESIAN_POINT('Ctrl Pts',(-9.67581103310552,-0.197813707971895,
14.8042121350661));
#14378=CARTESIAN_POINT('Ctrl Pts',(-9.68822500000004,-0.0989100500918347,
14.8002376293806));
#14379=CARTESIAN_POINT('Ctrl Pts',(-9.688225,4.96602758914833E-13,14.7962631236952));
#14380=CARTESIAN_POINT('Ctrl Pts',(-9.688225,-1.28830279777503E-12,14.7537368763049));
#14381=CARTESIAN_POINT('Ctrl Pts',(-9.68822499999968,-0.298712821307393,
14.7657400630942));
#14382=CARTESIAN_POINT('Ctrl Pts',(-9.57054245632521,-0.595858078272712,
14.7777432498835));
#14383=CARTESIAN_POINT('Ctrl Pts',(-9.36601586214844,-0.813569405233683,
14.7897464366728));
#14384=CARTESIAN_POINT('Ctrl Pts',(-9.16148926797168,-1.03128073219465,
14.8017496234622));
#14385=CARTESIAN_POINT('Ctrl Pts',(-8.87226522412714,-1.16727314847178,
14.8137528102515));
#14386=CARTESIAN_POINT('Ctrl Pts',(-8.57413435701315,-1.18591009260198,
14.8257559970408));
#14387=CARTESIAN_POINT('Ctrl Pts',(-8.27600348989916,-1.20454703673219,
14.8377591838301));
#14388=CARTESIAN_POINT('Ctrl Pts',(-7.97209482031967,-1.10563290540049,
14.8497623706194));
#14389=CARTESIAN_POINT('Ctrl Pts',(-7.74204705371956,-0.915087963995703,
14.8617655574088));
#14390=CARTESIAN_POINT('Ctrl Pts',(-7.51199928711945,-0.724543022590915,
14.8737687441981));
#14391=CARTESIAN_POINT('Ctrl Pts',(-7.35822688079582,-0.44436712806014,
14.8857719309874));
#14392=CARTESIAN_POINT('Ctrl Pts',(-7.321025609758,-0.147979855988914,14.8977751177767));
#14393=CARTESIAN_POINT('Ctrl Pts',(-7.28382433872017,0.148407416082312,
14.909778304566));
#14394=CARTESIAN_POINT('Ctrl Pts',(-7.36358464744691,0.45789534472331,14.9217814913553));
#14395=CARTESIAN_POINT('Ctrl Pts',(-7.53940549437966,0.699383189958846,
14.9337846781447));
#14396=CARTESIAN_POINT('Ctrl Pts',(-7.71522634131241,0.940871035194383,
14.945787864934));
#14397=CARTESIAN_POINT('Ctrl Pts',(-7.98526240565919,1.11182427083145,14.9577910517233));
#14398=CARTESIAN_POINT('Ctrl Pts',(-8.27875123560259,1.16744491727774,14.9697942385126));
#14399=CARTESIAN_POINT('Ctrl Pts',(-8.572240065546,1.22306556372402,14.9817974253019));
#14400=CARTESIAN_POINT('Ctrl Pts',(-8.88610136060085,1.16276985666977,14.9938006120913));
#14401=CARTESIAN_POINT('Ctrl Pts',(-9.13808834820219,1.0023581747627,15.0058037988806));
#14402=CARTESIAN_POINT('Ctrl Pts',(-9.39007533580353,0.841946492855626,
15.0178069856699));
#14403=CARTESIAN_POINT('Ctrl Pts',(-9.57754329642211,0.583102430601552,
15.0298101724592));
#14404=CARTESIAN_POINT('Ctrl Pts',(-9.65136659729228,0.293655596344751,
15.0418133592485));
#14405=CARTESIAN_POINT('Ctrl Pts',(-9.67581103310565,0.197813707971113,
15.045787864934));
#14406=CARTESIAN_POINT('Ctrl Pts',(-9.6882250000001,0.0989100500910911,
15.0497623706194));
#14407=CARTESIAN_POINT('Ctrl Pts',(-9.688225,-1.19515508600898E-12,15.0537368763049));
#14408=CARTESIAN_POINT('Origin',(-8.5,0.,1.8));
#14409=CARTESIAN_POINT('',(-9.688225,4.8017145815038E-13,15.3962631236952));
#14410=CARTESIAN_POINT('',(-9.688225,-1.23712151633981E-12,15.3537368763049));
#14411=CARTESIAN_POINT('',(-9.688225,-1.45515594291686E-16,1.8));
#14412=CARTESIAN_POINT('Ctrl Pts',(-9.688225,5.4767301804759E-13,15.3962631236952));
#14413=CARTESIAN_POINT('Ctrl Pts',(-9.68822499999986,0.298712821306675,
15.3842599369058));
#14414=CARTESIAN_POINT('Ctrl Pts',(-9.57054245632556,0.595858078272089,
15.3722567501165));
#14415=CARTESIAN_POINT('Ctrl Pts',(-9.3660158621489,0.813569405233193,15.3602535633272));
#14416=CARTESIAN_POINT('Ctrl Pts',(-9.16148926797225,1.0312807321943,15.3482503765379));
#14417=CARTESIAN_POINT('Ctrl Pts',(-8.87226522412776,1.16727314847159,15.3362471897486));
#14418=CARTESIAN_POINT('Ctrl Pts',(-8.57413435701375,1.18591009260195,15.3242440029592));
#14419=CARTESIAN_POINT('Ctrl Pts',(-8.27600348989975,1.2045470367323,15.3122408161699));
#14420=CARTESIAN_POINT('Ctrl Pts',(-7.97209482032019,1.10563290540075,15.3002376293806));
#14421=CARTESIAN_POINT('Ctrl Pts',(-7.74204705371997,0.915087963996047,
15.2882344425913));
#14422=CARTESIAN_POINT('Ctrl Pts',(-7.51199928711976,0.724543022591348,
15.276231255802));
#14423=CARTESIAN_POINT('Ctrl Pts',(-7.358226880796,0.444367128060615,15.2642280690126));
#14424=CARTESIAN_POINT('Ctrl Pts',(-7.32102560975806,0.147979855989381,
15.2522248822233));
#14425=CARTESIAN_POINT('Ctrl Pts',(-7.28382433872011,-0.148407416081853,
15.240221695434));
#14426=CARTESIAN_POINT('Ctrl Pts',(-7.36358464744674,-0.457895344722907,
15.2282185086447));
#14427=CARTESIAN_POINT('Ctrl Pts',(-7.53940549437942,-0.699383189958521,
15.2162153218554));
#14428=CARTESIAN_POINT('Ctrl Pts',(-7.71522634131211,-0.940871035194135,
15.204212135066));
#14429=CARTESIAN_POINT('Ctrl Pts',(-7.98526240565885,-1.1118242708313,15.1922089482767));
#14430=CARTESIAN_POINT('Ctrl Pts',(-8.27875123560226,-1.16744491727767,
15.1802057614874));
#14431=CARTESIAN_POINT('Ctrl Pts',(-8.57224006554568,-1.22306556372405,
15.1682025746981));
#14432=CARTESIAN_POINT('Ctrl Pts',(-8.88610136060057,-1.16276985666986,
15.1561993879088));
#14433=CARTESIAN_POINT('Ctrl Pts',(-9.13808834820196,-1.00235817476284,
15.1441962011195));
#14434=CARTESIAN_POINT('Ctrl Pts',(-9.39007533580336,-0.841946492855815,
15.1321930143301));
#14435=CARTESIAN_POINT('Ctrl Pts',(-9.577543296422,-0.583102430601755,15.1201898275408));
#14436=CARTESIAN_POINT('Ctrl Pts',(-9.65136659729223,-0.293655596344945,
15.1081866407515));
#14437=CARTESIAN_POINT('Ctrl Pts',(-9.67581103310557,-0.197813707971486,
15.104212135066));
#14438=CARTESIAN_POINT('Ctrl Pts',(-9.68822500000004,-0.0989100500916517,
15.1002376293806));
#14439=CARTESIAN_POINT('Ctrl Pts',(-9.688225,4.54525306281539E-13,15.0962631236952));
#14440=CARTESIAN_POINT('Ctrl Pts',(-9.688225,-1.19515508600898E-12,15.0537368763049));
#14441=CARTESIAN_POINT('Ctrl Pts',(-9.6882249999997,-0.298712821307277,
15.0657400630942));
#14442=CARTESIAN_POINT('Ctrl Pts',(-9.57054245632527,-0.595858078272583,
15.0777432498835));
#14443=CARTESIAN_POINT('Ctrl Pts',(-9.36601586214855,-0.813569405233566,
15.0897464366728));
#14444=CARTESIAN_POINT('Ctrl Pts',(-9.16148926797184,-1.03128073219455,
15.1017496234622));
#14445=CARTESIAN_POINT('Ctrl Pts',(-8.87226522412734,-1.16727314847171,
15.1137528102515));
#14446=CARTESIAN_POINT('Ctrl Pts',(-8.57413435701338,-1.18591009260197,
15.1257559970408));
#14447=CARTESIAN_POINT('Ctrl Pts',(-8.27600348989941,-1.20454703673223,
15.1377591838301));
#14448=CARTESIAN_POINT('Ctrl Pts',(-7.97209482031993,-1.10563290540061,
15.1497623706194));
#14449=CARTESIAN_POINT('Ctrl Pts',(-7.74204705371979,-0.915087963995892,
15.1617655574087));
#14450=CARTESIAN_POINT('Ctrl Pts',(-7.51199928711965,-0.724543022591176,
15.1737687441981));
#14451=CARTESIAN_POINT('Ctrl Pts',(-7.35822688079596,-0.444367128060467,
15.1857719309874));
#14452=CARTESIAN_POINT('Ctrl Pts',(-7.32102560975804,-0.147979855989274,
15.1977751177767));
#14453=CARTESIAN_POINT('Ctrl Pts',(-7.28382433872013,0.148407416081918,
15.209778304566));
#14454=CARTESIAN_POINT('Ctrl Pts',(-7.36358464744675,0.457895344722916,
15.2217814913553));
#14455=CARTESIAN_POINT('Ctrl Pts',(-7.5394054943794,0.699383189958498,15.2337846781446));
#14456=CARTESIAN_POINT('Ctrl Pts',(-7.71522634131206,0.94087103519408,15.245787864934));
#14457=CARTESIAN_POINT('Ctrl Pts',(-7.98526240565874,1.11182427083124,15.2577910517233));
#14458=CARTESIAN_POINT('Ctrl Pts',(-8.2787512356021,1.16744491727764,15.2697942385126));
#14459=CARTESIAN_POINT('Ctrl Pts',(-8.57224006554547,1.22306556372405,15.2817974253019));
#14460=CARTESIAN_POINT('Ctrl Pts',(-8.88610136060031,1.16276985666994,15.2938006120912));
#14461=CARTESIAN_POINT('Ctrl Pts',(-9.13808834820171,1.002358174763,15.3058037988806));
#14462=CARTESIAN_POINT('Ctrl Pts',(-9.39007533580311,0.841946492856062,
15.3178069856699));
#14463=CARTESIAN_POINT('Ctrl Pts',(-9.5775432964218,0.583102430602104,15.3298101724592));
#14464=CARTESIAN_POINT('Ctrl Pts',(-9.65136659729213,0.293655596345364,
15.3418133592485));
#14465=CARTESIAN_POINT('Ctrl Pts',(-9.6758110331056,0.197813707971522,15.345787864934));
#14466=CARTESIAN_POINT('Ctrl Pts',(-9.6882250000001,0.0989100500912743,
15.3497623706194));
#14467=CARTESIAN_POINT('Ctrl Pts',(-9.688225,-1.23712151633981E-12,15.3537368763049));
#14468=CARTESIAN_POINT('Origin',(-8.5,0.,1.8));
#14469=CARTESIAN_POINT('',(-9.688225,5.05817610019221E-13,15.6962631236952));
#14470=CARTESIAN_POINT('',(-9.688225,-1.21141985331974E-12,15.6537368763049));
#14471=CARTESIAN_POINT('',(-9.688225,-1.45515594291686E-16,1.8));
#14472=CARTESIAN_POINT('Ctrl Pts',(-9.688225,5.05817610019221E-13,15.6962631236952));
#14473=CARTESIAN_POINT('Ctrl Pts',(-9.68822499999987,0.298712821306611,
15.6842599369058));
#14474=CARTESIAN_POINT('Ctrl Pts',(-9.5705424563256,0.595858078272007,15.6722567501165));
#14475=CARTESIAN_POINT('Ctrl Pts',(-9.36601586214898,0.813569405233113,
15.6602535633272));
#14476=CARTESIAN_POINT('Ctrl Pts',(-9.16148926797236,1.03128073219422,15.6482503765379));
#14477=CARTESIAN_POINT('Ctrl Pts',(-8.87226522412791,1.16727314847153,15.6362471897486));
#14478=CARTESIAN_POINT('Ctrl Pts',(-8.57413435701393,1.18591009260194,15.6242440029592));
#14479=CARTESIAN_POINT('Ctrl Pts',(-8.27600348989995,1.20454703673234,15.6122408161699));
#14480=CARTESIAN_POINT('Ctrl Pts',(-7.9720948203204,1.10563290540084,15.6002376293806));
#14481=CARTESIAN_POINT('Ctrl Pts',(-7.74204705372016,0.915087963996203,
15.5882344425913));
#14482=CARTESIAN_POINT('Ctrl Pts',(-7.51199928711993,0.724543022591566,
15.576231255802));
#14483=CARTESIAN_POINT('Ctrl Pts',(-7.35822688079612,0.444367128060892,
15.5642280690127));
#14484=CARTESIAN_POINT('Ctrl Pts',(-7.3210256097581,0.14797985598969,15.5522248822233));
#14485=CARTESIAN_POINT('Ctrl Pts',(-7.28382433872008,-0.148407416081511,
15.540221695434));
#14486=CARTESIAN_POINT('Ctrl Pts',(-7.3635846474466,-0.457895344722562,
15.5282185086447));
#14487=CARTESIAN_POINT('Ctrl Pts',(-7.5394054943792,-0.699383189958214,
15.5162153218554));
#14488=CARTESIAN_POINT('Ctrl Pts',(-7.71522634131179,-0.940871035193866,
15.5042121350661));
#14489=CARTESIAN_POINT('Ctrl Pts',(-7.98526240565846,-1.11182427083111,
15.4922089482767));
#14490=CARTESIAN_POINT('Ctrl Pts',(-8.27875123560183,-1.16744491727759,
15.4802057614874));
#14491=CARTESIAN_POINT('Ctrl Pts',(-8.5722400655452,-1.22306556372407,15.4682025746981));
#14492=CARTESIAN_POINT('Ctrl Pts',(-8.88610136060008,-1.16276985667002,
15.4561993879088));
#14493=CARTESIAN_POINT('Ctrl Pts',(-9.13808834820153,-1.00235817476312,
15.4441962011195));
#14494=CARTESIAN_POINT('Ctrl Pts',(-9.39007533580298,-0.841946492856212,
15.4321930143302));
#14495=CARTESIAN_POINT('Ctrl Pts',(-9.57754329642172,-0.583102430602261,
15.4201898275408));
#14496=CARTESIAN_POINT('Ctrl Pts',(-9.65136659729209,-0.293655596345509,
15.4081866407515));
#14497=CARTESIAN_POINT('Ctrl Pts',(-9.67581103310553,-0.197813707971844,
15.4042121350661));
#14498=CARTESIAN_POINT('Ctrl Pts',(-9.68822500000005,-0.0989100500917836,
15.4002376293806));
#14499=CARTESIAN_POINT('Ctrl Pts',(-9.688225,5.4767301804759E-13,15.3962631236952));
#14500=CARTESIAN_POINT('Ctrl Pts',(-9.688225,-1.23712151633981E-12,15.3537368763049));
#14501=CARTESIAN_POINT('Ctrl Pts',(-9.68822499999969,-0.298712821307319,
15.3657400630942));
#14502=CARTESIAN_POINT('Ctrl Pts',(-9.57054245632525,-0.595858078272621,
15.3777432498835));
#14503=CARTESIAN_POINT('Ctrl Pts',(-9.36601586214852,-0.813569405233596,
15.3897464366728));
#14504=CARTESIAN_POINT('Ctrl Pts',(-9.1614892679718,-1.03128073219457,15.4017496234622));
#14505=CARTESIAN_POINT('Ctrl Pts',(-8.8722652241273,-1.16727314847172,15.4137528102515));
#14506=CARTESIAN_POINT('Ctrl Pts',(-8.57413435701334,-1.18591009260197,
15.4257559970408));
#14507=CARTESIAN_POINT('Ctrl Pts',(-8.27600348989937,-1.20454703673222,
15.4377591838301));
#14508=CARTESIAN_POINT('Ctrl Pts',(-7.97209482031989,-1.10563290540059,
15.4497623706194));
#14509=CARTESIAN_POINT('Ctrl Pts',(-7.74204705371976,-0.915087963995865,
15.4617655574087));
#14510=CARTESIAN_POINT('Ctrl Pts',(-7.51199928711962,-0.724543022591141,
15.4737687441981));
#14511=CARTESIAN_POINT('Ctrl Pts',(-7.35822688079594,-0.444367128060427,
15.4857719309874));
#14512=CARTESIAN_POINT('Ctrl Pts',(-7.32102560975804,-0.147979855989233,
15.4977751177767));
#14513=CARTESIAN_POINT('Ctrl Pts',(-7.28382433872014,0.148407416081961,
15.509778304566));
#14514=CARTESIAN_POINT('Ctrl Pts',(-7.36358464744677,0.457895344722956,
15.5217814913553));
#14515=CARTESIAN_POINT('Ctrl Pts',(-7.53940549437943,0.699383189958532,
15.5337846781447));
#14516=CARTESIAN_POINT('Ctrl Pts',(-7.71522634131209,0.940871035194107,
15.545787864934));
#14517=CARTESIAN_POINT('Ctrl Pts',(-7.98526240565878,1.11182427083126,15.5577910517233));
#14518=CARTESIAN_POINT('Ctrl Pts',(-8.27875123560215,1.16744491727765,15.5697942385126));
#14519=CARTESIAN_POINT('Ctrl Pts',(-8.57224006554551,1.22306556372405,15.5817974253019));
#14520=CARTESIAN_POINT('Ctrl Pts',(-8.88610136060035,1.16276985666992,15.5938006120912));
#14521=CARTESIAN_POINT('Ctrl Pts',(-9.13808834820175,1.00235817476298,15.6058037988806));
#14522=CARTESIAN_POINT('Ctrl Pts',(-9.39007533580314,0.84194649285603,15.6178069856699));
#14523=CARTESIAN_POINT('Ctrl Pts',(-9.57754329642182,0.583102430602066,
15.6298101724592));
#14524=CARTESIAN_POINT('Ctrl Pts',(-9.65136659729214,0.293655596345324,
15.6418133592485));
#14525=CARTESIAN_POINT('Ctrl Pts',(-9.6758110331056,0.197813707971524,15.645787864934));
#14526=CARTESIAN_POINT('Ctrl Pts',(-9.6882250000001,0.0989100500913225,
15.6497623706194));
#14527=CARTESIAN_POINT('Ctrl Pts',(-9.688225,-1.14391829342253E-12,15.6537368763049));
#14528=CARTESIAN_POINT('Origin',(-8.5,0.,1.8));
#14529=CARTESIAN_POINT('',(-9.68731278632248,-0.000152542232196749,15.9962631236952));
#14530=CARTESIAN_POINT('',(-9.688225,-1.18588472375336E-12,15.9537368763049));
#14531=CARTESIAN_POINT('',(-9.688225,-1.45515594291686E-16,1.8));
#14532=CARTESIAN_POINT('Ctrl Pts',(-9.688225,5.98965321785272E-13,15.9962631236952));
#14533=CARTESIAN_POINT('Ctrl Pts',(-9.68822499999985,0.298712821306659,
15.9842599369058));
#14534=CARTESIAN_POINT('Ctrl Pts',(-9.57054245632559,0.595858078272002,
15.9722567501165));
#14535=CARTESIAN_POINT('Ctrl Pts',(-9.36601586214901,0.813569405233082,
15.9602535633272));
#14536=CARTESIAN_POINT('Ctrl Pts',(-9.16148926797243,1.03128073219416,15.9482503765379));
#14537=CARTESIAN_POINT('Ctrl Pts',(-8.87226522412804,1.16727314847148,15.9362471897486));
#14538=CARTESIAN_POINT('Ctrl Pts',(-8.57413435701411,1.18591009260192,15.9242440029593));
#14539=CARTESIAN_POINT('Ctrl Pts',(-8.27600348990018,1.20454703673237,15.9122408161699));
#14540=CARTESIAN_POINT('Ctrl Pts',(-7.97209482032065,1.10563290540095,15.9002376293806));
#14541=CARTESIAN_POINT('Ctrl Pts',(-7.7420470537204,0.915087963996402,15.8882344425913));
#14542=CARTESIAN_POINT('Ctrl Pts',(-7.51199928712015,0.724543022591854,
15.876231255802));
#14543=CARTESIAN_POINT('Ctrl Pts',(-7.35822688079628,0.444367128061277,
15.8642280690127));
#14544=CARTESIAN_POINT('Ctrl Pts',(-7.32102560975815,0.147979855990134,
15.8522248822234));
#14545=CARTESIAN_POINT('Ctrl Pts',(-7.28382433872002,-0.148407416081009,
15.840221695434));
#14546=CARTESIAN_POINT('Ctrl Pts',(-7.36358464744641,-0.457895344722041,
15.8282185086447));
#14547=CARTESIAN_POINT('Ctrl Pts',(-7.53940549437885,-0.699383189957743,
15.8162153218554));
#14548=CARTESIAN_POINT('Ctrl Pts',(-7.7152263413113,-0.940871035193445,
15.8042121350661));
#14549=CARTESIAN_POINT('Ctrl Pts',(-7.98526240565783,-1.11182427083081,
15.7922089482768));
#14550=CARTESIAN_POINT('Ctrl Pts',(-8.27875123560112,-1.16744491727746,
15.7802057614875));
#14551=CARTESIAN_POINT('Ctrl Pts',(-8.57224006554441,-1.22306556372411,
15.7682025746981));
#14552=CARTESIAN_POINT('Ctrl Pts',(-8.88610136059929,-1.16276985667027,
15.7561993879088));
#14553=CARTESIAN_POINT('Ctrl Pts',(-9.13808834820081,-1.00235817476357,
15.7441962011195));
#14554=CARTESIAN_POINT('Ctrl Pts',(-9.39007533580233,-0.841946492856875,
15.7321930143302));
#14555=CARTESIAN_POINT('Ctrl Pts',(-9.57754329642125,-0.583102430603113,
15.7201898275409));
#14556=CARTESIAN_POINT('Ctrl Pts',(-9.65136659729185,-0.293655596346466,
15.7081866407516));
#14557=CARTESIAN_POINT('Ctrl Pts',(-9.67581103310544,-0.197813707972516,
15.7042121350661));
#14558=CARTESIAN_POINT('Ctrl Pts',(-9.68822500000004,-0.0989100500921407,
15.7002376293806));
#14559=CARTESIAN_POINT('Ctrl Pts',(-9.688225,5.05817610019221E-13,15.6962631236952));
#14560=CARTESIAN_POINT('Ctrl Pts',(-9.688225,-1.14391829342253E-12,15.6537368763049));
#14561=CARTESIAN_POINT('Ctrl Pts',(-9.68822499999971,-0.298712821307226,
15.6657400630942));
#14562=CARTESIAN_POINT('Ctrl Pts',(-9.5705424563253,-0.595858078272537,
15.6777432498835));
#14563=CARTESIAN_POINT('Ctrl Pts',(-9.36601586214859,-0.813569405233528,
15.6897464366728));
#14564=CARTESIAN_POINT('Ctrl Pts',(-9.16148926797188,-1.03128073219452,
15.7017496234622));
#14565=CARTESIAN_POINT('Ctrl Pts',(-8.87226522412739,-1.16727314847169,
15.7137528102515));
#14566=CARTESIAN_POINT('Ctrl Pts',(-8.57413435701343,-1.18591009260197,
15.7257559970408));
#14567=CARTESIAN_POINT('Ctrl Pts',(-8.27600348989946,-1.20454703673224,
15.7377591838301));
#14568=CARTESIAN_POINT('Ctrl Pts',(-7.97209482031998,-1.10563290540063,
15.7497623706194));
#14569=CARTESIAN_POINT('Ctrl Pts',(-7.74204705371983,-0.915087963995925,
15.7617655574087));
#14570=CARTESIAN_POINT('Ctrl Pts',(-7.51199928711968,-0.724543022591218,
15.7737687441981));
#14571=CARTESIAN_POINT('Ctrl Pts',(-7.35822688079597,-0.444367128060516,
15.7857719309874));
#14572=CARTESIAN_POINT('Ctrl Pts',(-7.32102560975805,-0.147979855989325,
15.7977751177767));
#14573=CARTESIAN_POINT('Ctrl Pts',(-7.28382433872012,0.148407416081866,
15.809778304566));
#14574=CARTESIAN_POINT('Ctrl Pts',(-7.36358464744673,0.457895344722867,
15.8217814913553));
#14575=CARTESIAN_POINT('Ctrl Pts',(-7.53940549437938,0.699383189958457,
15.8337846781446));
#14576=CARTESIAN_POINT('Ctrl Pts',(-7.71522634131202,0.940871035194046,
15.845787864934));
#14577=CARTESIAN_POINT('Ctrl Pts',(-7.9852624056587,1.11182427083122,15.8577910517233));
#14578=CARTESIAN_POINT('Ctrl Pts',(-8.27875123560205,1.16744491727763,15.8697942385126));
#14579=CARTESIAN_POINT('Ctrl Pts',(-8.57224006554541,1.22306556372405,15.8817974253019));
#14580=CARTESIAN_POINT('Ctrl Pts',(-8.88610136060026,1.16276985666995,15.8938006120912));
#14581=CARTESIAN_POINT('Ctrl Pts',(-9.13808834820167,1.00235817476303,15.9058037988806));
#14582=CARTESIAN_POINT('Ctrl Pts',(-9.39007533580307,0.8419464928561,15.9178069856699));
#14583=CARTESIAN_POINT('Ctrl Pts',(-9.57754329642177,0.583102430602151,
15.9298101724592));
#14584=CARTESIAN_POINT('Ctrl Pts',(-9.65136659729211,0.293655596345414,
15.9418133592485));
#14585=CARTESIAN_POINT('Ctrl Pts',(-9.67581103310559,0.197813707971573,
15.945787864934));
#14586=CARTESIAN_POINT('Ctrl Pts',(-9.6882250000001,0.0989100500913255,
15.9497623706194));
#14587=CARTESIAN_POINT('Ctrl Pts',(-9.688225,-1.18588472375336E-12,15.9537368763049));
#14588=CARTESIAN_POINT('Origin',(-8.5,0.,1.8));
#14589=CARTESIAN_POINT('',(-9.68853128499928,-0.000371837973163785,16.2962631236952));
#14590=CARTESIAN_POINT('',(-9.688225,-1.16018306073329E-12,16.2537368763049));
#14591=CARTESIAN_POINT('',(-9.688225,-1.45515594291686E-16,1.8));
#14592=CARTESIAN_POINT('Ctrl Pts',(-9.68898909271114,-0.000927628473370801,
16.2962631236952));
#14593=CARTESIAN_POINT('Ctrl Pts',(-9.68618839456819,0.331830806210976,
16.28286116413));
#14594=CARTESIAN_POINT('Ctrl Pts',(-9.54051002256345,0.666783184116169,
16.2694592045648));
#14595=CARTESIAN_POINT('Ctrl Pts',(-9.29275770219925,0.88787589629704,16.2560572449997));
#14596=CARTESIAN_POINT('Ctrl Pts',(-8.99869020692162,1.1502999979143,16.240149903848));
#14597=CARTESIAN_POINT('Ctrl Pts',(-8.56081787342036,1.25231518939494,16.2242425626964));
#14598=CARTESIAN_POINT('Ctrl Pts',(-8.18138465234568,1.14687580809469,16.2083352215448));
#14599=CARTESIAN_POINT('Ctrl Pts',(-7.801951431271,1.04143642679444,16.1924278803932));
#14600=CARTESIAN_POINT('Ctrl Pts',(-7.48095732262289,0.728542472713292,
16.1765205392416));
#14601=CARTESIAN_POINT('Ctrl Pts',(-7.36353983692846,0.352071909547143,
16.1606131980899));
#14602=CARTESIAN_POINT('Ctrl Pts',(-7.30483109408124,0.163836627964079,
16.1526595275141));
#14603=CARTESIAN_POINT('Ctrl Pts',(-7.29701650697244,-0.0402928058902354,
16.1447058569383));
#14604=CARTESIAN_POINT('Ctrl Pts',(-7.33630215661051,-0.234917907606526,
16.1367521863625));
#14605=CARTESIAN_POINT('Ctrl Pts',(-7.37558780624859,-0.42954300932284,
16.1287985157867));
#14606=CARTESIAN_POINT('Ctrl Pts',(-7.46197369263355,-0.614663778901128,
16.1208448452109));
#14607=CARTESIAN_POINT('Ctrl Pts',(-7.58911134538717,-0.76538325520993,
16.1128911746351));
#14608=CARTESIAN_POINT('Ctrl Pts',(-7.84338665089437,-1.06682220782752,
16.0969838334835));
#14609=CARTESIAN_POINT('Ctrl Pts',(-8.26066902187615,-1.23065598736718,
16.0810764923318));
#14610=CARTESIAN_POINT('Ctrl Pts',(-8.65127494800788,-1.18064869785899,
16.0651691511802));
#14611=CARTESIAN_POINT('Ctrl Pts',(-9.04188087413961,-1.1306414083508,16.0492618100286));
#14612=CARTESIAN_POINT('Ctrl Pts',(-9.40581035542129,-0.866793049794769,
16.033354468877));
#14613=CARTESIAN_POINT('Ctrl Pts',(-9.57507559972748,-0.510823660624535,
16.0174471277254));
#14614=CARTESIAN_POINT('Ctrl Pts',(-9.65021314331775,-0.352807373198149,
16.0103857930486));
#14615=CARTESIAN_POINT('Ctrl Pts',(-9.6869919257318,-0.176638554687772,
16.0033244583719));
#14616=CARTESIAN_POINT('Ctrl Pts',(-9.68646940363724,-0.000293574405992758,
15.9962631236952));
#14617=CARTESIAN_POINT('Ctrl Pts',(-9.688225,-1.18588472375336E-12,15.9537368763049));
#14618=CARTESIAN_POINT('Ctrl Pts',(-9.6882249999997,-0.298712821307291,
15.9657400630942));
#14619=CARTESIAN_POINT('Ctrl Pts',(-9.57054245632526,-0.595858078272619,
15.9777432498835));
#14620=CARTESIAN_POINT('Ctrl Pts',(-9.36601586214851,-0.813569405233608,
15.9897464366728));
#14621=CARTESIAN_POINT('Ctrl Pts',(-9.16148926797177,-1.0312807321946,16.0017496234622));
#14622=CARTESIAN_POINT('Ctrl Pts',(-8.87226522412724,-1.16727314847175,
16.0137528102515));
#14623=CARTESIAN_POINT('Ctrl Pts',(-8.57413435701325,-1.18591009260198,
16.0257559970408));
#14624=CARTESIAN_POINT('Ctrl Pts',(-8.27600348989926,-1.20454703673221,
16.0377591838301));
#14625=CARTESIAN_POINT('Ctrl Pts',(-7.97209482031977,-1.10563290540054,
16.0497623706194));
#14626=CARTESIAN_POINT('Ctrl Pts',(-7.74204705371964,-0.915087963995769,
16.0617655574088));
#14627=CARTESIAN_POINT('Ctrl Pts',(-7.51199928711951,-0.724543022591,16.0737687441981));
#14628=CARTESIAN_POINT('Ctrl Pts',(-7.35822688079586,-0.444367128060239,
16.0857719309874));
#14629=CARTESIAN_POINT('Ctrl Pts',(-7.32102560975801,-0.147979855989016,
16.0977751177767));
#14630=CARTESIAN_POINT('Ctrl Pts',(-7.28382433872016,0.148407416082207,
16.109778304566));
#14631=CARTESIAN_POINT('Ctrl Pts',(-7.36358464744687,0.457895344723212,
16.1217814913553));
#14632=CARTESIAN_POINT('Ctrl Pts',(-7.5394054943796,0.699383189958763,16.1337846781447));
#14633=CARTESIAN_POINT('Ctrl Pts',(-7.71522634131233,0.940871035194315,
16.145787864934));
#14634=CARTESIAN_POINT('Ctrl Pts',(-7.98526240565909,1.11182427083141,16.1577910517233));
#14635=CARTESIAN_POINT('Ctrl Pts',(-8.27875123560249,1.16744491727772,16.1697942385126));
#14636=CARTESIAN_POINT('Ctrl Pts',(-8.5722400655459,1.22306556372403,16.1817974253019));
#14637=CARTESIAN_POINT('Ctrl Pts',(-8.88610136060075,1.1627698566698,16.1938006120913));
#14638=CARTESIAN_POINT('Ctrl Pts',(-9.1380883482021,1.00235817476275,16.2058037988806));
#14639=CARTESIAN_POINT('Ctrl Pts',(-9.39007533580346,0.841946492855702,
16.2178069856699));
#14640=CARTESIAN_POINT('Ctrl Pts',(-9.57754329642206,0.583102430601644,
16.2298101724592));
#14641=CARTESIAN_POINT('Ctrl Pts',(-9.65136659729226,0.29365559634485,16.2418133592485));
#14642=CARTESIAN_POINT('Ctrl Pts',(-9.67581103310564,0.197813707971193,
16.245787864934));
#14643=CARTESIAN_POINT('Ctrl Pts',(-9.6882250000001,0.0989100500911486,
16.2497623706194));
#14644=CARTESIAN_POINT('Ctrl Pts',(-9.688225,-1.16018306073329E-12,16.2537368763049));
#14645=CARTESIAN_POINT('Origin',(-8.5,0.,1.8));
#14646=CARTESIAN_POINT('',(-9.688225,5.82645043323282E-13,16.5962631236952));
#14647=CARTESIAN_POINT('',(-9.688225,-1.13453690886445E-12,16.5537368763049));
#14648=CARTESIAN_POINT('',(-9.688225,-1.45515594291686E-16,1.8));
#14649=CARTESIAN_POINT('Ctrl Pts',(-9.688225,5.82645043323282E-13,16.5962631236952));
#14650=CARTESIAN_POINT('Ctrl Pts',(-9.68822499999986,0.298712821306687,
16.5842599369058));
#14651=CARTESIAN_POINT('Ctrl Pts',(-9.57054245632556,0.595858078272076,
16.5722567501165));
#14652=CARTESIAN_POINT('Ctrl Pts',(-9.36601586214893,0.813569405233169,
16.5602535633272));
#14653=CARTESIAN_POINT('Ctrl Pts',(-9.16148926797229,1.03128073219426,16.5482503765379));
#14654=CARTESIAN_POINT('Ctrl Pts',(-8.87226522412784,1.16727314847156,16.5362471897486));
#14655=CARTESIAN_POINT('Ctrl Pts',(-8.57413435701386,1.18591009260194,16.5242440029592));
#14656=CARTESIAN_POINT('Ctrl Pts',(-8.27600348989987,1.20454703673232,16.5122408161699));
#14657=CARTESIAN_POINT('Ctrl Pts',(-7.97209482032033,1.10563290540081,16.5002376293806));
#14658=CARTESIAN_POINT('Ctrl Pts',(-7.7420470537201,0.915087963996154,16.4882344425913));
#14659=CARTESIAN_POINT('Ctrl Pts',(-7.51199928711988,0.724543022591502,
16.476231255802));
#14660=CARTESIAN_POINT('Ctrl Pts',(-7.35822688079609,0.444367128060818,
16.4642280690127));
#14661=CARTESIAN_POINT('Ctrl Pts',(-7.32102560975809,0.147979855989614,
16.4522248822233));
#14662=CARTESIAN_POINT('Ctrl Pts',(-7.28382433872008,-0.14840741608159,
16.440221695434));
#14663=CARTESIAN_POINT('Ctrl Pts',(-7.36358464744663,-0.457895344722635,
16.4282185086447));
#14664=CARTESIAN_POINT('Ctrl Pts',(-7.53940549437924,-0.699383189958276,
16.4162153218554));
#14665=CARTESIAN_POINT('Ctrl Pts',(-7.71522634131185,-0.940871035193917,
16.4042121350661));
#14666=CARTESIAN_POINT('Ctrl Pts',(-7.98526240565853,-1.11182427083114,
16.3922089482767));
#14667=CARTESIAN_POINT('Ctrl Pts',(-8.2787512356019,-1.16744491727761,16.3802057614874));
#14668=CARTESIAN_POINT('Ctrl Pts',(-8.57224006554527,-1.22306556372407,
16.3682025746981));
#14669=CARTESIAN_POINT('Ctrl Pts',(-8.88610136060016,-1.16276985666999,
16.3561993879088));
#14670=CARTESIAN_POINT('Ctrl Pts',(-9.13808834820159,-1.00235817476307,
16.3441962011195));
#14671=CARTESIAN_POINT('Ctrl Pts',(-9.39007533580303,-0.841946492856155,
16.3321930143302));
#14672=CARTESIAN_POINT('Ctrl Pts',(-9.57754329642176,-0.583102430602191,
16.3201898275408));
#14673=CARTESIAN_POINT('Ctrl Pts',(-9.65136659729211,-0.293655596345434,
16.3081866407515));
#14674=CARTESIAN_POINT('Ctrl Pts',(-9.67581103310554,-0.197813707971768,
16.3042121350661));
#14675=CARTESIAN_POINT('Ctrl Pts',(-9.68822500000005,-0.0989100500917069,
16.3002376293806));
#14676=CARTESIAN_POINT('Ctrl Pts',(-9.688225,6.24500451351651E-13,16.2962631236952));
#14677=CARTESIAN_POINT('Ctrl Pts',(-9.688225,-1.16018306073329E-12,16.2537368763049));
#14678=CARTESIAN_POINT('Ctrl Pts',(-9.68822499999971,-0.298712821307242,
16.2657400630942));
#14679=CARTESIAN_POINT('Ctrl Pts',(-9.57054245632529,-0.595858078272552,
16.2777432498835));
#14680=CARTESIAN_POINT('Ctrl Pts',(-9.36601586214858,-0.81356940523354,
16.2897464366728));
#14681=CARTESIAN_POINT('Ctrl Pts',(-9.16148926797187,-1.03128073219453,
16.3017496234622));
#14682=CARTESIAN_POINT('Ctrl Pts',(-8.87226522412738,-1.1672731484717,16.3137528102515));
#14683=CARTESIAN_POINT('Ctrl Pts',(-8.57413435701341,-1.18591009260197,
16.3257559970408));
#14684=CARTESIAN_POINT('Ctrl Pts',(-8.27600348989945,-1.20454703673224,
16.3377591838301));
#14685=CARTESIAN_POINT('Ctrl Pts',(-7.97209482031996,-1.10563290540062,
16.3497623706194));
#14686=CARTESIAN_POINT('Ctrl Pts',(-7.74204705371982,-0.915087963995914,
16.3617655574087));
#14687=CARTESIAN_POINT('Ctrl Pts',(-7.51199928711967,-0.724543022591205,
16.3737687441981));
#14688=CARTESIAN_POINT('Ctrl Pts',(-7.35822688079597,-0.4443671280605,16.3857719309874));
#14689=CARTESIAN_POINT('Ctrl Pts',(-7.32102560975805,-0.147979855989309,
16.3977751177767));
#14690=CARTESIAN_POINT('Ctrl Pts',(-7.28382433872013,0.148407416081883,
16.409778304566));
#14691=CARTESIAN_POINT('Ctrl Pts',(-7.36358464744674,0.457895344722883,
16.4217814913553));
#14692=CARTESIAN_POINT('Ctrl Pts',(-7.53940549437938,0.69938318995847,16.4337846781446));
#14693=CARTESIAN_POINT('Ctrl Pts',(-7.71522634131203,0.940871035194057,
16.445787864934));
#14694=CARTESIAN_POINT('Ctrl Pts',(-7.98526240565871,1.11182427083122,16.4577910517233));
#14695=CARTESIAN_POINT('Ctrl Pts',(-8.27875123560207,1.16744491727764,16.4697942385126));
#14696=CARTESIAN_POINT('Ctrl Pts',(-8.57224006554543,1.22306556372405,16.4817974253019));
#14697=CARTESIAN_POINT('Ctrl Pts',(-8.88610136060028,1.16276985666995,16.4938006120912));
#14698=CARTESIAN_POINT('Ctrl Pts',(-9.13808834820168,1.00235817476302,16.5058037988806));
#14699=CARTESIAN_POINT('Ctrl Pts',(-9.39007533580308,0.841946492856088,
16.5178069856699));
#14700=CARTESIAN_POINT('Ctrl Pts',(-9.57754329642178,0.583102430602136,
16.5298101724592));
#14701=CARTESIAN_POINT('Ctrl Pts',(-9.65136659729212,0.293655596345398,
16.5418133592485));
#14702=CARTESIAN_POINT('Ctrl Pts',(-9.67581103310558,0.1978137079716,16.545787864934));
#14703=CARTESIAN_POINT('Ctrl Pts',(-9.68822500000009,0.0989100500913994,
16.5497623706194));
#14704=CARTESIAN_POINT('Ctrl Pts',(-9.688225,-1.06703534896724E-12,16.5537368763049));
#14705=CARTESIAN_POINT('Origin',(-8.5,0.,1.8));
#14706=CARTESIAN_POINT('',(-9.688225,6.08291195192123E-13,16.8962631236952));
#14707=CARTESIAN_POINT('',(-9.688225,-1.10900177929807E-12,16.8537368763049));
#14708=CARTESIAN_POINT('',(-9.688225,-1.45515594291686E-16,1.8));
#14709=CARTESIAN_POINT('Ctrl Pts',(-9.688225,5.40789635294914E-13,16.8962631236952));
#14710=CARTESIAN_POINT('Ctrl Pts',(-9.68822499999986,0.298712821306646,
16.8842599369058));
#14711=CARTESIAN_POINT('Ctrl Pts',(-9.57054245632558,0.595858078272038,
16.8722567501165));
#14712=CARTESIAN_POINT('Ctrl Pts',(-9.36601586214896,0.813569405233138,
16.8602535633272));
#14713=CARTESIAN_POINT('Ctrl Pts',(-9.16148926797233,1.03128073219424,16.8482503765379));
#14714=CARTESIAN_POINT('Ctrl Pts',(-8.87226522412788,1.16727314847155,16.8362471897486));
#14715=CARTESIAN_POINT('Ctrl Pts',(-8.5741343570139,1.18591009260194,16.8242440029592));
#14716=CARTESIAN_POINT('Ctrl Pts',(-8.27600348989992,1.20454703673233,16.8122408161699));
#14717=CARTESIAN_POINT('Ctrl Pts',(-7.97209482032037,1.10563290540082,16.8002376293806));
#14718=CARTESIAN_POINT('Ctrl Pts',(-7.74204705372014,0.915087963996181,
16.7882344425913));
#14719=CARTESIAN_POINT('Ctrl Pts',(-7.51199928711991,0.724543022591537,
16.776231255802));
#14720=CARTESIAN_POINT('Ctrl Pts',(-7.3582268807961,0.444367128060859,16.7642280690127));
#14721=CARTESIAN_POINT('Ctrl Pts',(-7.32102560975809,0.147979855989656,
16.7522248822233));
#14722=CARTESIAN_POINT('Ctrl Pts',(-7.28382433872008,-0.148407416081547,
16.740221695434));
#14723=CARTESIAN_POINT('Ctrl Pts',(-7.36358464744662,-0.457895344722595,
16.7282185086447));
#14724=CARTESIAN_POINT('Ctrl Pts',(-7.53940549437922,-0.699383189958242,
16.7162153218554));
#14725=CARTESIAN_POINT('Ctrl Pts',(-7.71522634131182,-0.940871035193889,
16.7042121350661));
#14726=CARTESIAN_POINT('Ctrl Pts',(-7.98526240565849,-1.11182427083113,
16.6922089482767));
#14727=CARTESIAN_POINT('Ctrl Pts',(-8.27875123560186,-1.1674449172776,16.6802057614874));
#14728=CARTESIAN_POINT('Ctrl Pts',(-8.57224006554523,-1.22306556372407,
16.6682025746981));
#14729=CARTESIAN_POINT('Ctrl Pts',(-8.88610136060012,-1.16276985667001,
16.6561993879088));
#14730=CARTESIAN_POINT('Ctrl Pts',(-9.13808834820156,-1.0023581747631,16.6441962011195));
#14731=CARTESIAN_POINT('Ctrl Pts',(-9.390075335803,-0.841946492856186,16.6321930143302));
#14732=CARTESIAN_POINT('Ctrl Pts',(-9.57754329642174,-0.58310243060223,
16.6201898275408));
#14733=CARTESIAN_POINT('Ctrl Pts',(-9.6513665972921,-0.293655596345475,
16.6081866407515));
#14734=CARTESIAN_POINT('Ctrl Pts',(-9.67581103310554,-0.19781370797181,
16.6042121350661));
#14735=CARTESIAN_POINT('Ctrl Pts',(-9.68822500000005,-0.0989100500917488,
16.6002376293806));
#14736=CARTESIAN_POINT('Ctrl Pts',(-9.688225,5.82645043323282E-13,16.5962631236952));
#14737=CARTESIAN_POINT('Ctrl Pts',(-9.688225,-1.06703534896724E-12,16.5537368763049));
#14738=CARTESIAN_POINT('Ctrl Pts',(-9.68822499999973,-0.298712821307149,
16.5657400630942));
#14739=CARTESIAN_POINT('Ctrl Pts',(-9.57054245632533,-0.595858078272468,
16.5777432498835));
#14740=CARTESIAN_POINT('Ctrl Pts',(-9.36601586214864,-0.813569405233472,
16.5897464366728));
#14741=CARTESIAN_POINT('Ctrl Pts',(-9.16148926797195,-1.03128073219448,
16.6017496234622));
#14742=CARTESIAN_POINT('Ctrl Pts',(-8.87226522412747,-1.16727314847167,
16.6137528102515));
#14743=CARTESIAN_POINT('Ctrl Pts',(-8.57413435701351,-1.18591009260196,
16.6257559970408));
#14744=CARTESIAN_POINT('Ctrl Pts',(-8.27600348989954,-1.20454703673225,
16.6377591838301));
#14745=CARTESIAN_POINT('Ctrl Pts',(-7.97209482032005,-1.10563290540067,
16.6497623706194));
#14746=CARTESIAN_POINT('Ctrl Pts',(-7.74204705371989,-0.915087963995974,
16.6617655574087));
#14747=CARTESIAN_POINT('Ctrl Pts',(-7.51199928711973,-0.724543022591282,
16.6737687441981));
#14748=CARTESIAN_POINT('Ctrl Pts',(-7.358226880796,-0.44436712806059,16.6857719309874));
#14749=CARTESIAN_POINT('Ctrl Pts',(-7.32102560975806,-0.147979855989401,
16.6977751177767));
#14750=CARTESIAN_POINT('Ctrl Pts',(-7.28382433872012,0.148407416081787,
16.709778304566));
#14751=CARTESIAN_POINT('Ctrl Pts',(-7.3635846474467,0.457895344722794,16.7217814913553));
#14752=CARTESIAN_POINT('Ctrl Pts',(-7.53940549437933,0.699383189958394,
16.7337846781446));
#14753=CARTESIAN_POINT('Ctrl Pts',(-7.71522634131196,0.940871035193995,
16.745787864934));
#14754=CARTESIAN_POINT('Ctrl Pts',(-7.98526240565862,1.11182427083118,16.7577910517233));
#14755=CARTESIAN_POINT('Ctrl Pts',(-8.27875123560198,1.16744491727762,16.7697942385126));
#14756=CARTESIAN_POINT('Ctrl Pts',(-8.57224006554533,1.22306556372406,16.7817974253019));
#14757=CARTESIAN_POINT('Ctrl Pts',(-8.88610136060019,1.16276985666998,16.7938006120912));
#14758=CARTESIAN_POINT('Ctrl Pts',(-9.1380883482016,1.00235817476307,16.8058037988806));
#14759=CARTESIAN_POINT('Ctrl Pts',(-9.39007533580302,0.841946492856158,
16.8178069856699));
#14760=CARTESIAN_POINT('Ctrl Pts',(-9.57754329642174,0.58310243060222,16.8298101724592));
#14761=CARTESIAN_POINT('Ctrl Pts',(-9.65136659729209,0.293655596345488,
16.8418133592485));
#14762=CARTESIAN_POINT('Ctrl Pts',(-9.67581103310557,0.197813707971671,
16.845787864934));
#14763=CARTESIAN_POINT('Ctrl Pts',(-9.68822500000009,0.0989100500914474,
16.8497623706194));
#14764=CARTESIAN_POINT('Ctrl Pts',(-9.688225,-1.04144470824963E-12,16.8537368763049));
#14765=CARTESIAN_POINT('Origin',(-8.5,0.,1.8));
#14766=CARTESIAN_POINT('',(-9.688225,6.33826324758502E-13,17.1962631236952));
#14767=CARTESIAN_POINT('',(-9.688225,-1.083300116278E-12,17.1537368763049));
#14768=CARTESIAN_POINT('',(-9.688225,-1.45515594291686E-16,1.8));
#14769=CARTESIAN_POINT('Ctrl Pts',(-9.688225,6.33826324758502E-13,17.1962631236952));
#14770=CARTESIAN_POINT('Ctrl Pts',(-9.68822499999984,0.298712821306739,
17.1842599369058));
#14771=CARTESIAN_POINT('Ctrl Pts',(-9.57054245632553,0.595858078272122,
17.1722567501165));
#14772=CARTESIAN_POINT('Ctrl Pts',(-9.36601586214889,0.813569405233206,
17.1602535633272));
#14773=CARTESIAN_POINT('Ctrl Pts',(-9.16148926797225,1.03128073219429,17.1482503765379));
#14774=CARTESIAN_POINT('Ctrl Pts',(-8.87226522412779,1.16727314847158,17.1362471897486));
#14775=CARTESIAN_POINT('Ctrl Pts',(-8.5741343570138,1.18591009260194,17.1242440029592));
#14776=CARTESIAN_POINT('Ctrl Pts',(-8.27600348989982,1.20454703673231,17.1122408161699));
#14777=CARTESIAN_POINT('Ctrl Pts',(-7.97209482032028,1.10563290540078,17.1002376293806));
#14778=CARTESIAN_POINT('Ctrl Pts',(-7.74204705372006,0.915087963996121,
17.0882344425913));
#14779=CARTESIAN_POINT('Ctrl Pts',(-7.51199928711985,0.72454302259146,17.076231255802));
#14780=CARTESIAN_POINT('Ctrl Pts',(-7.35822688079607,0.444367128060769,
17.0642280690127));
#14781=CARTESIAN_POINT('Ctrl Pts',(-7.32102560975808,0.147979855989563,
17.0522248822233));
#14782=CARTESIAN_POINT('Ctrl Pts',(-7.28382433872009,-0.148407416081643,
17.040221695434));
#14783=CARTESIAN_POINT('Ctrl Pts',(-7.36358464744665,-0.457895344722684,
17.0282185086447));
#14784=CARTESIAN_POINT('Ctrl Pts',(-7.53940549437927,-0.699383189958317,
17.0162153218554));
#14785=CARTESIAN_POINT('Ctrl Pts',(-7.71522634131189,-0.94087103519395,
17.0042121350661));
#14786=CARTESIAN_POINT('Ctrl Pts',(-7.98526240565858,-1.11182427083117,
16.9922089482767));
#14787=CARTESIAN_POINT('Ctrl Pts',(-8.27875123560195,-1.16744491727762,
16.9802057614874));
#14788=CARTESIAN_POINT('Ctrl Pts',(-8.57224006554533,-1.22306556372406,
16.9682025746981));
#14789=CARTESIAN_POINT('Ctrl Pts',(-8.88610136060021,-1.16276985666998,
16.9561993879088));
#14790=CARTESIAN_POINT('Ctrl Pts',(-9.13808834820164,-1.00235817476305,
16.9441962011195));
#14791=CARTESIAN_POINT('Ctrl Pts',(-9.39007533580307,-0.841946492856116,
16.9321930143301));
#14792=CARTESIAN_POINT('Ctrl Pts',(-9.57754329642178,-0.583102430602145,
16.9201898275408));
#14793=CARTESIAN_POINT('Ctrl Pts',(-9.65136659729212,-0.293655596345385,
16.9081866407515));
#14794=CARTESIAN_POINT('Ctrl Pts',(-9.67581103310554,-0.197813707971761,
16.9042121350661));
#14795=CARTESIAN_POINT('Ctrl Pts',(-9.68822500000005,-0.0989100500917455,
16.9002376293806));
#14796=CARTESIAN_POINT('Ctrl Pts',(-9.688225,5.40789635294914E-13,16.8962631236952));
#14797=CARTESIAN_POINT('Ctrl Pts',(-9.688225,-1.04144470824963E-12,16.8537368763049));
#14798=CARTESIAN_POINT('Ctrl Pts',(-9.68822499999974,-0.298712821307124,
16.8657400630942));
#14799=CARTESIAN_POINT('Ctrl Pts',(-9.57054245632535,-0.595858078272445,
16.8777432498835));
#14800=CARTESIAN_POINT('Ctrl Pts',(-9.36601586214866,-0.813569405233454,
16.8897464366728));
#14801=CARTESIAN_POINT('Ctrl Pts',(-9.16148926797197,-1.03128073219446,
16.9017496234622));
#14802=CARTESIAN_POINT('Ctrl Pts',(-8.8722652241275,-1.16727314847166,16.9137528102515));
#14803=CARTESIAN_POINT('Ctrl Pts',(-8.57413435701353,-1.18591009260196,
16.9257559970408));
#14804=CARTESIAN_POINT('Ctrl Pts',(-8.27600348989957,-1.20454703673226,
16.9377591838301));
#14805=CARTESIAN_POINT('Ctrl Pts',(-7.97209482032007,-1.10563290540068,
16.9497623706194));
#14806=CARTESIAN_POINT('Ctrl Pts',(-7.74204705371991,-0.91508796399599,
16.9617655574087));
#14807=CARTESIAN_POINT('Ctrl Pts',(-7.51199928711974,-0.724543022591304,
16.9737687441981));
#14808=CARTESIAN_POINT('Ctrl Pts',(-7.35822688079601,-0.444367128060615,
16.9857719309874));
#14809=CARTESIAN_POINT('Ctrl Pts',(-7.32102560975806,-0.147979855989427,
16.9977751177767));
#14810=CARTESIAN_POINT('Ctrl Pts',(-7.28382433872011,0.148407416081761,
17.009778304566));
#14811=CARTESIAN_POINT('Ctrl Pts',(-7.36358464744669,0.457895344722769,
17.0217814913553));
#14812=CARTESIAN_POINT('Ctrl Pts',(-7.53940549437931,0.699383189958374,
17.0337846781446));
#14813=CARTESIAN_POINT('Ctrl Pts',(-7.71522634131194,0.940871035193978,
17.045787864934));
#14814=CARTESIAN_POINT('Ctrl Pts',(-7.9852624056586,1.11182427083117,17.0577910517233));
#14815=CARTESIAN_POINT('Ctrl Pts',(-8.27875123560195,1.16744491727762,17.0697942385126));
#14816=CARTESIAN_POINT('Ctrl Pts',(-8.57224006554531,1.22306556372406,17.0817974253019));
#14817=CARTESIAN_POINT('Ctrl Pts',(-8.88610136060016,1.16276985666999,17.0938006120912));
#14818=CARTESIAN_POINT('Ctrl Pts',(-9.13808834820158,1.00235817476308,17.1058037988805));
#14819=CARTESIAN_POINT('Ctrl Pts',(-9.390075335803,0.841946492856177,17.1178069856699));
#14820=CARTESIAN_POINT('Ctrl Pts',(-9.57754329642172,0.583102430602244,
17.1298101724592));
#14821=CARTESIAN_POINT('Ctrl Pts',(-9.65136659729209,0.293655596345513,
17.1418133592485));
#14822=CARTESIAN_POINT('Ctrl Pts',(-9.67581103310557,0.197813707971696,
17.145787864934));
#14823=CARTESIAN_POINT('Ctrl Pts',(-9.68822500000008,0.0989100500914731,
17.1497623706194));
#14824=CARTESIAN_POINT('Ctrl Pts',(-9.688225,-1.01579855638079E-12,17.1537368763049));
#14825=CARTESIAN_POINT('Origin',(-8.5,0.,1.8));
#14826=CARTESIAN_POINT('',(-9.688225,6.59472476627343E-13,17.4962631236952));
#14827=CARTESIAN_POINT('',(-9.68910276879127,0.000129087185285244,17.4537368763049));
#14828=CARTESIAN_POINT('',(-9.688225,-1.45515594291686E-16,1.8));
#14829=CARTESIAN_POINT('Ctrl Pts',(-9.688225,6.59472476627343E-13,17.4962631236952));
#14830=CARTESIAN_POINT('Ctrl Pts',(-9.68822499999984,0.298712821306742,
17.4842599369058));
#14831=CARTESIAN_POINT('Ctrl Pts',(-9.57054245632554,0.595858078272101,
17.4722567501165));
#14832=CARTESIAN_POINT('Ctrl Pts',(-9.36601586214892,0.813569405233176,
17.4602535633272));
#14833=CARTESIAN_POINT('Ctrl Pts',(-9.1614892679723,1.03128073219425,17.4482503765379));
#14834=CARTESIAN_POINT('Ctrl Pts',(-8.87226522412787,1.16727314847154,17.4362471897486));
#14835=CARTESIAN_POINT('Ctrl Pts',(-8.57413435701391,1.18591009260194,17.4242440029592));
#14836=CARTESIAN_POINT('Ctrl Pts',(-8.27600348989995,1.20454703673233,17.4122408161699));
#14837=CARTESIAN_POINT('Ctrl Pts',(-7.97209482032043,1.10563290540085,17.4002376293806));
#14838=CARTESIAN_POINT('Ctrl Pts',(-7.7420470537202,0.915087963996234,17.3882344425913));
#14839=CARTESIAN_POINT('Ctrl Pts',(-7.51199928711998,0.724543022591621,
17.376231255802));
#14840=CARTESIAN_POINT('Ctrl Pts',(-7.35822688079616,0.444367128060982,
17.3642280690127));
#14841=CARTESIAN_POINT('Ctrl Pts',(-7.32102560975811,0.147979855989806,
17.3522248822233));
#14842=CARTESIAN_POINT('Ctrl Pts',(-7.28382433872006,-0.14840741608137,
17.340221695434));
#14843=CARTESIAN_POINT('Ctrl Pts',(-7.36358464744655,-0.457895344722404,
17.3282185086447));
#14844=CARTESIAN_POINT('Ctrl Pts',(-7.53940549437909,-0.699383189958065,
17.3162153218554));
#14845=CARTESIAN_POINT('Ctrl Pts',(-7.71522634131163,-0.940871035193726,
17.3042121350661));
#14846=CARTESIAN_POINT('Ctrl Pts',(-7.98526240565824,-1.11182427083101,
17.2922089482768));
#14847=CARTESIAN_POINT('Ctrl Pts',(-8.27875123560158,-1.16744491727754,
17.2802057614874));
#14848=CARTESIAN_POINT('Ctrl Pts',(-8.57224006554492,-1.22306556372408,
17.2682025746981));
#14849=CARTESIAN_POINT('Ctrl Pts',(-8.88610136059979,-1.16276985667011,
17.2561993879088));
#14850=CARTESIAN_POINT('Ctrl Pts',(-9.13808834820126,-1.00235817476329,
17.2441962011195));
#14851=CARTESIAN_POINT('Ctrl Pts',(-9.39007533580273,-0.841946492856463,
17.2321930143302));
#14852=CARTESIAN_POINT('Ctrl Pts',(-9.57754329642154,-0.58310243060259,
17.2201898275409));
#14853=CARTESIAN_POINT('Ctrl Pts',(-9.65136659729199,-0.293655596345883,
17.2081866407515));
#14854=CARTESIAN_POINT('Ctrl Pts',(-9.67581103310551,-0.197813707972074,
17.2042121350661));
#14855=CARTESIAN_POINT('Ctrl Pts',(-9.68822500000005,-0.0989100500918551,
17.2002376293806));
#14856=CARTESIAN_POINT('Ctrl Pts',(-9.688225,6.33826324758502E-13,17.1962631236952));
#14857=CARTESIAN_POINT('Ctrl Pts',(-9.688225,-1.01579855638079E-12,17.1537368763049));
#14858=CARTESIAN_POINT('Ctrl Pts',(-9.68822499999974,-0.298712821307098,
17.1657400630942));
#14859=CARTESIAN_POINT('Ctrl Pts',(-9.57054245632536,-0.595858078272422,
17.1777432498835));
#14860=CARTESIAN_POINT('Ctrl Pts',(-9.36601586214868,-0.813569405233435,
17.1897464366728));
#14861=CARTESIAN_POINT('Ctrl Pts',(-9.16148926797199,-1.03128073219445,
17.2017496234622));
#14862=CARTESIAN_POINT('Ctrl Pts',(-8.87226522412752,-1.16727314847165,
17.2137528102515));
#14863=CARTESIAN_POINT('Ctrl Pts',(-8.57413435701356,-1.18591009260196,
17.2257559970408));
#14864=CARTESIAN_POINT('Ctrl Pts',(-8.27600348989959,-1.20454703673226,
17.2377591838301));
#14865=CARTESIAN_POINT('Ctrl Pts',(-7.9720948203201,-1.10563290540069,17.2497623706194));
#14866=CARTESIAN_POINT('Ctrl Pts',(-7.74204705371993,-0.915087963996007,
17.2617655574087));
#14867=CARTESIAN_POINT('Ctrl Pts',(-7.51199928711976,-0.724543022591325,
17.2737687441981));
#14868=CARTESIAN_POINT('Ctrl Pts',(-7.35822688079602,-0.444367128060639,
17.2857719309874));
#14869=CARTESIAN_POINT('Ctrl Pts',(-7.32102560975807,-0.147979855989452,
17.2977751177767));
#14870=CARTESIAN_POINT('Ctrl Pts',(-7.28382433872011,0.148407416081735,
17.309778304566));
#14871=CARTESIAN_POINT('Ctrl Pts',(-7.36358464744668,0.457895344722745,
17.3217814913553));
#14872=CARTESIAN_POINT('Ctrl Pts',(-7.5394054943793,0.699383189958353,17.3337846781446));
#14873=CARTESIAN_POINT('Ctrl Pts',(-7.71522634131192,0.940871035193961,
17.345787864934));
#14874=CARTESIAN_POINT('Ctrl Pts',(-7.98526240565858,1.11182427083116,17.3577910517233));
#14875=CARTESIAN_POINT('Ctrl Pts',(-8.27875123560193,1.16744491727761,17.3697942385126));
#14876=CARTESIAN_POINT('Ctrl Pts',(-8.57224006554528,1.22306556372406,17.3817974253019));
#14877=CARTESIAN_POINT('Ctrl Pts',(-8.88610136060014,1.16276985667,17.3938006120912));
#14878=CARTESIAN_POINT('Ctrl Pts',(-9.13808834820156,1.0023581747631,17.4058037988805));
#14879=CARTESIAN_POINT('Ctrl Pts',(-9.39007533580298,0.841946492856196,
17.4178069856699));
#14880=CARTESIAN_POINT('Ctrl Pts',(-9.57754329642171,0.583102430602267,
17.4298101724592));
#14881=CARTESIAN_POINT('Ctrl Pts',(-9.65136659729208,0.293655596345538,
17.4418133592485));
#14882=CARTESIAN_POINT('Ctrl Pts',(-9.67581103310557,0.1978137079717,17.445787864934));
#14883=CARTESIAN_POINT('Ctrl Pts',(-9.68822500000009,0.0989100500914538,
17.4497623706194));
#14884=CARTESIAN_POINT('Ctrl Pts',(-9.688225,-1.05770947556039E-12,17.4537368763049));
#14885=CARTESIAN_POINT('Origin',(-8.5,0.,1.8));
#14886=CARTESIAN_POINT('',(-9.688225,6.85118628496184E-13,17.7962631236952));
#14887=CARTESIAN_POINT('',(-9.68776597122061,0.000508313949723295,17.7537368763049));
#14888=CARTESIAN_POINT('',(-9.688225,-1.45515594291686E-16,1.8));
#14889=CARTESIAN_POINT('Ctrl Pts',(-9.688225,6.85118628496184E-13,17.7962631236952));
#14890=CARTESIAN_POINT('Ctrl Pts',(-9.68822499999983,0.298712821306812,
17.7842599369058));
#14891=CARTESIAN_POINT('Ctrl Pts',(-9.57054245632549,0.595858078272213,
17.7722567501165));
#14892=CARTESIAN_POINT('Ctrl Pts',(-9.36601586214881,0.813569405233293,
17.7602535633272));
#14893=CARTESIAN_POINT('Ctrl Pts',(-9.16148926797213,1.03128073219437,17.7482503765379));
#14894=CARTESIAN_POINT('Ctrl Pts',(-8.87226522412762,1.16727314847163,17.7362471897486));
#14895=CARTESIAN_POINT('Ctrl Pts',(-8.57413435701362,1.18591009260196,17.7242440029592));
#14896=CARTESIAN_POINT('Ctrl Pts',(-8.27600348989961,1.20454703673228,17.7122408161699));
#14897=CARTESIAN_POINT('Ctrl Pts',(-7.97209482032006,1.10563290540068,17.7002376293806));
#14898=CARTESIAN_POINT('Ctrl Pts',(-7.74204705371987,0.915087963995959,
17.6882344425913));
#14899=CARTESIAN_POINT('Ctrl Pts',(-7.51199928711968,0.724543022591234,
17.676231255802));
#14900=CARTESIAN_POINT('Ctrl Pts',(-7.35822688079595,0.444367128060483,
17.6642280690126));
#14901=CARTESIAN_POINT('Ctrl Pts',(-7.32102560975804,0.147979855989244,
17.6522248822233));
#14902=CARTESIAN_POINT('Ctrl Pts',(-7.28382433872013,-0.148407416081994,
17.640221695434));
#14903=CARTESIAN_POINT('Ctrl Pts',(-7.36358464744679,-0.457895344723038,
17.6282185086447));
#14904=CARTESIAN_POINT('Ctrl Pts',(-7.5394054943795,-0.699383189958632,
17.6162153218554));
#14905=CARTESIAN_POINT('Ctrl Pts',(-7.71522634131221,-0.940871035194226,
17.604212135066));
#14906=CARTESIAN_POINT('Ctrl Pts',(-7.98526240565898,-1.11182427083136,
17.5922089482767));
#14907=CARTESIAN_POINT('Ctrl Pts',(-8.2787512356024,-1.1674449172777,17.5802057614874));
#14908=CARTESIAN_POINT('Ctrl Pts',(-8.57224006554582,-1.22306556372404,
17.5682025746981));
#14909=CARTESIAN_POINT('Ctrl Pts',(-8.8861013606007,-1.16276985666982,17.5561993879088));
#14910=CARTESIAN_POINT('Ctrl Pts',(-9.13808834820208,-1.00235817476277,
17.5441962011194));
#14911=CARTESIAN_POINT('Ctrl Pts',(-9.39007533580346,-0.841946492855711,
17.5321930143301));
#14912=CARTESIAN_POINT('Ctrl Pts',(-9.57754329642207,-0.58310243060163,
17.5201898275408));
#14913=CARTESIAN_POINT('Ctrl Pts',(-9.65136659729227,-0.293655596344811,
17.5081866407515));
#14914=CARTESIAN_POINT('Ctrl Pts',(-9.6758110331056,-0.197813707971328,
17.504212135066));
#14915=CARTESIAN_POINT('Ctrl Pts',(-9.68822500000006,-0.0989100500914692,
17.5002376293806));
#14916=CARTESIAN_POINT('Ctrl Pts',(-9.688225,6.59472476627343E-13,17.4962631236952));
#14917=CARTESIAN_POINT('Ctrl Pts',(-9.69026320655127,0.00029974448077278,
17.4537368763049));
#14918=CARTESIAN_POINT('Ctrl Pts',(-9.68955486729688,-0.386329465614491,
17.4693398230865));
#14919=CARTESIAN_POINT('Ctrl Pts',(-9.48339361754863,-0.77397925042195,
17.4849427698681));
#14920=CARTESIAN_POINT('Ctrl Pts',(-9.16245597895801,-0.988934269126449,
17.5005457166497));
#14921=CARTESIAN_POINT('Ctrl Pts',(-8.83525724035327,-1.20808279681468,
17.5164530578013));
#14922=CARTESIAN_POINT('Ctrl Pts',(-8.38876013652682,-1.24773270561251,
17.5323603989529));
#14923=CARTESIAN_POINT('Ctrl Pts',(-8.02665222357482,-1.09152891264187,
17.5482677401045));
#14924=CARTESIAN_POINT('Ctrl Pts',(-7.84559826709884,-1.01342701615656,
17.5562214106804));
#14925=CARTESIAN_POINT('Ctrl Pts',(-7.68564160834148,-0.886361694229139,
17.5641750812562));
#14926=CARTESIAN_POINT('Ctrl Pts',(-7.56359443378863,-0.729753018927428,
17.572128751832));
#14927=CARTESIAN_POINT('Ctrl Pts',(-7.44154725923576,-0.573144343625699,
17.5800824224078));
#14928=CARTESIAN_POINT('Ctrl Pts',(-7.35740956888742,-0.386992314949683,
17.5880360929836));
#14929=CARTESIAN_POINT('Ctrl Pts',(-7.32590577206228,-0.192344036827784,
17.5959897635594));
#14930=CARTESIAN_POINT('Ctrl Pts',(-7.26289817841198,0.196952519416013,
17.611897104711));
#14931=CARTESIAN_POINT('Ctrl Pts',(-7.41042615885448,0.62023407344335,17.6278044458627));
#14932=CARTESIAN_POINT('Ctrl Pts',(-7.70286921780885,0.883980445933719,
17.6437117870143));
#14933=CARTESIAN_POINT('Ctrl Pts',(-7.99531227676318,1.14772681842406,17.6596191281659));
#14934=CARTESIAN_POINT('Ctrl Pts',(-8.43267041422935,1.25193800937752,17.6755264693175));
#14935=CARTESIAN_POINT('Ctrl Pts',(-8.81296522226336,1.14840913211923,17.6914338104691));
#14936=CARTESIAN_POINT('Ctrl Pts',(-9.19326003029737,1.04488025486095,17.7073411516207));
#14937=CARTESIAN_POINT('Ctrl Pts',(-9.5164915088992,0.733611309390916,17.7232484927724));
#14938=CARTESIAN_POINT('Ctrl Pts',(-9.63496652153152,0.357793699254791,
17.739155833924));
#14939=CARTESIAN_POINT('Ctrl Pts',(-9.67116551426496,0.242965950886986,
17.7440161813843));
#14940=CARTESIAN_POINT('Ctrl Pts',(-9.6882493851827,0.122112236099562,17.7488765288446));
#14941=CARTESIAN_POINT('Ctrl Pts',(-9.68732689617031,0.000994531771981839,
17.7537368763049));
#14942=CARTESIAN_POINT('Origin',(-8.5,0.,1.8));
#14943=CARTESIAN_POINT('',(-9.688225,7.10764780365025E-13,18.0962631236951));
#14944=CARTESIAN_POINT('',(-9.688225,-1.00647268297394E-12,18.0537368763049));
#14945=CARTESIAN_POINT('',(-9.688225,-1.45515594291686E-16,1.8));
#14946=CARTESIAN_POINT('Ctrl Pts',(-9.688225,7.78266340262235E-13,18.0962631236951));
#14947=CARTESIAN_POINT('Ctrl Pts',(-9.68822499999981,0.298712821306883,
18.0842599369058));
#14948=CARTESIAN_POINT('Ctrl Pts',(-9.57054245632546,0.595858078272252,
18.0722567501165));
#14949=CARTESIAN_POINT('Ctrl Pts',(-9.36601586214879,0.813569405233311,
18.0602535633272));
#14950=CARTESIAN_POINT('Ctrl Pts',(-9.16148926797212,1.03128073219437,18.0482503765379));
#14951=CARTESIAN_POINT('Ctrl Pts',(-8.87226522412764,1.16727314847162,18.0362471897486));
#14952=CARTESIAN_POINT('Ctrl Pts',(-8.57413435701366,1.18591009260195,18.0242440029592));
#14953=CARTESIAN_POINT('Ctrl Pts',(-8.27600348989968,1.20454703673229,18.0122408161699));
#14954=CARTESIAN_POINT('Ctrl Pts',(-7.97209482032015,1.10563290540072,18.0002376293806));
#14955=CARTESIAN_POINT('Ctrl Pts',(-7.74204705371995,0.915087963996029,
17.9882344425913));
#14956=CARTESIAN_POINT('Ctrl Pts',(-7.51199928711976,0.72454302259134,17.976231255802));
#14957=CARTESIAN_POINT('Ctrl Pts',(-7.35822688079601,0.44436712806063,17.9642280690126));
#14958=CARTESIAN_POINT('Ctrl Pts',(-7.32102560975806,0.14797985598942,17.9522248822233));
#14959=CARTESIAN_POINT('Ctrl Pts',(-7.28382433872011,-0.148407416081791,
17.940221695434));
#14960=CARTESIAN_POINT('Ctrl Pts',(-7.36358464744671,-0.457895344722822,
17.9282185086447));
#14961=CARTESIAN_POINT('Ctrl Pts',(-7.53940549437936,-0.699383189958434,
17.9162153218554));
#14962=CARTESIAN_POINT('Ctrl Pts',(-7.71522634131201,-0.940871035194046,
17.9042121350661));
#14963=CARTESIAN_POINT('Ctrl Pts',(-7.98526240565871,-1.11182427083123,
17.8922089482767));
#14964=CARTESIAN_POINT('Ctrl Pts',(-8.27875123560209,-1.16744491727764,
17.8802057614874));
#14965=CARTESIAN_POINT('Ctrl Pts',(-8.57224006554548,-1.22306556372405,
17.8682025746981));
#14966=CARTESIAN_POINT('Ctrl Pts',(-8.88610136060035,-1.16276985666993,
17.8561993879088));
#14967=CARTESIAN_POINT('Ctrl Pts',(-9.13808834820176,-1.00235817476297,
17.8441962011195));
#14968=CARTESIAN_POINT('Ctrl Pts',(-9.39007533580317,-0.841946492856008,
17.8321930143301));
#14969=CARTESIAN_POINT('Ctrl Pts',(-9.57754329642185,-0.583102430602014,
17.8201898275408));
#14970=CARTESIAN_POINT('Ctrl Pts',(-9.65136659729216,-0.293655596345245,
17.8081866407515));
#14971=CARTESIAN_POINT('Ctrl Pts',(-9.67581103310557,-0.197813707971618,
17.8042121350661));
#14972=CARTESIAN_POINT('Ctrl Pts',(-9.68822500000006,-0.0989100500916012,
17.8002376293806));
#14973=CARTESIAN_POINT('Ctrl Pts',(-9.688225,6.85118628496184E-13,17.7962631236952));
#14974=CARTESIAN_POINT('Ctrl Pts',(-9.688225,-9.64561763794336E-13,17.7537368763049));
#14975=CARTESIAN_POINT('Ctrl Pts',(-9.68822499999976,-0.298712821307047,
17.7657400630942));
#14976=CARTESIAN_POINT('Ctrl Pts',(-9.57054245632539,-0.595858078272375,
17.7777432498835));
#14977=CARTESIAN_POINT('Ctrl Pts',(-9.36601586214871,-0.813569405233398,
17.7897464366728));
#14978=CARTESIAN_POINT('Ctrl Pts',(-9.16148926797204,-1.03128073219442,
17.8017496234622));
#14979=CARTESIAN_POINT('Ctrl Pts',(-8.87226522412757,-1.16727314847164,
17.8137528102515));
#14980=CARTESIAN_POINT('Ctrl Pts',(-8.57413435701361,-1.18591009260196,
17.8257559970408));
#14981=CARTESIAN_POINT('Ctrl Pts',(-8.27600348989965,-1.20454703673227,
17.8377591838301));
#14982=CARTESIAN_POINT('Ctrl Pts',(-7.97209482032014,-1.10563290540071,
17.8497623706194));
#14983=CARTESIAN_POINT('Ctrl Pts',(-7.74204705371997,-0.915087963996039,
17.8617655574087));
#14984=CARTESIAN_POINT('Ctrl Pts',(-7.51199928711979,-0.724543022591367,
17.8737687441981));
#14985=CARTESIAN_POINT('Ctrl Pts',(-7.35822688079604,-0.444367128060688,
17.8857719309874));
#14986=CARTESIAN_POINT('Ctrl Pts',(-7.32102560975807,-0.147979855989503,
17.8977751177767));
#14987=CARTESIAN_POINT('Ctrl Pts',(-7.2838243387201,0.148407416081682,17.909778304566));
#14988=CARTESIAN_POINT('Ctrl Pts',(-7.36358464744666,0.457895344722696,
17.9217814913553));
#14989=CARTESIAN_POINT('Ctrl Pts',(-7.53940549437927,0.699383189958312,
17.9337846781446));
#14990=CARTESIAN_POINT('Ctrl Pts',(-7.71522634131187,0.940871035193927,
17.945787864934));
#14991=CARTESIAN_POINT('Ctrl Pts',(-7.98526240565853,1.11182427083114,17.9577910517233));
#14992=CARTESIAN_POINT('Ctrl Pts',(-8.27875123560188,1.1674449172776,17.9697942385126));
#14993=CARTESIAN_POINT('Ctrl Pts',(-8.57224006554523,1.22306556372406,17.9817974253019));
#14994=CARTESIAN_POINT('Ctrl Pts',(-8.88610136060009,1.16276985667001,17.9938006120912));
#14995=CARTESIAN_POINT('Ctrl Pts',(-9.13808834820152,1.00235817476312,18.0058037988805));
#14996=CARTESIAN_POINT('Ctrl Pts',(-9.39007533580295,0.841946492856234,
18.0178069856699));
#14997=CARTESIAN_POINT('Ctrl Pts',(-9.57754329642169,0.583102430602313,
18.0298101724592));
#14998=CARTESIAN_POINT('Ctrl Pts',(-9.65136659729207,0.293655596345588,
18.0418133592485));
#14999=CARTESIAN_POINT('Ctrl Pts',(-9.67581103310556,0.197813707971772,
18.045787864934));
#15000=CARTESIAN_POINT('Ctrl Pts',(-9.68822500000008,0.0989100500915499,
18.0497623706194));
#15001=CARTESIAN_POINT('Ctrl Pts',(-9.688225,-9.39026634227957E-13,18.0537368763049));
#15002=CARTESIAN_POINT('Origin',(-8.5,0.,1.8));
#15003=CARTESIAN_POINT('',(-9.688225,7.36299909931404E-13,18.3962631236951));
#15004=CARTESIAN_POINT('',(-9.688225,-9.80826531105095E-13,18.3537368763049));
#15005=CARTESIAN_POINT('',(-9.688225,-1.45515594291686E-16,1.8));
#15006=CARTESIAN_POINT('Ctrl Pts',(-9.688225,7.36299909931404E-13,18.3962631236951));
#15007=CARTESIAN_POINT('Ctrl Pts',(-9.68822499999982,0.298712821306841,
18.3842599369058));
#15008=CARTESIAN_POINT('Ctrl Pts',(-9.57054245632548,0.595858078272214,
18.3722567501165));
#15009=CARTESIAN_POINT('Ctrl Pts',(-9.36601586214882,0.813569405233281,
18.3602535633272));
#15010=CARTESIAN_POINT('Ctrl Pts',(-9.16148926797216,1.03128073219435,18.3482503765379));
#15011=CARTESIAN_POINT('Ctrl Pts',(-8.87226522412768,1.16727314847161,18.3362471897486));
#15012=CARTESIAN_POINT('Ctrl Pts',(-8.5741343570137,1.18591009260195,18.3242440029592));
#15013=CARTESIAN_POINT('Ctrl Pts',(-8.27600348989972,1.20454703673229,18.3122408161699));
#15014=CARTESIAN_POINT('Ctrl Pts',(-7.97209482032018,1.10563290540074,18.3002376293806));
#15015=CARTESIAN_POINT('Ctrl Pts',(-7.74204705371999,0.915087963996056,
18.2882344425913));
#15016=CARTESIAN_POINT('Ctrl Pts',(-7.51199928711979,0.724543022591374,
18.276231255802));
#15017=CARTESIAN_POINT('Ctrl Pts',(-7.35822688079603,0.444367128060671,
18.2642280690126));
#15018=CARTESIAN_POINT('Ctrl Pts',(-7.32102560975807,0.147979855989462,
18.2522248822233));
#15019=CARTESIAN_POINT('Ctrl Pts',(-7.2838243387201,-0.148407416081748,
18.240221695434));
#15020=CARTESIAN_POINT('Ctrl Pts',(-7.36358464744669,-0.457895344722782,
18.2282185086447));
#15021=CARTESIAN_POINT('Ctrl Pts',(-7.53940549437933,-0.6993831899584,18.2162153218554));
#15022=CARTESIAN_POINT('Ctrl Pts',(-7.71522634131197,-0.940871035194018,
18.2042121350661));
#15023=CARTESIAN_POINT('Ctrl Pts',(-7.98526240565867,-1.11182427083121,
18.1922089482767));
#15024=CARTESIAN_POINT('Ctrl Pts',(-8.27875123560205,-1.16744491727763,
18.1802057614874));
#15025=CARTESIAN_POINT('Ctrl Pts',(-8.57224006554543,-1.22306556372406,
18.1682025746981));
#15026=CARTESIAN_POINT('Ctrl Pts',(-8.88610136060031,-1.16276985666994,
18.1561993879088));
#15027=CARTESIAN_POINT('Ctrl Pts',(-9.13808834820172,-1.00235817476299,
18.1441962011195));
#15028=CARTESIAN_POINT('Ctrl Pts',(-9.39007533580314,-0.841946492856039,
18.1321930143301));
#15029=CARTESIAN_POINT('Ctrl Pts',(-9.57754329642183,-0.583102430602052,
18.1201898275408));
#15030=CARTESIAN_POINT('Ctrl Pts',(-9.65136659729215,-0.293655596345285,
18.1081866407515));
#15031=CARTESIAN_POINT('Ctrl Pts',(-9.67581103310557,-0.197813707971616,
18.1042121350661));
#15032=CARTESIAN_POINT('Ctrl Pts',(-9.68822500000006,-0.0989100500915531,
18.1002376293806));
#15033=CARTESIAN_POINT('Ctrl Pts',(-9.688225,7.78266340262235E-13,18.0962631236951));
#15034=CARTESIAN_POINT('Ctrl Pts',(-9.688225,-9.39026634227957E-13,18.0537368763049));
#15035=CARTESIAN_POINT('Ctrl Pts',(-9.68822499999976,-0.298712821307044,
18.0657400630942));
#15036=CARTESIAN_POINT('Ctrl Pts',(-9.57054245632538,-0.595858078272397,
18.0777432498835));
#15037=CARTESIAN_POINT('Ctrl Pts',(-9.36601586214868,-0.813569405233428,
18.0897464366728));
#15038=CARTESIAN_POINT('Ctrl Pts',(-9.16148926797198,-1.03128073219446,
18.1017496234622));
#15039=CARTESIAN_POINT('Ctrl Pts',(-8.87226522412749,-1.16727314847167,
18.1137528102515));
#15040=CARTESIAN_POINT('Ctrl Pts',(-8.5741343570135,-1.18591009260196,18.1257559970408));
#15041=CARTESIAN_POINT('Ctrl Pts',(-8.27600348989951,-1.20454703673225,
18.1377591838301));
#15042=CARTESIAN_POINT('Ctrl Pts',(-7.97209482032,-1.10563290540065,18.1497623706194));
#15043=CARTESIAN_POINT('Ctrl Pts',(-7.74204705371983,-0.915087963995926,
18.1617655574087));
#15044=CARTESIAN_POINT('Ctrl Pts',(-7.51199928711966,-0.724543022591206,
18.1737687441981));
#15045=CARTESIAN_POINT('Ctrl Pts',(-7.35822688079595,-0.444367128060476,
18.1857719309874));
#15046=CARTESIAN_POINT('Ctrl Pts',(-7.32102560975804,-0.147979855989261,
18.1977751177767));
#15047=CARTESIAN_POINT('Ctrl Pts',(-7.28382433872013,0.148407416081955,
18.209778304566));
#15048=CARTESIAN_POINT('Ctrl Pts',(-7.36358464744677,0.457895344722976,
18.2217814913553));
#15049=CARTESIAN_POINT('Ctrl Pts',(-7.53940549437945,0.699383189958564,
18.2337846781447));
#15050=CARTESIAN_POINT('Ctrl Pts',(-7.71522634131214,0.940871035194152,
18.245787864934));
#15051=CARTESIAN_POINT('Ctrl Pts',(-7.98526240565886,1.1118242708313,18.2577910517233));
#15052=CARTESIAN_POINT('Ctrl Pts',(-8.27875123560225,1.16744491727767,18.2697942385126));
#15053=CARTESIAN_POINT('Ctrl Pts',(-8.57224006554564,1.22306556372404,18.2817974253019));
#15054=CARTESIAN_POINT('Ctrl Pts',(-8.88610136060051,1.16276985666988,18.2938006120912));
#15055=CARTESIAN_POINT('Ctrl Pts',(-9.13808834820189,1.00235817476288,18.3058037988806));
#15056=CARTESIAN_POINT('Ctrl Pts',(-9.39007533580328,0.841946492855888,
18.3178069856699));
#15057=CARTESIAN_POINT('Ctrl Pts',(-9.57754329642193,0.583102430601868,
18.3298101724592));
#15058=CARTESIAN_POINT('Ctrl Pts',(-9.6513665972922,0.293655596345089,18.3418133592485));
#15059=CARTESIAN_POINT('Ctrl Pts',(-9.6758110331056,0.197813707971437,18.345787864934));
#15060=CARTESIAN_POINT('Ctrl Pts',(-9.68822500000008,0.0989100500913954,
18.3497623706194));
#15061=CARTESIAN_POINT('Ctrl Pts',(-9.688225,-9.13324971207885E-13,18.3537368763049));
#15062=CARTESIAN_POINT('Origin',(-8.5,0.,1.8));
#15063=CARTESIAN_POINT('',(-9.688225,7.61946061800245E-13,18.6962631236951));
#15064=CARTESIAN_POINT('',(-9.688225,-9.55291401538716E-13,18.6537368763049));
#15065=CARTESIAN_POINT('',(-9.688225,-1.45515594291686E-16,1.8));
#15066=CARTESIAN_POINT('Ctrl Pts',(-9.688225,8.29447621697454E-13,18.6962631236951));
#15067=CARTESIAN_POINT('Ctrl Pts',(-9.68822499999979,0.298712821306934,
18.6842599369058));
#15068=CARTESIAN_POINT('Ctrl Pts',(-9.57054245632543,0.595858078272298,
18.6722567501165));
#15069=CARTESIAN_POINT('Ctrl Pts',(-9.36601586214876,0.813569405233349,
18.6602535633272));
#15070=CARTESIAN_POINT('Ctrl Pts',(-9.16148926797208,1.0312807321944,18.6482503765379));
#15071=CARTESIAN_POINT('Ctrl Pts',(-8.87226522412759,1.16727314847164,18.6362471897486));
#15072=CARTESIAN_POINT('Ctrl Pts',(-8.57413435701361,1.18591009260196,18.6242440029592));
#15073=CARTESIAN_POINT('Ctrl Pts',(-8.27600348989962,1.20454703673228,18.6122408161699));
#15074=CARTESIAN_POINT('Ctrl Pts',(-7.9720948203201,1.1056329054007,18.6002376293806));
#15075=CARTESIAN_POINT('Ctrl Pts',(-7.74204705371991,0.915087963995996,
18.5882344425913));
#15076=CARTESIAN_POINT('Ctrl Pts',(-7.51199928711973,0.724543022591297,
18.576231255802));
#15077=CARTESIAN_POINT('Ctrl Pts',(-7.35822688079599,0.444367128060581,
18.5642280690126));
#15078=CARTESIAN_POINT('Ctrl Pts',(-7.32102560975805,0.147979855989369,
18.5522248822233));
#15079=CARTESIAN_POINT('Ctrl Pts',(-7.28382433872012,-0.148407416081843,
18.540221695434));
#15080=CARTESIAN_POINT('Ctrl Pts',(-7.36358464744673,-0.457895344722872,
18.5282185086447));
#15081=CARTESIAN_POINT('Ctrl Pts',(-7.53940549437939,-0.699383189958476,
18.5162153218554));
#15082=CARTESIAN_POINT('Ctrl Pts',(-7.71522634131205,-0.94087103519408,
18.5042121350661));
#15083=CARTESIAN_POINT('Ctrl Pts',(-7.98526240565876,-1.11182427083125,
18.4922089482767));
#15084=CARTESIAN_POINT('Ctrl Pts',(-8.27875123560214,-1.16744491727765,
18.4802057614874));
#15085=CARTESIAN_POINT('Ctrl Pts',(-8.57224006554553,-1.22306556372405,
18.4682025746981));
#15086=CARTESIAN_POINT('Ctrl Pts',(-8.8861013606004,-1.16276985666991,18.4561993879088));
#15087=CARTESIAN_POINT('Ctrl Pts',(-9.1380883482018,-1.00235817476294,18.4441962011195));
#15088=CARTESIAN_POINT('Ctrl Pts',(-9.3900753358032,-0.84194649285597,18.4321930143301));
#15089=CARTESIAN_POINT('Ctrl Pts',(-9.57754329642188,-0.583102430601968,
18.4201898275408));
#15090=CARTESIAN_POINT('Ctrl Pts',(-9.65136659729217,-0.293655596345195,
18.4081866407515));
#15091=CARTESIAN_POINT('Ctrl Pts',(-9.67581103310557,-0.197813707971568,
18.4042121350661));
#15092=CARTESIAN_POINT('Ctrl Pts',(-9.68822500000006,-0.09891005009155,
18.4002376293806));
#15093=CARTESIAN_POINT('Ctrl Pts',(-9.688225,7.36299909931404E-13,18.3962631236951));
#15094=CARTESIAN_POINT('Ctrl Pts',(-9.688225,-9.13324971207885E-13,18.3537368763049));
#15095=CARTESIAN_POINT('Ctrl Pts',(-9.68822499999977,-0.298712821306996,
18.3657400630942));
#15096=CARTESIAN_POINT('Ctrl Pts',(-9.57054245632541,-0.595858078272329,
18.3777432498835));
#15097=CARTESIAN_POINT('Ctrl Pts',(-9.36601586214875,-0.81356940523336,
18.3897464366728));
#15098=CARTESIAN_POINT('Ctrl Pts',(-9.16148926797208,-1.03128073219439,
18.4017496234621));
#15099=CARTESIAN_POINT('Ctrl Pts',(-8.87226522412762,-1.16727314847162,
18.4137528102515));
#15100=CARTESIAN_POINT('Ctrl Pts',(-8.57413435701366,-1.18591009260195,
18.4257559970408));
#15101=CARTESIAN_POINT('Ctrl Pts',(-8.2760034898997,-1.20454703673228,18.4377591838301));
#15102=CARTESIAN_POINT('Ctrl Pts',(-7.97209482032019,-1.10563290540073,
18.4497623706194));
#15103=CARTESIAN_POINT('Ctrl Pts',(-7.74204705372001,-0.915087963996072,
18.4617655574087));
#15104=CARTESIAN_POINT('Ctrl Pts',(-7.51199928711982,-0.72454302259141,
18.4737687441981));
#15105=CARTESIAN_POINT('Ctrl Pts',(-7.35822688079606,-0.444367128060738,
18.4857719309874));
#15106=CARTESIAN_POINT('Ctrl Pts',(-7.32102560975808,-0.147979855989554,
18.4977751177767));
#15107=CARTESIAN_POINT('Ctrl Pts',(-7.2838243387201,0.14840741608163,18.509778304566));
#15108=CARTESIAN_POINT('Ctrl Pts',(-7.36358464744664,0.457895344722647,
18.5217814913553));
#15109=CARTESIAN_POINT('Ctrl Pts',(-7.53940549437924,0.69938318995827,18.5337846781446));
#15110=CARTESIAN_POINT('Ctrl Pts',(-7.71522634131183,0.940871035193894,
18.545787864934));
#15111=CARTESIAN_POINT('Ctrl Pts',(-7.98526240565848,1.11182427083112,18.5577910517233));
#15112=CARTESIAN_POINT('Ctrl Pts',(-8.27875123560183,1.16744491727759,18.5697942385126));
#15113=CARTESIAN_POINT('Ctrl Pts',(-8.57224006554518,1.22306556372407,18.5817974253019));
#15114=CARTESIAN_POINT('Ctrl Pts',(-8.88610136060004,1.16276985667003,18.5938006120912));
#15115=CARTESIAN_POINT('Ctrl Pts',(-9.13808834820147,1.00235817476315,18.6058037988805));
#15116=CARTESIAN_POINT('Ctrl Pts',(-9.39007533580291,0.841946492856273,
18.6178069856699));
#15117=CARTESIAN_POINT('Ctrl Pts',(-9.57754329642166,0.58310243060236,18.6298101724592));
#15118=CARTESIAN_POINT('Ctrl Pts',(-9.65136659729206,0.293655596345638,
18.6418133592485));
#15119=CARTESIAN_POINT('Ctrl Pts',(-9.67581103310556,0.197813707971779,
18.645787864934));
#15120=CARTESIAN_POINT('Ctrl Pts',(-9.68822500000008,0.0989100500915112,
18.6497623706194));
#15121=CARTESIAN_POINT('Ctrl Pts',(-9.688225,-1.02273745028469E-12,18.6537368763049));
#15122=CARTESIAN_POINT('Origin',(-8.5,0.,1.8));
#15123=CARTESIAN_POINT('',(-9.688225,7.87592213669086E-13,18.9962631236951));
#15124=CARTESIAN_POINT('',(-9.688225,-9.29589738518644E-13,18.9537368763049));
#15125=CARTESIAN_POINT('',(-9.688225,-1.45515594291686E-16,1.8));
#15126=CARTESIAN_POINT('Ctrl Pts',(-9.688225,7.87592213669086E-13,18.9962631236951));
#15127=CARTESIAN_POINT('Ctrl Pts',(-9.6882249999998,0.29871282130687,18.9842599369058));
#15128=CARTESIAN_POINT('Ctrl Pts',(-9.57054245632547,0.595858078272216,
18.9722567501165));
#15129=CARTESIAN_POINT('Ctrl Pts',(-9.36601586214883,0.813569405233269,
18.9602535633272));
#15130=CARTESIAN_POINT('Ctrl Pts',(-9.16148926797219,1.03128073219432,18.9482503765379));
#15131=CARTESIAN_POINT('Ctrl Pts',(-8.87226522412774,1.16727314847158,18.9362471897486));
#15132=CARTESIAN_POINT('Ctrl Pts',(-8.57413435701378,1.18591009260194,18.9242440029592));
#15133=CARTESIAN_POINT('Ctrl Pts',(-8.27600348989982,1.20454703673231,18.9122408161699));
#15134=CARTESIAN_POINT('Ctrl Pts',(-7.97209482032031,1.10563290540079,18.9002376293806));
#15135=CARTESIAN_POINT('Ctrl Pts',(-7.7420470537201,0.915087963996152,18.8882344425913));
#15136=CARTESIAN_POINT('Ctrl Pts',(-7.5119992871199,0.724543022591515,18.876231255802));
#15137=CARTESIAN_POINT('Ctrl Pts',(-7.35822688079611,0.444367128060859,
18.8642280690127));
#15138=CARTESIAN_POINT('Ctrl Pts',(-7.32102560975809,0.147979855989679,
18.8522248822233));
#15139=CARTESIAN_POINT('Ctrl Pts',(-7.28382433872008,-0.148407416081501,
18.840221695434));
#15140=CARTESIAN_POINT('Ctrl Pts',(-7.3635846474466,-0.457895344722527,
18.8282185086447));
#15141=CARTESIAN_POINT('Ctrl Pts',(-7.53940549437916,-0.699383189958169,
18.8162153218554));
#15142=CARTESIAN_POINT('Ctrl Pts',(-7.71522634131173,-0.940871035193811,
18.8042121350661));
#15143=CARTESIAN_POINT('Ctrl Pts',(-7.98526240565836,-1.11182427083106,
18.7922089482768));
#15144=CARTESIAN_POINT('Ctrl Pts',(-8.27875123560171,-1.16744491727757,
18.7802057614874));
#15145=CARTESIAN_POINT('Ctrl Pts',(-8.57224006554505,-1.22306556372407,
18.7682025746981));
#15146=CARTESIAN_POINT('Ctrl Pts',(-8.88610136059992,-1.16276985667007,
18.7561993879088));
#15147=CARTESIAN_POINT('Ctrl Pts',(-9.13808834820137,-1.00235817476322,
18.7441962011195));
#15148=CARTESIAN_POINT('Ctrl Pts',(-9.39007533580282,-0.841946492856367,
18.7321930143302));
#15149=CARTESIAN_POINT('Ctrl Pts',(-9.5775432964216,-0.583102430602474,
18.7201898275408));
#15150=CARTESIAN_POINT('Ctrl Pts',(-9.65136659729203,-0.293655596345759,
18.7081866407515));
#15151=CARTESIAN_POINT('Ctrl Pts',(-9.67581103310553,-0.197813707971926,
18.7042121350661));
#15152=CARTESIAN_POINT('Ctrl Pts',(-9.68822500000007,-0.0989100500916821,
18.7002376293806));
#15153=CARTESIAN_POINT('Ctrl Pts',(-9.688225,8.29447621697454E-13,18.6962631236951));
#15154=CARTESIAN_POINT('Ctrl Pts',(-9.688225,-1.02273745028469E-12,18.6537368763049));
#15155=CARTESIAN_POINT('Ctrl Pts',(-9.68822499999974,-0.298712821307128,
18.6657400630942));
#15156=CARTESIAN_POINT('Ctrl Pts',(-9.57054245632534,-0.595858078272472,
18.6777432498835));
#15157=CARTESIAN_POINT('Ctrl Pts',(-9.36601586214863,-0.813569405233489,
18.6897464366728));
#15158=CARTESIAN_POINT('Ctrl Pts',(-9.16148926797191,-1.03128073219451,
18.7017496234622));
#15159=CARTESIAN_POINT('Ctrl Pts',(-8.8722652241274,-1.1672731484717,18.7137528102515));
#15160=CARTESIAN_POINT('Ctrl Pts',(-8.57413435701342,-1.18591009260197,
18.7257559970408));
#15161=CARTESIAN_POINT('Ctrl Pts',(-8.27600348989943,-1.20454703673224,
18.7377591838301));
#15162=CARTESIAN_POINT('Ctrl Pts',(-7.97209482031992,-1.10563290540061,
18.7497623706194));
#15163=CARTESIAN_POINT('Ctrl Pts',(-7.74204705371976,-0.915087963995873,
18.7617655574087));
#15164=CARTESIAN_POINT('Ctrl Pts',(-7.51199928711961,-0.724543022591136,
18.7737687441981));
#15165=CARTESIAN_POINT('Ctrl Pts',(-7.35822688079592,-0.444367128060395,
18.7857719309874));
#15166=CARTESIAN_POINT('Ctrl Pts',(-7.32102560975803,-0.147979855989177,
18.7977751177767));
#15167=CARTESIAN_POINT('Ctrl Pts',(-7.28382433872014,0.148407416082041,
18.809778304566));
#15168=CARTESIAN_POINT('Ctrl Pts',(-7.3635846474468,0.457895344723056,18.8217814913553));
#15169=CARTESIAN_POINT('Ctrl Pts',(-7.5394054943795,0.699383189958632,18.8337846781447));
#15170=CARTESIAN_POINT('Ctrl Pts',(-7.7152263413122,0.940871035194207,18.845787864934));
#15171=CARTESIAN_POINT('Ctrl Pts',(-7.98526240565894,1.11182427083134,18.8577910517233));
#15172=CARTESIAN_POINT('Ctrl Pts',(-8.27875123560233,1.16744491727769,18.8697942385126));
#15173=CARTESIAN_POINT('Ctrl Pts',(-8.57224006554573,1.22306556372404,18.8817974253019));
#15174=CARTESIAN_POINT('Ctrl Pts',(-8.88610136060059,1.16276985666985,18.8938006120912));
#15175=CARTESIAN_POINT('Ctrl Pts',(-9.13808834820196,1.00235817476284,18.9058037988806));
#15176=CARTESIAN_POINT('Ctrl Pts',(-9.39007533580334,0.841946492855824,
18.9178069856699));
#15177=CARTESIAN_POINT('Ctrl Pts',(-9.57754329642197,0.583102430601792,
18.9298101724592));
#15178=CARTESIAN_POINT('Ctrl Pts',(-9.65136659729222,0.293655596345008,
18.9418133592485));
#15179=CARTESIAN_POINT('Ctrl Pts',(-9.6758110331056,0.197813707971398,18.945787864934));
#15180=CARTESIAN_POINT('Ctrl Pts',(-9.68822500000007,0.0989100500914017,
18.9497623706194));
#15181=CARTESIAN_POINT('Ctrl Pts',(-9.688225,-8.62088178621434E-13,18.9537368763049));
#15182=CARTESIAN_POINT('Origin',(-8.5,0.,1.8));
#15183=CARTESIAN_POINT('',(-9.68783295262227,-0.000517608156923501,19.2962631236951));
#15184=CARTESIAN_POINT('',(-9.688225,-9.03999097801034E-13,19.2537368763049));
#15185=CARTESIAN_POINT('',(-9.688225,-1.45515594291686E-16,1.8));
#15186=CARTESIAN_POINT('Ctrl Pts',(-9.688225,8.80739925435137E-13,19.2962631236951));
#15187=CARTESIAN_POINT('Ctrl Pts',(-9.68822499999978,0.298712821306963,
19.2842599369058));
#15188=CARTESIAN_POINT('Ctrl Pts',(-9.57054245632543,0.5958580782723,19.2722567501165));
#15189=CARTESIAN_POINT('Ctrl Pts',(-9.36601586214877,0.813569405233337,
19.2602535633272));
#15190=CARTESIAN_POINT('Ctrl Pts',(-9.16148926797211,1.03128073219437,19.2482503765379));
#15191=CARTESIAN_POINT('Ctrl Pts',(-8.87226522412765,1.16727314847161,19.2362471897486));
#15192=CARTESIAN_POINT('Ctrl Pts',(-8.57413435701369,1.18591009260195,19.2242440029592));
#15193=CARTESIAN_POINT('Ctrl Pts',(-8.27600348989973,1.20454703673229,19.2122408161699));
#15194=CARTESIAN_POINT('Ctrl Pts',(-7.97209482032022,1.10563290540075,19.2002376293806));
#15195=CARTESIAN_POINT('Ctrl Pts',(-7.74204705372003,0.915087963996093,
19.1882344425913));
#15196=CARTESIAN_POINT('Ctrl Pts',(-7.51199928711984,0.724543022591437,
19.176231255802));
#15197=CARTESIAN_POINT('Ctrl Pts',(-7.35822688079607,0.444367128060769,
19.1642280690127));
#15198=CARTESIAN_POINT('Ctrl Pts',(-7.32102560975808,0.147979855989586,
19.1522248822233));
#15199=CARTESIAN_POINT('Ctrl Pts',(-7.28382433872009,-0.148407416081596,
19.140221695434));
#15200=CARTESIAN_POINT('Ctrl Pts',(-7.36358464744663,-0.457895344722616,
19.1282185086447));
#15201=CARTESIAN_POINT('Ctrl Pts',(-7.53940549437922,-0.699383189958244,
19.1162153218554));
#15202=CARTESIAN_POINT('Ctrl Pts',(-7.71522634131181,-0.940871035193872,
19.1042121350661));
#15203=CARTESIAN_POINT('Ctrl Pts',(-7.98526240565845,-1.1118242708311,19.0922089482767));
#15204=CARTESIAN_POINT('Ctrl Pts',(-8.2787512356018,-1.16744491727759,19.0802057614874));
#15205=CARTESIAN_POINT('Ctrl Pts',(-8.57224006554514,-1.22306556372407,
19.0682025746981));
#15206=CARTESIAN_POINT('Ctrl Pts',(-8.88610136060001,-1.16276985667004,
19.0561993879088));
#15207=CARTESIAN_POINT('Ctrl Pts',(-9.13808834820145,-1.00235817476317,
19.0441962011195));
#15208=CARTESIAN_POINT('Ctrl Pts',(-9.39007533580289,-0.841946492856298,
19.0321930143302));
#15209=CARTESIAN_POINT('Ctrl Pts',(-9.57754329642164,-0.583102430602389,
19.0201898275408));
#15210=CARTESIAN_POINT('Ctrl Pts',(-9.65136659729205,-0.293655596345669,
19.0081866407515));
#15211=CARTESIAN_POINT('Ctrl Pts',(-9.67581103310554,-0.197813707971877,
19.0042121350661));
#15212=CARTESIAN_POINT('Ctrl Pts',(-9.68822500000007,-0.0989100500916788,
19.0002376293806));
#15213=CARTESIAN_POINT('Ctrl Pts',(-9.688225,7.87592213669086E-13,18.9962631236951));
#15214=CARTESIAN_POINT('Ctrl Pts',(-9.688225,-8.62088178621434E-13,18.9537368763049));
#15215=CARTESIAN_POINT('Ctrl Pts',(-9.68822499999978,-0.298712821306989,
18.9657400630942));
#15216=CARTESIAN_POINT('Ctrl Pts',(-9.5705424563254,-0.595858078272372,
18.9777432498835));
#15217=CARTESIAN_POINT('Ctrl Pts',(-9.36601586214869,-0.813569405233421,
18.9897464366728));
#15218=CARTESIAN_POINT('Ctrl Pts',(-9.16148926797198,-1.03128073219447,
19.0017496234621));
#15219=CARTESIAN_POINT('Ctrl Pts',(-8.87226522412745,-1.16727314847169,
19.0137528102515));
#15220=CARTESIAN_POINT('Ctrl Pts',(-8.57413435701344,-1.18591009260197,
19.0257559970408));
#15221=CARTESIAN_POINT('Ctrl Pts',(-8.27600348989943,-1.20454703673225,
19.0377591838301));
#15222=CARTESIAN_POINT('Ctrl Pts',(-7.9720948203199,-1.10563290540061,19.0497623706194));
#15223=CARTESIAN_POINT('Ctrl Pts',(-7.74204705371973,-0.915087963995846,
19.0617655574087));
#15224=CARTESIAN_POINT('Ctrl Pts',(-7.51199928711957,-0.724543022591087,
19.0737687441981));
#15225=CARTESIAN_POINT('Ctrl Pts',(-7.35822688079588,-0.444367128060312,
19.0857719309874));
#15226=CARTESIAN_POINT('Ctrl Pts',(-7.32102560975802,-0.147979855989069,
19.0977751177767));
#15227=CARTESIAN_POINT('Ctrl Pts',(-7.28382433872015,0.148407416082175,
19.109778304566));
#15228=CARTESIAN_POINT('Ctrl Pts',(-7.36358464744686,0.457895344723207,
19.1217814913553));
#15229=CARTESIAN_POINT('Ctrl Pts',(-7.53940549437961,0.699383189958775,
19.1337846781447));
#15230=CARTESIAN_POINT('Ctrl Pts',(-7.71522634131235,0.940871035194342,
19.145787864934));
#15231=CARTESIAN_POINT('Ctrl Pts',(-7.98526240565915,1.11182427083144,19.1577910517233));
#15232=CARTESIAN_POINT('Ctrl Pts',(-8.27875123560257,1.16744491727773,19.1697942385126));
#15233=CARTESIAN_POINT('Ctrl Pts',(-8.572240065546,1.22306556372403,19.1817974253019));
#15234=CARTESIAN_POINT('Ctrl Pts',(-8.88610136060088,1.16276985666976,19.1938006120913));
#15235=CARTESIAN_POINT('Ctrl Pts',(-9.13808834820223,1.00235817476267,19.2058037988806));
#15236=CARTESIAN_POINT('Ctrl Pts',(-9.39007533580358,0.841946492855579,
19.2178069856699));
#15237=CARTESIAN_POINT('Ctrl Pts',(-9.57754329642215,0.58310243060147,19.2298101724592));
#15238=CARTESIAN_POINT('Ctrl Pts',(-9.65136659729231,0.29365559634464,19.2418133592485));
#15239=CARTESIAN_POINT('Ctrl Pts',(-9.67581103310564,0.197813707971131,
19.245787864934));
#15240=CARTESIAN_POINT('Ctrl Pts',(-9.68822500000007,0.0989100500912471,
19.2497623706194));
#15241=CARTESIAN_POINT('Ctrl Pts',(-9.688225,-9.03999097801034E-13,19.2537368763049));
#15242=CARTESIAN_POINT('Origin',(-8.5,0.,1.8));
#15243=CARTESIAN_POINT('',(-9.68921750296084,-0.000102469561994563,19.5962631236951));
#15244=CARTESIAN_POINT('',(-9.688225,-8.78408457083424E-13,19.5537368763049));
#15245=CARTESIAN_POINT('',(-9.688225,-1.45515594291686E-16,1.8));
#15246=CARTESIAN_POINT('Ctrl Pts',(-9.69028507049178,-0.000212689062328297,
19.5962631236951));
#15247=CARTESIAN_POINT('Ctrl Pts',(-9.68998036389171,0.391158548490939,
19.5804677035918));
#15248=CARTESIAN_POINT('Ctrl Pts',(-9.4779526199623,0.783211439565971,19.5646722834885));
#15249=CARTESIAN_POINT('Ctrl Pts',(-9.15044819587364,0.996873139970471,
19.5488768633852));
#15250=CARTESIAN_POINT('Ctrl Pts',(-8.82062318529691,1.21204877551144,19.5329695222336));
#15251=CARTESIAN_POINT('Ctrl Pts',(-8.37367923882642,1.24629622368731,19.5170621810819));
#15252=CARTESIAN_POINT('Ctrl Pts',(-8.01348680256335,1.08572482393094,19.5011548399303));
#15253=CARTESIAN_POINT('Ctrl Pts',(-7.83339058443181,1.00543912405275,19.4932011693545));
#15254=CARTESIAN_POINT('Ctrl Pts',(-7.67498224385212,0.87644871219149,19.4852474987787));
#15255=CARTESIAN_POINT('Ctrl Pts',(-7.55483788786785,0.718375552796157,
19.4772938282029));
#15256=CARTESIAN_POINT('Ctrl Pts',(-7.43469353188358,0.560302393400842,
19.4693401576271));
#15257=CARTESIAN_POINT('Ctrl Pts',(-7.35281316049472,0.373146486471458,
19.4613864870513));
#15258=CARTESIAN_POINT('Ctrl Pts',(-7.32366558028848,0.178131461516125,
19.4534328164754));
#15259=CARTESIAN_POINT('Ctrl Pts',(-7.26537041987601,-0.211898588394563,
19.4375254753238));
#15260=CARTESIAN_POINT('Ctrl Pts',(-7.41800642419409,-0.633365110409051,
19.4216181341722));
#15261=CARTESIAN_POINT('Ctrl Pts',(-7.71361762553116,-0.893555635556405,
19.4057107930206));
#15262=CARTESIAN_POINT('Ctrl Pts',(-8.00922882686823,-1.15374616070376,
19.389803451869));
#15263=CARTESIAN_POINT('Ctrl Pts',(-8.44781522522429,-1.25266068898398,
19.3738961107173));
#15264=CARTESIAN_POINT('Ctrl Pts',(-8.8268302328739,-1.14454041604515,19.3579887695657));
#15265=CARTESIAN_POINT('Ctrl Pts',(-9.20584524052351,-1.03642014310631,
19.3420814284141));
#15266=CARTESIAN_POINT('Ctrl Pts',(-9.52528885746666,-0.721265068948423,
19.3261740872625));
#15267=CARTESIAN_POINT('Ctrl Pts',(-9.6392103838706,-0.344042203087319,
19.3102667461109));
#15268=CARTESIAN_POINT('Ctrl Pts',(-9.6726396881056,-0.233349357359851,
19.3055988719723));
#15269=CARTESIAN_POINT('Ctrl Pts',(-9.6883719131767,-0.117311983360903,
19.3009309978337));
#15270=CARTESIAN_POINT('Ctrl Pts',(-9.68745089909105,-0.00102202174496036,
19.2962631236951));
#15271=CARTESIAN_POINT('Ctrl Pts',(-9.688225,-9.03999097801034E-13,19.2537368763049));
#15272=CARTESIAN_POINT('Ctrl Pts',(-9.68822499999977,-0.298712821307009,
19.2657400630942));
#15273=CARTESIAN_POINT('Ctrl Pts',(-9.5705424563254,-0.595858078272365,
19.2777432498835));
#15274=CARTESIAN_POINT('Ctrl Pts',(-9.36601586214871,-0.813569405233403,
19.2897464366728));
#15275=CARTESIAN_POINT('Ctrl Pts',(-9.16148926797202,-1.03128073219444,
19.3017496234622));
#15276=CARTESIAN_POINT('Ctrl Pts',(-8.87226522412752,-1.16727314847166,
19.3137528102515));
#15277=CARTESIAN_POINT('Ctrl Pts',(-8.57413435701353,-1.18591009260196,
19.3257559970408));
#15278=CARTESIAN_POINT('Ctrl Pts',(-8.27600348989955,-1.20454703673226,
19.3377591838301));
#15279=CARTESIAN_POINT('Ctrl Pts',(-7.97209482032003,-1.10563290540066,
19.3497623706194));
#15280=CARTESIAN_POINT('Ctrl Pts',(-7.74204705371986,-0.915087963995949,
19.3617655574087));
#15281=CARTESIAN_POINT('Ctrl Pts',(-7.51199928711968,-0.724543022591235,
19.3737687441981));
#15282=CARTESIAN_POINT('Ctrl Pts',(-7.35822688079597,-0.444367128060509,
19.3857719309874));
#15283=CARTESIAN_POINT('Ctrl Pts',(-7.32102560975805,-0.147979855989295,
19.3977751177767));
#15284=CARTESIAN_POINT('Ctrl Pts',(-7.28382433872012,0.148407416081919,
19.409778304566));
#15285=CARTESIAN_POINT('Ctrl Pts',(-7.36358464744676,0.457895344722943,
19.4217814913553));
#15286=CARTESIAN_POINT('Ctrl Pts',(-7.53940549437943,0.699383189958536,
19.4337846781447));
#15287=CARTESIAN_POINT('Ctrl Pts',(-7.71522634131211,0.940871035194129,
19.445787864934));
#15288=CARTESIAN_POINT('Ctrl Pts',(-7.98526240565883,1.11182427083128,19.4577910517233));
#15289=CARTESIAN_POINT('Ctrl Pts',(-8.27875123560222,1.16744491727767,19.4697942385126));
#15290=CARTESIAN_POINT('Ctrl Pts',(-8.57224006554561,1.22306556372405,19.4817974253019));
#15291=CARTESIAN_POINT('Ctrl Pts',(-8.88610136060047,1.16276985666989,19.4938006120912));
#15292=CARTESIAN_POINT('Ctrl Pts',(-9.13808834820187,1.0023581747629,19.5058037988806));
#15293=CARTESIAN_POINT('Ctrl Pts',(-9.39007533580326,0.841946492855913,
19.5178069856699));
#15294=CARTESIAN_POINT('Ctrl Pts',(-9.57754329642192,0.5831024306019,19.5298101724592));
#15295=CARTESIAN_POINT('Ctrl Pts',(-9.65136659729219,0.293655596345123,
19.5418133592485));
#15296=CARTESIAN_POINT('Ctrl Pts',(-9.67581103310559,0.197813707971494,
19.545787864934));
#15297=CARTESIAN_POINT('Ctrl Pts',(-9.68822500000007,0.0989100500914754,
19.5497623706194));
#15298=CARTESIAN_POINT('Ctrl Pts',(-9.688225,-8.10851386034983E-13,19.5537368763049));
#15299=CARTESIAN_POINT('Origin',(-8.5,0.,1.8));
#15300=CARTESIAN_POINT('',(-9.688225,8.64530669275609E-13,19.8962631236951));
#15301=CARTESIAN_POINT('',(-9.688225,-8.52762305214583E-13,19.8537368763049));
#15302=CARTESIAN_POINT('',(-9.688225,-1.45515594291686E-16,1.8));
#15303=CARTESIAN_POINT('Ctrl Pts',(-9.688225,7.96918087075937E-13,19.8962631236951));
#15304=CARTESIAN_POINT('Ctrl Pts',(-9.6882249999998,0.298712821306902,19.8842599369058));
#15305=CARTESIAN_POINT('Ctrl Pts',(-9.57054245632545,0.595858078272269,
19.8722567501165));
#15306=CARTESIAN_POINT('Ctrl Pts',(-9.36601586214878,0.813569405233325,
19.8602535633272));
#15307=CARTESIAN_POINT('Ctrl Pts',(-9.16148926797211,1.03128073219438,19.8482503765379));
#15308=CARTESIAN_POINT('Ctrl Pts',(-8.87226522412763,1.16727314847163,19.8362471897486));
#15309=CARTESIAN_POINT('Ctrl Pts',(-8.57413435701364,1.18591009260195,19.8242440029592));
#15310=CARTESIAN_POINT('Ctrl Pts',(-8.27600348989966,1.20454703673228,19.8122408161699));
#15311=CARTESIAN_POINT('Ctrl Pts',(-7.97209482032013,1.10563290540071,19.8002376293806));
#15312=CARTESIAN_POINT('Ctrl Pts',(-7.74204705371994,0.915087963996017,
19.7882344425913));
#15313=CARTESIAN_POINT('Ctrl Pts',(-7.51199928711975,0.724543022591324,
19.776231255802));
#15314=CARTESIAN_POINT('Ctrl Pts',(-7.35822688079601,0.444367128060612,
19.7642280690126));
#15315=CARTESIAN_POINT('Ctrl Pts',(-7.32102560975806,0.147979855989401,
19.7522248822233));
#15316=CARTESIAN_POINT('Ctrl Pts',(-7.28382433872011,-0.14840741608181,
19.740221695434));
#15317=CARTESIAN_POINT('Ctrl Pts',(-7.36358464744672,-0.45789534472284,
19.7282185086447));
#15318=CARTESIAN_POINT('Ctrl Pts',(-7.53940549437937,-0.699383189958449,
19.7162153218554));
#15319=CARTESIAN_POINT('Ctrl Pts',(-7.71522634131202,-0.940871035194058,
19.7042121350661));
#15320=CARTESIAN_POINT('Ctrl Pts',(-7.98526240565873,-1.11182427083124,
19.6922089482767));
#15321=CARTESIAN_POINT('Ctrl Pts',(-8.27875123560211,-1.16744491727765,
19.6802057614874));
#15322=CARTESIAN_POINT('Ctrl Pts',(-8.5722400655455,-1.22306556372405,19.6682025746981));
#15323=CARTESIAN_POINT('Ctrl Pts',(-8.88610136060037,-1.16276985666993,
19.6561993879088));
#15324=CARTESIAN_POINT('Ctrl Pts',(-9.13808834820177,-1.00235817476296,
19.6441962011195));
#15325=CARTESIAN_POINT('Ctrl Pts',(-9.39007533580318,-0.841946492855994,
19.6321930143301));
#15326=CARTESIAN_POINT('Ctrl Pts',(-9.57754329642186,-0.583102430601997,
19.6201898275408));
#15327=CARTESIAN_POINT('Ctrl Pts',(-9.65136659729216,-0.293655596345227,
19.6081866407515));
#15328=CARTESIAN_POINT('Ctrl Pts',(-9.67581103310559,-0.197813707971534,
19.6042121350661));
#15329=CARTESIAN_POINT('Ctrl Pts',(-9.68822500000008,-0.0989100500914475,
19.6002376293806));
#15330=CARTESIAN_POINT('Ctrl Pts',(-9.688225,9.06386077303978E-13,19.5962631236951));
#15331=CARTESIAN_POINT('Ctrl Pts',(-9.688225,-8.10851386034983E-13,19.5537368763049));
#15332=CARTESIAN_POINT('Ctrl Pts',(-9.68822499999979,-0.298712821306893,
19.5657400630942));
#15333=CARTESIAN_POINT('Ctrl Pts',(-9.57054245632546,-0.595858078272237,
19.5777432498835));
#15334=CARTESIAN_POINT('Ctrl Pts',(-9.36601586214882,-0.813569405233286,
19.5897464366728));
#15335=CARTESIAN_POINT('Ctrl Pts',(-9.16148926797217,-1.03128073219433,
19.6017496234621));
#15336=CARTESIAN_POINT('Ctrl Pts',(-8.87226522412772,-1.16727314847159,
19.6137528102515));
#15337=CARTESIAN_POINT('Ctrl Pts',(-8.57413435701376,-1.18591009260195,
19.6257559970408));
#15338=CARTESIAN_POINT('Ctrl Pts',(-8.2760034898998,-1.2045470367323,19.6377591838301));
#15339=CARTESIAN_POINT('Ctrl Pts',(-7.97209482032029,-1.10563290540078,
19.6497623706194));
#15340=CARTESIAN_POINT('Ctrl Pts',(-7.74204705372008,-0.915087963996137,
19.6617655574087));
#15341=CARTESIAN_POINT('Ctrl Pts',(-7.51199928711988,-0.724543022591495,
19.673768744198));
#15342=CARTESIAN_POINT('Ctrl Pts',(-7.3582268807961,-0.444367128060836,
19.6857719309874));
#15343=CARTESIAN_POINT('Ctrl Pts',(-7.32102560975809,-0.147979855989656,
19.6977751177767));
#15344=CARTESIAN_POINT('Ctrl Pts',(-7.28382433872008,0.148407416081525,
19.709778304566));
#15345=CARTESIAN_POINT('Ctrl Pts',(-7.36358464744661,0.457895344722549,
19.7217814913553));
#15346=CARTESIAN_POINT('Ctrl Pts',(-7.53940549437918,0.699383189958187,
19.7337846781446));
#15347=CARTESIAN_POINT('Ctrl Pts',(-7.71522634131175,0.940871035193826,
19.745787864934));
#15348=CARTESIAN_POINT('Ctrl Pts',(-7.98526240565838,1.11182427083107,19.7577910517233));
#15349=CARTESIAN_POINT('Ctrl Pts',(-8.27875123560173,1.16744491727757,19.7697942385126));
#15350=CARTESIAN_POINT('Ctrl Pts',(-8.57224006554507,1.22306556372407,19.7817974253019));
#15351=CARTESIAN_POINT('Ctrl Pts',(-8.88610136059994,1.16276985667006,19.7938006120912));
#15352=CARTESIAN_POINT('Ctrl Pts',(-9.13808834820139,1.00235817476321,19.8058037988805));
#15353=CARTESIAN_POINT('Ctrl Pts',(-9.39007533580284,0.84194649285635,19.8178069856699));
#15354=CARTESIAN_POINT('Ctrl Pts',(-9.57754329642161,0.583102430602453,
19.8298101724592));
#15355=CARTESIAN_POINT('Ctrl Pts',(-9.65136659729203,0.293655596345737,
19.8418133592485));
#15356=CARTESIAN_POINT('Ctrl Pts',(-9.67581103310554,0.197813707971903,
19.845787864934));
#15357=CARTESIAN_POINT('Ctrl Pts',(-9.68822500000007,0.0989100500916587,
19.8497623706194));
#15358=CARTESIAN_POINT('Ctrl Pts',(-9.688225,-8.52762305214583E-13,19.8537368763049));
#15359=CARTESIAN_POINT('Origin',(-8.5,0.,1.8));
#15360=CARTESIAN_POINT('',(-9.688225,8.90176821144451E-13,20.1962631236951));
#15361=CARTESIAN_POINT('',(-9.688225,-8.27171664496973E-13,20.1537368763049));
#15362=CARTESIAN_POINT('',(-9.688225,-1.45515594291686E-16,1.8));
#15363=CARTESIAN_POINT('Ctrl Pts',(-9.688225,9.5767838104166E-13,20.1962631236951));
#15364=CARTESIAN_POINT('Ctrl Pts',(-9.68822499999976,0.29871282130704,20.1842599369058));
#15365=CARTESIAN_POINT('Ctrl Pts',(-9.57054245632539,0.595858078272369,
20.1722567501165));
#15366=CARTESIAN_POINT('Ctrl Pts',(-9.36601586214872,0.813569405233393,
20.1602535633272));
#15367=CARTESIAN_POINT('Ctrl Pts',(-9.16148926797204,1.03128073219442,20.1482503765379));
#15368=CARTESIAN_POINT('Ctrl Pts',(-8.87226522412758,1.16727314847164,20.1362471897486));
#15369=CARTESIAN_POINT('Ctrl Pts',(-8.57413435701362,1.18591009260196,20.1242440029592));
#15370=CARTESIAN_POINT('Ctrl Pts',(-8.27600348989965,1.20454703673228,20.1122408161699));
#15371=CARTESIAN_POINT('Ctrl Pts',(-7.97209482032015,1.10563290540071,20.1002376293806));
#15372=CARTESIAN_POINT('Ctrl Pts',(-7.74204705371997,0.915087963996044,
20.0882344425913));
#15373=CARTESIAN_POINT('Ctrl Pts',(-7.51199928711979,0.724543022591373,
20.076231255802));
#15374=CARTESIAN_POINT('Ctrl Pts',(-7.35822688079604,0.444367128060695,
20.0642280690126));
#15375=CARTESIAN_POINT('Ctrl Pts',(-7.32102560975807,0.14797985598951,20.0522248822233));
#15376=CARTESIAN_POINT('Ctrl Pts',(-7.2838243387201,-0.148407416081675,
20.040221695434));
#15377=CARTESIAN_POINT('Ctrl Pts',(-7.36358464744666,-0.457895344722689,
20.0282185086447));
#15378=CARTESIAN_POINT('Ctrl Pts',(-7.53940549437926,-0.699383189958306,
20.0162153218554));
#15379=CARTESIAN_POINT('Ctrl Pts',(-7.71522634131187,-0.940871035193923,
20.0042121350661));
#15380=CARTESIAN_POINT('Ctrl Pts',(-7.98526240565852,-1.11182427083114,
19.9922089482767));
#15381=CARTESIAN_POINT('Ctrl Pts',(-8.27875123560187,-1.1674449172776,19.9802057614874));
#15382=CARTESIAN_POINT('Ctrl Pts',(-8.57224006554522,-1.22306556372406,
19.9682025746981));
#15383=CARTESIAN_POINT('Ctrl Pts',(-8.88610136060008,-1.16276985667001,
19.9561993879088));
#15384=CARTESIAN_POINT('Ctrl Pts',(-9.13808834820151,-1.00235817476313,
19.9441962011195));
#15385=CARTESIAN_POINT('Ctrl Pts',(-9.39007533580294,-0.84194649285624,
19.9321930143302));
#15386=CARTESIAN_POINT('Ctrl Pts',(-9.57754329642168,-0.58310243060232,
19.9201898275408));
#15387=CARTESIAN_POINT('Ctrl Pts',(-9.65136659729207,-0.293655596345595,
19.9081866407515));
#15388=CARTESIAN_POINT('Ctrl Pts',(-9.67581103310554,-0.197813707971823,
19.9042121350661));
#15389=CARTESIAN_POINT('Ctrl Pts',(-9.68822500000007,-0.098910050091647,
19.9002376293806));
#15390=CARTESIAN_POINT('Ctrl Pts',(-9.688225,7.96918087075937E-13,19.8962631236951));
#15391=CARTESIAN_POINT('Ctrl Pts',(-9.688225,-8.52762305214583E-13,19.8537368763049));
#15392=CARTESIAN_POINT('Ctrl Pts',(-9.68822499999978,-0.298712821306935,
19.8657400630942));
#15393=CARTESIAN_POINT('Ctrl Pts',(-9.57054245632544,-0.595858078272275,
19.8777432498835));
#15394=CARTESIAN_POINT('Ctrl Pts',(-9.36601586214879,-0.813569405233316,
19.8897464366728));
#15395=CARTESIAN_POINT('Ctrl Pts',(-9.16148926797213,-1.03128073219436,
19.9017496234621));
#15396=CARTESIAN_POINT('Ctrl Pts',(-8.87226522412768,-1.1672731484716,19.9137528102515));
#15397=CARTESIAN_POINT('Ctrl Pts',(-8.57413435701372,-1.18591009260195,
19.9257559970408));
#15398=CARTESIAN_POINT('Ctrl Pts',(-8.27600348989976,-1.20454703673229,
19.9377591838301));
#15399=CARTESIAN_POINT('Ctrl Pts',(-7.97209482032025,-1.10563290540076,
19.9497623706194));
#15400=CARTESIAN_POINT('Ctrl Pts',(-7.74204705372005,-0.915087963996111,
19.9617655574087));
#15401=CARTESIAN_POINT('Ctrl Pts',(-7.51199928711986,-0.72454302259146,
19.9737687441981));
#15402=CARTESIAN_POINT('Ctrl Pts',(-7.35822688079608,-0.444367128060796,
19.9857719309874));
#15403=CARTESIAN_POINT('Ctrl Pts',(-7.32102560975809,-0.147979855989614,
19.9977751177767));
#15404=CARTESIAN_POINT('Ctrl Pts',(-7.28382433872009,0.148407416081568,
20.009778304566));
#15405=CARTESIAN_POINT('Ctrl Pts',(-7.36358464744662,0.457895344722589,
20.0217814913553));
#15406=CARTESIAN_POINT('Ctrl Pts',(-7.5394054943792,0.699383189958221,20.0337846781446));
#15407=CARTESIAN_POINT('Ctrl Pts',(-7.71522634131179,0.940871035193854,
20.045787864934));
#15408=CARTESIAN_POINT('Ctrl Pts',(-7.98526240565842,1.11182427083109,20.0577910517233));
#15409=CARTESIAN_POINT('Ctrl Pts',(-8.27875123560177,1.16744491727758,20.0697942385126));
#15410=CARTESIAN_POINT('Ctrl Pts',(-8.57224006554511,1.22306556372407,20.0817974253019));
#15411=CARTESIAN_POINT('Ctrl Pts',(-8.88610136059998,1.16276985667005,20.0938006120912));
#15412=CARTESIAN_POINT('Ctrl Pts',(-9.13808834820142,1.00235817476318,20.1058037988805));
#15413=CARTESIAN_POINT('Ctrl Pts',(-9.39007533580287,0.841946492856318,
20.1178069856699));
#15414=CARTESIAN_POINT('Ctrl Pts',(-9.57754329642163,0.583102430602415,
20.1298101724592));
#15415=CARTESIAN_POINT('Ctrl Pts',(-9.65136659729204,0.293655596345696,
20.1418133592485));
#15416=CARTESIAN_POINT('Ctrl Pts',(-9.67581103310554,0.197813707971883,
20.145787864934));
#15417=CARTESIAN_POINT('Ctrl Pts',(-9.68822500000007,0.0989100500916617,
20.1497623706194));
#15418=CARTESIAN_POINT('Ctrl Pts',(-9.688225,-8.27171664496973E-13,20.1537368763049));
#15419=CARTESIAN_POINT('Origin',(-8.5,0.,1.8));
#15420=CARTESIAN_POINT('',(-9.688225,9.15711950710829E-13,20.4962631236951));
#15421=CARTESIAN_POINT('',(-9.688225,-8.01581023779363E-13,20.4537368763049));
#15422=CARTESIAN_POINT('',(-9.688225,-1.45515594291686E-16,1.8));
#15423=CARTESIAN_POINT('Ctrl Pts',(-9.688225,9.15711950710829E-13,20.4962631236951));
#15424=CARTESIAN_POINT('Ctrl Pts',(-9.68822499999977,0.298712821306998,
20.4842599369058));
#15425=CARTESIAN_POINT('Ctrl Pts',(-9.57054245632541,0.595858078272332,
20.4722567501165));
#15426=CARTESIAN_POINT('Ctrl Pts',(-9.36601586214874,0.813569405233362,
20.4602535633272));
#15427=CARTESIAN_POINT('Ctrl Pts',(-9.16148926797208,1.03128073219439,20.4482503765379));
#15428=CARTESIAN_POINT('Ctrl Pts',(-8.87226522412762,1.16727314847162,20.4362471897486));
#15429=CARTESIAN_POINT('Ctrl Pts',(-8.57413435701366,1.18591009260195,20.4242440029592));
#15430=CARTESIAN_POINT('Ctrl Pts',(-8.2760034898997,1.20454703673228,20.4122408161699));
#15431=CARTESIAN_POINT('Ctrl Pts',(-7.97209482032019,1.10563290540073,20.4002376293806));
#15432=CARTESIAN_POINT('Ctrl Pts',(-7.74204705372,0.915087963996071,20.3882344425913));
#15433=CARTESIAN_POINT('Ctrl Pts',(-7.51199928711982,0.724543022591408,
20.376231255802));
#15434=CARTESIAN_POINT('Ctrl Pts',(-7.35822688079606,0.444367128060736,
20.3642280690127));
#15435=CARTESIAN_POINT('Ctrl Pts',(-7.32102560975808,0.147979855989552,
20.3522248822233));
#15436=CARTESIAN_POINT('Ctrl Pts',(-7.28382433872009,-0.148407416081632,
20.340221695434));
#15437=CARTESIAN_POINT('Ctrl Pts',(-7.36358464744665,-0.457895344722649,
20.3282185086447));
#15438=CARTESIAN_POINT('Ctrl Pts',(-7.53940549437924,-0.699383189958272,
20.3162153218554));
#15439=CARTESIAN_POINT('Ctrl Pts',(-7.71522634131184,-0.940871035193895,
20.3042121350661));
#15440=CARTESIAN_POINT('Ctrl Pts',(-7.98526240565848,-1.11182427083112,
20.2922089482767));
#15441=CARTESIAN_POINT('Ctrl Pts',(-8.27875123560183,-1.16744491727759,
20.2802057614874));
#15442=CARTESIAN_POINT('Ctrl Pts',(-8.57224006554518,-1.22306556372407,
20.2682025746981));
#15443=CARTESIAN_POINT('Ctrl Pts',(-8.88610136060004,-1.16276985667003,
20.2561993879088));
#15444=CARTESIAN_POINT('Ctrl Pts',(-9.13808834820148,-1.00235817476315,
20.2441962011195));
#15445=CARTESIAN_POINT('Ctrl Pts',(-9.39007533580291,-0.841946492856271,
20.2321930143302));
#15446=CARTESIAN_POINT('Ctrl Pts',(-9.57754329642166,-0.583102430602358,
20.2201898275408));
#15447=CARTESIAN_POINT('Ctrl Pts',(-9.65136659729206,-0.293655596345635,
20.2081866407515));
#15448=CARTESIAN_POINT('Ctrl Pts',(-9.67581103310556,-0.197813707971799,
20.2042121350661));
#15449=CARTESIAN_POINT('Ctrl Pts',(-9.68822500000008,-0.0989100500915538,
20.2002376293806));
#15450=CARTESIAN_POINT('Ctrl Pts',(-9.688225,9.5767838104166E-13,20.1962631236951));
#15451=CARTESIAN_POINT('Ctrl Pts',(-9.688225,-8.27171664496973E-13,20.1537368763049));
#15452=CARTESIAN_POINT('Ctrl Pts',(-9.68822499999979,-0.298712821306932,
20.1657400630942));
#15453=CARTESIAN_POINT('Ctrl Pts',(-9.57054245632544,-0.595858078272296,
20.1777432498835));
#15454=CARTESIAN_POINT('Ctrl Pts',(-9.36601586214876,-0.813569405233347,
20.1897464366728));
#15455=CARTESIAN_POINT('Ctrl Pts',(-9.16148926797208,-1.0312807321944,20.2017496234621));
#15456=CARTESIAN_POINT('Ctrl Pts',(-8.8722652241276,-1.16727314847164,20.2137528102515));
#15457=CARTESIAN_POINT('Ctrl Pts',(-8.57413435701361,-1.18591009260196,
20.2257559970408));
#15458=CARTESIAN_POINT('Ctrl Pts',(-8.27600348989963,-1.20454703673228,
20.2377591838301));
#15459=CARTESIAN_POINT('Ctrl Pts',(-7.9720948203201,-1.1056329054007,20.2497623706194));
#15460=CARTESIAN_POINT('Ctrl Pts',(-7.74204705371992,-0.915087963995998,
20.2617655574087));
#15461=CARTESIAN_POINT('Ctrl Pts',(-7.51199928711973,-0.724543022591299,
20.2737687441981));
#15462=CARTESIAN_POINT('Ctrl Pts',(-7.358226880796,-0.444367128060583,20.2857719309874));
#15463=CARTESIAN_POINT('Ctrl Pts',(-7.32102560975806,-0.147979855989371,
20.2977751177767));
#15464=CARTESIAN_POINT('Ctrl Pts',(-7.28382433872012,0.14840741608184,20.309778304566));
#15465=CARTESIAN_POINT('Ctrl Pts',(-7.36358464744673,0.457895344722869,
20.3217814913553));
#15466=CARTESIAN_POINT('Ctrl Pts',(-7.53940549437939,0.699383189958473,
20.3337846781446));
#15467=CARTESIAN_POINT('Ctrl Pts',(-7.71522634131205,0.940871035194078,
20.345787864934));
#15468=CARTESIAN_POINT('Ctrl Pts',(-7.98526240565876,1.11182427083125,20.3577910517233));
#15469=CARTESIAN_POINT('Ctrl Pts',(-8.27875123560214,1.16744491727765,20.3697942385126));
#15470=CARTESIAN_POINT('Ctrl Pts',(-8.57224006554553,1.22306556372405,20.3817974253019));
#15471=CARTESIAN_POINT('Ctrl Pts',(-8.8861013606004,1.16276985666991,20.3938006120912));
#15472=CARTESIAN_POINT('Ctrl Pts',(-9.1380883482018,1.00235817476294,20.4058037988806));
#15473=CARTESIAN_POINT('Ctrl Pts',(-9.3900753358032,0.841946492855971,20.4178069856699));
#15474=CARTESIAN_POINT('Ctrl Pts',(-9.57754329642188,0.58310243060197,20.4298101724592));
#15475=CARTESIAN_POINT('Ctrl Pts',(-9.65136659729217,0.293655596345198,
20.4418133592485));
#15476=CARTESIAN_POINT('Ctrl Pts',(-9.67581103310558,0.197813707971548,
20.445787864934));
#15477=CARTESIAN_POINT('Ctrl Pts',(-9.68822500000007,0.0989100500915072,
20.4497623706194));
#15478=CARTESIAN_POINT('Ctrl Pts',(-9.688225,-8.01581023779363E-13,20.4537368763049));
#15479=CARTESIAN_POINT('Origin',(-8.5,0.,1.8));
#15480=CARTESIAN_POINT('',(-9.688225,9.41247080277208E-13,20.7962631236951));
#15481=CARTESIAN_POINT('',(-9.68836223994391,0.000210585078932092,20.7537368763049));
#15482=CARTESIAN_POINT('',(-9.688225,-1.45515594291686E-16,1.8));
#15483=CARTESIAN_POINT('Ctrl Pts',(-9.688225,1.00885966247688E-12,20.7962631236951));
#15484=CARTESIAN_POINT('Ctrl Pts',(-9.68822499999975,0.298712821307114,
20.7842599369058));
#15485=CARTESIAN_POINT('Ctrl Pts',(-9.57054245632535,0.59585807827246,20.7722567501165));
#15486=CARTESIAN_POINT('Ctrl Pts',(-9.36601586214863,0.813569405233479,
20.7602535633272));
#15487=CARTESIAN_POINT('Ctrl Pts',(-9.16148926797192,1.0312807321945,20.7482503765379));
#15488=CARTESIAN_POINT('Ctrl Pts',(-8.87226522412742,1.16727314847169,20.7362471897485));
#15489=CARTESIAN_POINT('Ctrl Pts',(-8.57413435701343,1.18591009260197,20.7242440029592));
#15490=CARTESIAN_POINT('Ctrl Pts',(-8.27600348989944,1.20454703673224,20.7122408161699));
#15491=CARTESIAN_POINT('Ctrl Pts',(-7.97209482031993,1.10563290540062,20.7002376293806));
#15492=CARTESIAN_POINT('Ctrl Pts',(-7.74204705371978,0.915087963995882,
20.6882344425913));
#15493=CARTESIAN_POINT('Ctrl Pts',(-7.51199928711962,0.724543022591148,
20.676231255802));
#15494=CARTESIAN_POINT('Ctrl Pts',(-7.35822688079593,0.444367128060409,
20.6642280690126));
#15495=CARTESIAN_POINT('Ctrl Pts',(-7.32102560975803,0.147979855989191,
20.6522248822233));
#15496=CARTESIAN_POINT('Ctrl Pts',(-7.28382433872014,-0.148407416082027,
20.640221695434));
#15497=CARTESIAN_POINT('Ctrl Pts',(-7.3635846474468,-0.457895344723043,
20.6282185086447));
#15498=CARTESIAN_POINT('Ctrl Pts',(-7.53940549437949,-0.699383189958621,
20.6162153218554));
#15499=CARTESIAN_POINT('Ctrl Pts',(-7.71522634131219,-0.940871035194198,
20.604212135066));
#15500=CARTESIAN_POINT('Ctrl Pts',(-7.98526240565893,-1.11182427083133,
20.5922089482767));
#15501=CARTESIAN_POINT('Ctrl Pts',(-8.27875123560232,-1.16744491727769,
20.5802057614874));
#15502=CARTESIAN_POINT('Ctrl Pts',(-8.57224006554571,-1.22306556372404,
20.5682025746981));
#15503=CARTESIAN_POINT('Ctrl Pts',(-8.88610136060058,-1.16276985666986,
20.5561993879088));
#15504=CARTESIAN_POINT('Ctrl Pts',(-9.13808834820195,-1.00235817476285,
20.5441962011195));
#15505=CARTESIAN_POINT('Ctrl Pts',(-9.39007533580333,-0.841946492855835,
20.5321930143301));
#15506=CARTESIAN_POINT('Ctrl Pts',(-9.57754329642197,-0.583102430601805,
20.5201898275408));
#15507=CARTESIAN_POINT('Ctrl Pts',(-9.65136659729221,-0.293655596345021,
20.5081866407515));
#15508=CARTESIAN_POINT('Ctrl Pts',(-9.6758110331056,-0.19781370797139,20.504212135066));
#15509=CARTESIAN_POINT('Ctrl Pts',(-9.68822500000008,-0.0989100500913706,
20.5002376293806));
#15510=CARTESIAN_POINT('Ctrl Pts',(-9.688225,9.15711950710829E-13,20.4962631236951));
#15511=CARTESIAN_POINT('Ctrl Pts',(-9.688225,-8.01581023779363E-13,20.4537368763049));
#15512=CARTESIAN_POINT('Ctrl Pts',(-9.6882249999998,-0.298712821306884,
20.4657400630942));
#15513=CARTESIAN_POINT('Ctrl Pts',(-9.57054245632547,-0.595858078272229,
20.4777432498835));
#15514=CARTESIAN_POINT('Ctrl Pts',(-9.36601586214882,-0.813569405233279,
20.4897464366728));
#15515=CARTESIAN_POINT('Ctrl Pts',(-9.16148926797218,-1.03128073219433,
20.5017496234621));
#15516=CARTESIAN_POINT('Ctrl Pts',(-8.87226522412773,-1.16727314847159,
20.5137528102515));
#15517=CARTESIAN_POINT('Ctrl Pts',(-8.57413435701377,-1.18591009260195,
20.5257559970408));
#15518=CARTESIAN_POINT('Ctrl Pts',(-8.27600348989981,-1.2045470367323,20.5377591838301));
#15519=CARTESIAN_POINT('Ctrl Pts',(-7.97209482032029,-1.10563290540078,
20.5497623706194));
#15520=CARTESIAN_POINT('Ctrl Pts',(-7.74204705372009,-0.915087963996143,
20.5617655574087));
#15521=CARTESIAN_POINT('Ctrl Pts',(-7.51199928711989,-0.724543022591503,
20.573768744198));
#15522=CARTESIAN_POINT('Ctrl Pts',(-7.3582268807961,-0.444367128060845,
20.5857719309874));
#15523=CARTESIAN_POINT('Ctrl Pts',(-7.32102560975809,-0.147979855989665,
20.5977751177767));
#15524=CARTESIAN_POINT('Ctrl Pts',(-7.28382433872008,0.148407416081515,
20.609778304566));
#15525=CARTESIAN_POINT('Ctrl Pts',(-7.3635846474466,0.45789534472254,20.6217814913553));
#15526=CARTESIAN_POINT('Ctrl Pts',(-7.53940549437917,0.69938318995818,20.6337846781446));
#15527=CARTESIAN_POINT('Ctrl Pts',(-7.71522634131175,0.94087103519382,20.645787864934));
#15528=CARTESIAN_POINT('Ctrl Pts',(-7.98526240565837,1.11182427083107,20.6577910517233));
#15529=CARTESIAN_POINT('Ctrl Pts',(-8.27875123560172,1.16744491727757,20.6697942385126));
#15530=CARTESIAN_POINT('Ctrl Pts',(-8.57224006554506,1.22306556372407,20.6817974253019));
#15531=CARTESIAN_POINT('Ctrl Pts',(-8.88610136059993,1.16276985667007,20.6938006120912));
#15532=CARTESIAN_POINT('Ctrl Pts',(-9.13808834820138,1.00235817476321,20.7058037988805));
#15533=CARTESIAN_POINT('Ctrl Pts',(-9.39007533580283,0.841946492856357,
20.7178069856699));
#15534=CARTESIAN_POINT('Ctrl Pts',(-9.57754329642161,0.583102430602461,
20.7298101724592));
#15535=CARTESIAN_POINT('Ctrl Pts',(-9.65136659729203,0.293655596345746,
20.7418133592485));
#15536=CARTESIAN_POINT('Ctrl Pts',(-9.67581103310553,0.197813707971934,
20.7457878649339));
#15537=CARTESIAN_POINT('Ctrl Pts',(-9.68822500000006,0.098910050091713,
20.7497623706194));
#15538=CARTESIAN_POINT('Ctrl Pts',(-9.688225,-7.75879360759291E-13,20.7537368763049));
#15539=CARTESIAN_POINT('Origin',(-8.5,0.,1.8));
#15540=CARTESIAN_POINT('',(-9.688225,9.66893232146049E-13,21.0962631236951));
#15541=CARTESIAN_POINT('',(-9.6874221426744,0.000106455689637072,21.0537368763049));
#15542=CARTESIAN_POINT('',(-9.688225,-1.45515594291686E-16,1.8));
#15543=CARTESIAN_POINT('Ctrl Pts',(-9.688225,9.66893232146049E-13,21.0962631236951));
#15544=CARTESIAN_POINT('Ctrl Pts',(-9.68822499999976,0.298712821307072,
21.0842599369058));
#15545=CARTESIAN_POINT('Ctrl Pts',(-9.57054245632537,0.595858078272422,
21.0722567501165));
#15546=CARTESIAN_POINT('Ctrl Pts',(-9.36601586214866,0.813569405233449,
21.0602535633272));
#15547=CARTESIAN_POINT('Ctrl Pts',(-9.16148926797196,1.03128073219448,21.0482503765379));
#15548=CARTESIAN_POINT('Ctrl Pts',(-8.87226522412746,1.16727314847168,21.0362471897485));
#15549=CARTESIAN_POINT('Ctrl Pts',(-8.57413435701347,1.18591009260196,21.0242440029592));
#15550=CARTESIAN_POINT('Ctrl Pts',(-8.27600348989949,1.20454703673225,21.0122408161699));
#15551=CARTESIAN_POINT('Ctrl Pts',(-7.97209482031997,1.10563290540063,21.0002376293806));
#15552=CARTESIAN_POINT('Ctrl Pts',(-7.74204705371981,0.915087963995909,
20.9882344425913));
#15553=CARTESIAN_POINT('Ctrl Pts',(-7.51199928711965,0.724543022591183,
20.976231255802));
#15554=CARTESIAN_POINT('Ctrl Pts',(-7.35822688079594,0.444367128060449,
20.9642280690126));
#15555=CARTESIAN_POINT('Ctrl Pts',(-7.32102560975804,0.147979855989233,
20.9522248822233));
#15556=CARTESIAN_POINT('Ctrl Pts',(-7.28382433872013,-0.148407416081984,
20.940221695434));
#15557=CARTESIAN_POINT('Ctrl Pts',(-7.36358464744678,-0.457895344723003,
20.9282185086447));
#15558=CARTESIAN_POINT('Ctrl Pts',(-7.53940549437947,-0.699383189958587,
20.9162153218554));
#15559=CARTESIAN_POINT('Ctrl Pts',(-7.71522634131216,-0.940871035194171,
20.904212135066));
#15560=CARTESIAN_POINT('Ctrl Pts',(-7.98526240565889,-1.11182427083131,
20.8922089482767));
#15561=CARTESIAN_POINT('Ctrl Pts',(-8.27875123560228,-1.16744491727768,
20.8802057614874));
#15562=CARTESIAN_POINT('Ctrl Pts',(-8.57224006554567,-1.22306556372404,
20.8682025746981));
#15563=CARTESIAN_POINT('Ctrl Pts',(-8.88610136060053,-1.16276985666987,
20.8561993879088));
#15564=CARTESIAN_POINT('Ctrl Pts',(-9.13808834820192,-1.00235817476287,
20.8441962011195));
#15565=CARTESIAN_POINT('Ctrl Pts',(-9.3900753358033,-0.841946492855867,
20.8321930143301));
#15566=CARTESIAN_POINT('Ctrl Pts',(-9.57754329642195,-0.583102430601843,
20.8201898275408));
#15567=CARTESIAN_POINT('Ctrl Pts',(-9.6513665972922,-0.293655596345062,
20.8081866407515));
#15568=CARTESIAN_POINT('Ctrl Pts',(-9.67581103310561,-0.197813707971388,
20.804212135066));
#15569=CARTESIAN_POINT('Ctrl Pts',(-9.68822500000008,-0.0989100500913225,
20.8002376293806));
#15570=CARTESIAN_POINT('Ctrl Pts',(-9.688225,1.00885966247688E-12,20.7962631236951));
#15571=CARTESIAN_POINT('Ctrl Pts',(-9.68885519676553,0.00096699279630702,
20.7537368763049));
#15572=CARTESIAN_POINT('Ctrl Pts',(-9.68602600941174,-0.327109604903285,
20.7669463625483));
#15573=CARTESIAN_POINT('Ctrl Pts',(-9.54497968579521,-0.657370321733589,
20.7801558487917));
#15574=CARTESIAN_POINT('Ctrl Pts',(-9.30343789015976,-0.878224528088828,
20.7933653350352));
#15575=CARTESIAN_POINT('Ctrl Pts',(-9.01256452273736,-1.14418515218266,
20.8092726761868));
#15576=CARTESIAN_POINT('Ctrl Pts',(-8.57595415348136,-1.25148612229012,
20.8251800173384));
#15577=CARTESIAN_POINT('Ctrl Pts',(-8.1952758127627,-1.1506442032281,20.84108735849));
#15578=CARTESIAN_POINT('Ctrl Pts',(-7.81459747204409,-1.0498022841661,20.8569946996417));
#15579=CARTESIAN_POINT('Ctrl Pts',(-7.48985115986283,-0.740817475934675,
20.8729020407933));
#15580=CARTESIAN_POINT('Ctrl Pts',(-7.36788212617543,-0.365790383070442,
20.8888093819449));
#15581=CARTESIAN_POINT('Ctrl Pts',(-7.30689760933172,-0.178276836638304,
20.8967630525207));
#15582=CARTESIAN_POINT('Ctrl Pts',(-7.2966074121115,0.025747280952097,20.9047167230965));
#15583=CARTESIAN_POINT('Ctrl Pts',(-7.33354022386741,0.220831256234288,
20.9126703936723));
#15584=CARTESIAN_POINT('Ctrl Pts',(-7.37047303562331,0.415915231516458,
20.9206240642481));
#15585=CARTESIAN_POINT('Ctrl Pts',(-7.45462885635533,0.602059064490469,
20.928577734824));
#15586=CARTESIAN_POINT('Ctrl Pts',(-7.57993567741204,0.754304399351246,
20.9365314053998));
#15587=CARTESIAN_POINT('Ctrl Pts',(-7.83054931952548,1.05879506907282,20.9524387465514));
#15588=CARTESIAN_POINT('Ctrl Pts',(-8.2457669629377,1.2276917463414,20.968346087703));
#15589=CARTESIAN_POINT('Ctrl Pts',(-8.63696275298426,1.18240437964549,20.9842534288546));
#15590=CARTESIAN_POINT('Ctrl Pts',(-9.02815854303084,1.13711701294958,21.0001607700063));
#15591=CARTESIAN_POINT('Ctrl Pts',(-9.39533247971174,0.87764560228914,21.0160681111579));
#15592=CARTESIAN_POINT('Ctrl Pts',(-9.56885922347405,0.523765907133755,
21.0319754523095));
#15593=CARTESIAN_POINT('Ctrl Pts',(-9.64798807787227,0.362395421724354,
21.039229260308));
#15594=CARTESIAN_POINT('Ctrl Pts',(-9.68685003861911,0.181393728166409,
21.0464830683064));
#15595=CARTESIAN_POINT('Ctrl Pts',(-9.68638548896517,0.000243911851261936,
21.0537368763049));
#15596=CARTESIAN_POINT('Origin',(-8.5,0.,1.8));
#15597=CARTESIAN_POINT('',(-9.688225,9.92650406317352E-13,21.3962631236951));
#15598=CARTESIAN_POINT('',(-9.688225,-7.2464256817284E-13,21.3537368763049));
#15599=CARTESIAN_POINT('',(-9.688225,-1.45515594291686E-16,1.8));
#15600=CARTESIAN_POINT('Ctrl Pts',(-9.688225,1.0600409439121E-12,21.3962631236951));
#15601=CARTESIAN_POINT('Ctrl Pts',(-9.68822499999973,0.298712821307165,
21.3842599369058));
#15602=CARTESIAN_POINT('Ctrl Pts',(-9.57054245632532,0.595858078272506,
21.3722567501165));
#15603=CARTESIAN_POINT('Ctrl Pts',(-9.3660158621486,0.813569405233517,21.3602535633272));
#15604=CARTESIAN_POINT('Ctrl Pts',(-9.16148926797188,1.03128073219453,21.3482503765379));
#15605=CARTESIAN_POINT('Ctrl Pts',(-8.87226522412737,1.16727314847171,21.3362471897485));
#15606=CARTESIAN_POINT('Ctrl Pts',(-8.57413435701338,1.18591009260197,21.3242440029592));
#15607=CARTESIAN_POINT('Ctrl Pts',(-8.27600348989939,1.20454703673223,21.3122408161699));
#15608=CARTESIAN_POINT('Ctrl Pts',(-7.97209482031988,1.10563290540059,21.3002376293806));
#15609=CARTESIAN_POINT('Ctrl Pts',(-7.74204705371974,0.915087963995849,
21.2882344425913));
#15610=CARTESIAN_POINT('Ctrl Pts',(-7.51199928711959,0.724543022591105,
21.276231255802));
#15611=CARTESIAN_POINT('Ctrl Pts',(-7.35822688079591,0.444367128060359,
21.2642280690126));
#15612=CARTESIAN_POINT('Ctrl Pts',(-7.32102560975803,0.14797985598914,21.2522248822233));
#15613=CARTESIAN_POINT('Ctrl Pts',(-7.28382433872014,-0.148407416082079,
21.240221695434));
#15614=CARTESIAN_POINT('Ctrl Pts',(-7.36358464744682,-0.457895344723092,
21.2282185086447));
#15615=CARTESIAN_POINT('Ctrl Pts',(-7.53940549437952,-0.699383189958662,
21.2162153218554));
#15616=CARTESIAN_POINT('Ctrl Pts',(-7.71522634131223,-0.940871035194232,
21.204212135066));
#15617=CARTESIAN_POINT('Ctrl Pts',(-7.98526240565897,-1.11182427083135,
21.1922089482767));
#15618=CARTESIAN_POINT('Ctrl Pts',(-8.27875123560237,-1.16744491727769,
21.1802057614874));
#15619=CARTESIAN_POINT('Ctrl Pts',(-8.57224006554577,-1.22306556372404,
21.1682025746981));
#15620=CARTESIAN_POINT('Ctrl Pts',(-8.88610136060063,-1.16276985666984,
21.1561993879088));
#15621=CARTESIAN_POINT('Ctrl Pts',(-9.138088348202,-1.00235817476282,21.1441962011195));
#15622=CARTESIAN_POINT('Ctrl Pts',(-9.39007533580337,-0.841946492855797,
21.1321930143301));
#15623=CARTESIAN_POINT('Ctrl Pts',(-9.57754329642199,-0.583102430601759,
21.1201898275408));
#15624=CARTESIAN_POINT('Ctrl Pts',(-9.65136659729223,-0.293655596344972,
21.1081866407515));
#15625=CARTESIAN_POINT('Ctrl Pts',(-9.67581103310561,-0.197813707971339,
21.104212135066));
#15626=CARTESIAN_POINT('Ctrl Pts',(-9.68822500000008,-0.0989100500913194,
21.1002376293806));
#15627=CARTESIAN_POINT('Ctrl Pts',(-9.688225,9.66893232146049E-13,21.0962631236951));
#15628=CARTESIAN_POINT('Ctrl Pts',(-9.688225,-7.50344231192912E-13,21.0537368763049));
#15629=CARTESIAN_POINT('Ctrl Pts',(-9.68822499999981,-0.298712821306855,
21.0657400630942));
#15630=CARTESIAN_POINT('Ctrl Pts',(-9.57054245632547,-0.595858078272227,
21.0777432498835));
#15631=CARTESIAN_POINT('Ctrl Pts',(-9.36601586214881,-0.813569405233291,
21.0897464366728));
#15632=CARTESIAN_POINT('Ctrl Pts',(-9.16148926797215,-1.03128073219435,
21.1017496234621));
#15633=CARTESIAN_POINT('Ctrl Pts',(-8.87226522412767,-1.16727314847161,
21.1137528102515));
#15634=CARTESIAN_POINT('Ctrl Pts',(-8.57413435701369,-1.18591009260195,
21.1257559970408));
#15635=CARTESIAN_POINT('Ctrl Pts',(-8.2760034898997,-1.20454703673229,21.1377591838301));
#15636=CARTESIAN_POINT('Ctrl Pts',(-7.97209482032017,-1.10563290540073,
21.1497623706194));
#15637=CARTESIAN_POINT('Ctrl Pts',(-7.74204705371998,-0.915087963996047,
21.1617655574087));
#15638=CARTESIAN_POINT('Ctrl Pts',(-7.51199928711978,-0.724543022591362,
21.1737687441981));
#15639=CARTESIAN_POINT('Ctrl Pts',(-7.35822688079602,-0.444367128060657,
21.1857719309874));
#15640=CARTESIAN_POINT('Ctrl Pts',(-7.32102560975807,-0.147979855989448,
21.1977751177767));
#15641=CARTESIAN_POINT('Ctrl Pts',(-7.28382433872011,0.148407416081762,
21.209778304566));
#15642=CARTESIAN_POINT('Ctrl Pts',(-7.3635846474467,0.457895344722796,21.2217814913553));
#15643=CARTESIAN_POINT('Ctrl Pts',(-7.53940549437934,0.699383189958411,
21.2337846781446));
#15644=CARTESIAN_POINT('Ctrl Pts',(-7.71522634131199,0.940871035194027,
21.245787864934));
#15645=CARTESIAN_POINT('Ctrl Pts',(-7.98526240565868,1.11182427083122,21.2577910517233));
#15646=CARTESIAN_POINT('Ctrl Pts',(-8.27875123560207,1.16744491727764,21.2697942385126));
#15647=CARTESIAN_POINT('Ctrl Pts',(-8.57224006554545,1.22306556372406,21.2817974253019));
#15648=CARTESIAN_POINT('Ctrl Pts',(-8.88610136060032,1.16276985666994,21.2938006120912));
#15649=CARTESIAN_POINT('Ctrl Pts',(-9.13808834820174,1.00235817476298,21.3058037988806));
#15650=CARTESIAN_POINT('Ctrl Pts',(-9.39007533580315,0.841946492856029,
21.3178069856699));
#15651=CARTESIAN_POINT('Ctrl Pts',(-9.57754329642184,0.583102430602039,
21.3298101724592));
#15652=CARTESIAN_POINT('Ctrl Pts',(-9.65136659729215,0.293655596345272,
21.3418133592485));
#15653=CARTESIAN_POINT('Ctrl Pts',(-9.67581103310556,0.197813707971646,
21.345787864934));
#15654=CARTESIAN_POINT('Ctrl Pts',(-9.68822500000005,0.0989100500916291,
21.3497623706194));
#15655=CARTESIAN_POINT('Ctrl Pts',(-9.688225,-6.5714100827563E-13,21.3537368763049));
#15656=CARTESIAN_POINT('Origin',(-8.5,0.,1.8));
#15657=CARTESIAN_POINT('',(-9.68941361091145,8.37946601863416E-5,21.6962631236951));
#15658=CARTESIAN_POINT('',(-9.688225,-6.9905192745523E-13,21.6537368763049));
#15659=CARTESIAN_POINT('',(-9.688225,-1.45515594291686E-16,1.8));
#15660=CARTESIAN_POINT('Ctrl Pts',(-9.688225,1.01829655818619E-12,21.6962631236951));
#15661=CARTESIAN_POINT('Ctrl Pts',(-9.68822499999975,0.298712821307101,
21.6842599369058));
#15662=CARTESIAN_POINT('Ctrl Pts',(-9.57054245632536,0.595858078272424,
21.6722567501165));
#15663=CARTESIAN_POINT('Ctrl Pts',(-9.36601586214868,0.813569405233437,
21.6602535633272));
#15664=CARTESIAN_POINT('Ctrl Pts',(-9.16148926797199,1.03128073219445,21.6482503765379));
#15665=CARTESIAN_POINT('Ctrl Pts',(-8.87226522412752,1.16727314847165,21.6362471897486));
#15666=CARTESIAN_POINT('Ctrl Pts',(-8.57413435701356,1.18591009260196,21.6242440029592));
#15667=CARTESIAN_POINT('Ctrl Pts',(-8.27600348989959,1.20454703673226,21.6122408161699));
#15668=CARTESIAN_POINT('Ctrl Pts',(-7.97209482032009,1.10563290540069,21.6002376293806));
#15669=CARTESIAN_POINT('Ctrl Pts',(-7.74204705371992,0.915087963996005,
21.5882344425913));
#15670=CARTESIAN_POINT('Ctrl Pts',(-7.51199928711976,0.724543022591323,
21.576231255802));
#15671=CARTESIAN_POINT('Ctrl Pts',(-7.35822688079602,0.444367128060637,
21.5642280690126));
#15672=CARTESIAN_POINT('Ctrl Pts',(-7.32102560975807,0.14797985598945,21.5522248822233));
#15673=CARTESIAN_POINT('Ctrl Pts',(-7.28382433872011,-0.148407416081737,
21.540221695434));
#15674=CARTESIAN_POINT('Ctrl Pts',(-7.36358464744668,-0.457895344722747,
21.5282185086447));
#15675=CARTESIAN_POINT('Ctrl Pts',(-7.5394054943793,-0.699383189958355,
21.5162153218554));
#15676=CARTESIAN_POINT('Ctrl Pts',(-7.71522634131192,-0.940871035193963,
21.5042121350661));
#15677=CARTESIAN_POINT('Ctrl Pts',(-7.98526240565858,-1.11182427083116,
21.4922089482767));
#15678=CARTESIAN_POINT('Ctrl Pts',(-8.27875123560193,-1.16744491727761,
21.4802057614874));
#15679=CARTESIAN_POINT('Ctrl Pts',(-8.57224006554528,-1.22306556372406,
21.4682025746981));
#15680=CARTESIAN_POINT('Ctrl Pts',(-8.88610136060014,-1.16276985666999,
21.4561993879088));
#15681=CARTESIAN_POINT('Ctrl Pts',(-9.13808834820156,-1.00235817476309,
21.4441962011195));
#15682=CARTESIAN_POINT('Ctrl Pts',(-9.39007533580298,-0.841946492856195,
21.4321930143302));
#15683=CARTESIAN_POINT('Ctrl Pts',(-9.57754329642171,-0.583102430602265,
21.4201898275408));
#15684=CARTESIAN_POINT('Ctrl Pts',(-9.65136659729208,-0.293655596345536,
21.4081866407515));
#15685=CARTESIAN_POINT('Ctrl Pts',(-9.67581103310557,-0.197813707971697,
21.4042121350661));
#15686=CARTESIAN_POINT('Ctrl Pts',(-9.68822500000009,-0.0989100500914515,
21.4002376293806));
#15687=CARTESIAN_POINT('Ctrl Pts',(-9.688225,1.0600409439121E-12,21.3962631236951));
#15688=CARTESIAN_POINT('Ctrl Pts',(-9.688225,-6.5714100827563E-13,21.3537368763049));
#15689=CARTESIAN_POINT('Ctrl Pts',(-9.68822499999983,-0.298712821306739,
21.3657400630942));
#15690=CARTESIAN_POINT('Ctrl Pts',(-9.57054245632554,-0.595858078272098,
21.3777432498835));
#15691=CARTESIAN_POINT('Ctrl Pts',(-9.36601586214892,-0.813569405233174,
21.3897464366728));
#15692=CARTESIAN_POINT('Ctrl Pts',(-9.1614892679723,-1.03128073219425,21.4017496234621));
#15693=CARTESIAN_POINT('Ctrl Pts',(-8.87226522412787,-1.16727314847154,
21.4137528102515));
#15694=CARTESIAN_POINT('Ctrl Pts',(-8.57413435701392,-1.18591009260194,
21.4257559970408));
#15695=CARTESIAN_POINT('Ctrl Pts',(-8.27600348989996,-1.20454703673233,
21.4377591838301));
#15696=CARTESIAN_POINT('Ctrl Pts',(-7.97209482032043,-1.10563290540085,
21.4497623706194));
#15697=CARTESIAN_POINT('Ctrl Pts',(-7.7420470537202,-0.915087963996235,
21.4617655574087));
#15698=CARTESIAN_POINT('Ctrl Pts',(-7.51199928711998,-0.724543022591623,
21.473768744198));
#15699=CARTESIAN_POINT('Ctrl Pts',(-7.35822688079616,-0.444367128060984,
21.4857719309874));
#15700=CARTESIAN_POINT('Ctrl Pts',(-7.32102560975811,-0.147979855989808,
21.4977751177767));
#15701=CARTESIAN_POINT('Ctrl Pts',(-7.28382433872006,0.148407416081368,
21.509778304566));
#15702=CARTESIAN_POINT('Ctrl Pts',(-7.36358464744655,0.457895344722402,
21.5217814913553));
#15703=CARTESIAN_POINT('Ctrl Pts',(-7.53940549437909,0.699383189958063,
21.5337846781446));
#15704=CARTESIAN_POINT('Ctrl Pts',(-7.71522634131163,0.940871035193724,
21.5457878649339));
#15705=CARTESIAN_POINT('Ctrl Pts',(-7.98526240565824,1.11182427083101,21.5577910517233));
#15706=CARTESIAN_POINT('Ctrl Pts',(-8.27875123560158,1.16744491727754,21.5697942385126));
#15707=CARTESIAN_POINT('Ctrl Pts',(-8.57224006554491,1.22306556372408,21.5817974253019));
#15708=CARTESIAN_POINT('Ctrl Pts',(-8.88610136059979,1.16276985667011,21.5938006120912));
#15709=CARTESIAN_POINT('Ctrl Pts',(-9.13808834820126,1.00235817476329,21.6058037988805));
#15710=CARTESIAN_POINT('Ctrl Pts',(-9.39007533580273,0.841946492856465,
21.6178069856699));
#15711=CARTESIAN_POINT('Ctrl Pts',(-9.57754329642153,0.583102430602592,
21.6298101724592));
#15712=CARTESIAN_POINT('Ctrl Pts',(-9.65136659729199,0.293655596345886,
21.6418133592485));
#15713=CARTESIAN_POINT('Ctrl Pts',(-9.67581103310551,0.197813707972055,
21.6457878649339));
#15714=CARTESIAN_POINT('Ctrl Pts',(-9.68822500000006,0.0989100500918124,
21.6497623706194));
#15715=CARTESIAN_POINT('Ctrl Pts',(-9.688225,-6.9905192745523E-13,21.6537368763049));
#15716=CARTESIAN_POINT('Origin',(-8.5,0.,1.8));
#15717=CARTESIAN_POINT('',(-9.68754848723268,0.00103932034338594,21.9962631236951));
#15718=CARTESIAN_POINT('',(-9.688225,-6.7346128673762E-13,21.9537368763049));
#15719=CARTESIAN_POINT('',(-9.688225,-1.45515594291686E-16,1.8));
#15720=CARTESIAN_POINT('Ctrl Pts',(-9.68754848723268,0.00103932034338594,
21.9962631236951));
#15721=CARTESIAN_POINT('Ctrl Pts',(-9.68846371561513,0.113646838372302,
21.9917421023245));
#15722=CARTESIAN_POINT('Ctrl Pts',(-9.67372334216155,0.22601158102592,21.9872210809538));
#15723=CARTESIAN_POINT('Ctrl Pts',(-9.64233633231695,0.333516176657786,
21.9827000595831));
#15724=CARTESIAN_POINT('Ctrl Pts',(-9.53190025330015,0.711774127212782,
21.9667927184315));
#15725=CARTESIAN_POINT('Ctrl Pts',(-9.21537813921845,1.02986326011492,21.9508853772799));
#15726=CARTESIAN_POINT('Ctrl Pts',(-8.83737688077721,1.14147606431245,21.9349780361283));
#15727=CARTESIAN_POINT('Ctrl Pts',(-8.45937562233595,1.25308886850999,21.9190706949767));
#15728=CARTESIAN_POINT('Ctrl Pts',(-8.01989521953514,1.15822534400289,21.903163353825));
#15729=CARTESIAN_POINT('Ctrl Pts',(-7.72189584988414,0.900773470014709,
21.8872560126734));
#15730=CARTESIAN_POINT('Ctrl Pts',(-7.42389648023317,0.643321596026557,
21.8713486715218));
#15731=CARTESIAN_POINT('Ctrl Pts',(-7.26737814373198,0.223281372557366,
21.8554413303702));
#15732=CARTESIAN_POINT('Ctrl Pts',(-7.32207205408808,-0.16726995791123,
21.8395339892186));
#15733=CARTESIAN_POINT('Ctrl Pts',(-7.34941900926613,-0.36254562314555,
21.8315803186428));
#15734=CARTESIAN_POINT('Ctrl Pts',(-7.42956902615852,-0.55044906512972,
21.823626648067));
#15735=CARTESIAN_POINT('Ctrl Pts',(-7.54824974241705,-0.70962405557879,
21.8156729774911));
#15736=CARTESIAN_POINT('Ctrl Pts',(-7.66693045867558,-0.86879904602786,
21.8077193069153));
#15737=CARTESIAN_POINT('Ctrl Pts',(-7.82414187430025,-0.999245584941831,
21.7997656363395));
#15738=CARTESIAN_POINT('Ctrl Pts',(-8.00348963778739,-1.08118959706215,
21.7918119657637));
#15739=CARTESIAN_POINT('Ctrl Pts',(-8.36218516476167,-1.24507762130277,
21.7759046246121));
#15740=CARTESIAN_POINT('Ctrl Pts',(-8.80942608318585,-1.21495553836879,
21.7599972834604));
#15741=CARTESIAN_POINT('Ctrl Pts',(-9.14122245772507,-1.00283232517649,
21.7440899423088));
#15742=CARTESIAN_POINT('Ctrl Pts',(-9.4730188322643,-0.790709111984192,
21.7281826011572));
#15743=CARTESIAN_POINT('Ctrl Pts',(-9.68937066291857,-0.396584768533572,
21.7122752600056));
#15744=CARTESIAN_POINT('Ctrl Pts',(-9.69028767880224,-0.00245087183618204,
21.696367918854));
#15745=CARTESIAN_POINT('Ctrl Pts',(-9.69028969252292,-0.00158537365915197,
21.6963329871344));
#15746=CARTESIAN_POINT('Ctrl Pts',(-9.69029066737497,-0.000719875436054535,
21.6962980554148));
#15747=CARTESIAN_POINT('Ctrl Pts',(-9.6902906044062,0.000145620923329259,
21.6962631236951));
#15748=CARTESIAN_POINT('Ctrl Pts',(-9.688225,-6.9905192745523E-13,21.6537368763049));
#15749=CARTESIAN_POINT('Ctrl Pts',(-9.68822499999982,-0.298712821306781,
21.6657400630942));
#15750=CARTESIAN_POINT('Ctrl Pts',(-9.57054245632552,-0.595858078272136,
21.6777432498835));
#15751=CARTESIAN_POINT('Ctrl Pts',(-9.36601586214889,-0.813569405233204,
21.6897464366728));
#15752=CARTESIAN_POINT('Ctrl Pts',(-9.16148926797227,-1.03128073219427,
21.7017496234621));
#15753=CARTESIAN_POINT('Ctrl Pts',(-8.87226522412783,-1.16727314847155,
21.7137528102515));
#15754=CARTESIAN_POINT('Ctrl Pts',(-8.57413435701387,-1.18591009260194,
21.7257559970408));
#15755=CARTESIAN_POINT('Ctrl Pts',(-8.27600348989992,-1.20454703673232,
21.7377591838301));
#15756=CARTESIAN_POINT('Ctrl Pts',(-7.97209482032039,-1.10563290540083,
21.7497623706194));
#15757=CARTESIAN_POINT('Ctrl Pts',(-7.74204705372017,-0.915087963996209,
21.7617655574087));
#15758=CARTESIAN_POINT('Ctrl Pts',(-7.51199928711995,-0.724543022591588,
21.773768744198));
#15759=CARTESIAN_POINT('Ctrl Pts',(-7.35822688079614,-0.444367128060944,
21.7857719309874));
#15760=CARTESIAN_POINT('Ctrl Pts',(-7.32102560975811,-0.147979855989767,
21.7977751177767));
#15761=CARTESIAN_POINT('Ctrl Pts',(-7.28382433872007,0.14840741608141,21.809778304566));
#15762=CARTESIAN_POINT('Ctrl Pts',(-7.36358464744656,0.457895344722442,
21.8217814913553));
#15763=CARTESIAN_POINT('Ctrl Pts',(-7.53940549437911,0.699383189958097,
21.8337846781446));
#15764=CARTESIAN_POINT('Ctrl Pts',(-7.71522634131166,0.940871035193752,
21.8457878649339));
#15765=CARTESIAN_POINT('Ctrl Pts',(-7.98526240565828,1.11182427083102,21.8577910517233));
#15766=CARTESIAN_POINT('Ctrl Pts',(-8.27875123560162,1.16744491727755,21.8697942385126));
#15767=CARTESIAN_POINT('Ctrl Pts',(-8.57224006554496,1.22306556372408,21.8817974253019));
#15768=CARTESIAN_POINT('Ctrl Pts',(-8.88610136059983,1.1627698566701,21.8938006120912));
#15769=CARTESIAN_POINT('Ctrl Pts',(-9.13808834820129,1.00235817476327,21.9058037988805));
#15770=CARTESIAN_POINT('Ctrl Pts',(-9.39007533580276,0.841946492856433,
21.9178069856699));
#15771=CARTESIAN_POINT('Ctrl Pts',(-9.57754329642156,0.583102430602554,
21.9298101724592));
#15772=CARTESIAN_POINT('Ctrl Pts',(-9.651366597292,0.293655596345845,21.9418133592485));
#15773=CARTESIAN_POINT('Ctrl Pts',(-9.67581103310551,0.197813707972057,
21.9457878649339));
#15774=CARTESIAN_POINT('Ctrl Pts',(-9.68822500000005,0.0989100500918605,
21.9497623706194));
#15775=CARTESIAN_POINT('Ctrl Pts',(-9.688225,-6.05904215689179E-13,21.9537368763049));
#15776=CARTESIAN_POINT('Origin',(-8.5,0.,1.8));
#15777=CARTESIAN_POINT('',(-9.6873844249699,-0.000213222977800639,22.2962631236951));
#15778=CARTESIAN_POINT('',(-9.688225,-6.47759623717548E-13,22.2537368763049));
#15779=CARTESIAN_POINT('',(-9.688225,-1.45515594291686E-16,1.8));
#15780=CARTESIAN_POINT('Ctrl Pts',(-9.68642524001508,-0.000456532936506715,
22.2962631236951));
#15781=CARTESIAN_POINT('Ctrl Pts',(-9.68575927361135,0.226185688933078,
22.2871861492342));
#15782=CARTESIAN_POINT('Ctrl Pts',(-9.62343522762896,0.453218610314175,
22.2781091747733));
#15783=CARTESIAN_POINT('Ctrl Pts',(-9.50198612166228,0.642506480183205,
22.2690322003123));
#15784=CARTESIAN_POINT('Ctrl Pts',(-9.28914732064055,0.974232291997172,
22.2531248591607));
#15785=CARTESIAN_POINT('Ctrl Pts',(-8.89472160162217,1.19003420325999,22.2372175180091));
#15786=CARTESIAN_POINT('Ctrl Pts',(-8.50091325276927,1.19031007669399,22.2213101768575));
#15787=CARTESIAN_POINT('Ctrl Pts',(-8.10710490391636,1.19058595012799,22.2054028357058));
#15788=CARTESIAN_POINT('Ctrl Pts',(-7.71391392522893,0.975335785733172,
22.1894954945542));
#15789=CARTESIAN_POINT('Ctrl Pts',(-7.49974687085622,0.644194972207926,
22.1735881534026));
#15790=CARTESIAN_POINT('Ctrl Pts',(-7.39266334366985,0.478624565445293,
22.1656344828268));
#15791=CARTESIAN_POINT('Ctrl Pts',(-7.33033579756217,0.28408149640005,22.157680812251));
#15792=CARTESIAN_POINT('Ctrl Pts',(-7.31594364125642,0.0860545895591625,
22.1497271416752));
#15793=CARTESIAN_POINT('Ctrl Pts',(-7.30155148495066,-0.111972317281703,
22.1417734710994));
#15794=CARTESIAN_POINT('Ctrl Pts',(-7.33509471844682,-0.313483061918211,
22.1338198005235));
#15795=CARTESIAN_POINT('Ctrl Pts',(-7.41711281973766,-0.492796955554075,
22.1258661299477));
#15796=CARTESIAN_POINT('Ctrl Pts',(-7.58114902231934,-0.851424742825822,
22.1099587887961));
#15797=CARTESIAN_POINT('Ctrl Pts',(-7.93908469607976,-1.12126512609498,
22.0940514476445));
#15798=CARTESIAN_POINT('Ctrl Pts',(-8.32879455452619,-1.17793361788769,
22.0781441064929));
#15799=CARTESIAN_POINT('Ctrl Pts',(-8.71850441297263,-1.2346021096804,22.0622367653413));
#15800=CARTESIAN_POINT('Ctrl Pts',(-9.13998845610508,-1.07809870999666,
22.0463294241896));
#15801=CARTESIAN_POINT('Ctrl Pts',(-9.39855545569536,-0.780633626050859,
22.030422083038));
#15802=CARTESIAN_POINT('Ctrl Pts',(-9.58363519429373,-0.567711017728565,
22.019035763257));
#15803=CARTESIAN_POINT('Ctrl Pts',(-9.68524345874889,-0.282565888500901,
22.0076494434761));
#15804=CARTESIAN_POINT('Ctrl Pts',(-9.68754848723268,0.00103932034338594,
21.9962631236951));
#15805=CARTESIAN_POINT('Ctrl Pts',(-9.688225,-6.05904215689179E-13,21.9537368763049));
#15806=CARTESIAN_POINT('Ctrl Pts',(-9.68822499999985,-0.298712821306711,
21.9657400630942));
#15807=CARTESIAN_POINT('Ctrl Pts',(-9.57054245632555,-0.595858078272097,
21.9777432498835));
#15808=CARTESIAN_POINT('Ctrl Pts',(-9.36601586214891,-0.813569405233185,
21.9897464366728));
#15809=CARTESIAN_POINT('Ctrl Pts',(-9.16148926797228,-1.03128073219427,
22.0017496234621));
#15810=CARTESIAN_POINT('Ctrl Pts',(-8.87226522412781,-1.16727314847157,
22.0137528102515));
#15811=CARTESIAN_POINT('Ctrl Pts',(-8.57413435701383,-1.18591009260194,
22.0257559970408));
#15812=CARTESIAN_POINT('Ctrl Pts',(-8.27600348989985,-1.20454703673232,
22.0377591838301));
#15813=CARTESIAN_POINT('Ctrl Pts',(-7.97209482032031,-1.10563290540079,
22.0497623706194));
#15814=CARTESIAN_POINT('Ctrl Pts',(-7.74204705372009,-0.915087963996139,
22.0617655574087));
#15815=CARTESIAN_POINT('Ctrl Pts',(-7.51199928711987,-0.724543022591483,
22.073768744198));
#15816=CARTESIAN_POINT('Ctrl Pts',(-7.35822688079608,-0.444367128060796,
22.0857719309874));
#15817=CARTESIAN_POINT('Ctrl Pts',(-7.32102560975808,-0.147979855989591,
22.0977751177767));
#15818=CARTESIAN_POINT('Ctrl Pts',(-7.28382433872009,0.148407416081614,
22.109778304566));
#15819=CARTESIAN_POINT('Ctrl Pts',(-7.36358464744664,0.457895344722657,
22.1217814913553));
#15820=CARTESIAN_POINT('Ctrl Pts',(-7.53940549437926,0.699383189958295,
22.1337846781446));
#15821=CARTESIAN_POINT('Ctrl Pts',(-7.71522634131187,0.940871035193932,
22.145787864934));
#15822=CARTESIAN_POINT('Ctrl Pts',(-7.98526240565855,1.11182427083115,22.1577910517233));
#15823=CARTESIAN_POINT('Ctrl Pts',(-8.27875123560192,1.16744491727761,22.1697942385126));
#15824=CARTESIAN_POINT('Ctrl Pts',(-8.5722400655453,1.22306556372406,22.1817974253019));
#15825=CARTESIAN_POINT('Ctrl Pts',(-8.88610136060018,1.16276985666999,22.1938006120912));
#15826=CARTESIAN_POINT('Ctrl Pts',(-9.13808834820161,1.00235817476306,22.2058037988805));
#15827=CARTESIAN_POINT('Ctrl Pts',(-9.39007533580305,0.841946492856137,
22.2178069856699));
#15828=CARTESIAN_POINT('Ctrl Pts',(-9.57754329642177,0.58310243060217,22.2298101724592));
#15829=CARTESIAN_POINT('Ctrl Pts',(-9.65136659729211,0.293655596345412,
22.2418133592485));
#15830=CARTESIAN_POINT('Ctrl Pts',(-9.67581103310554,0.197813707971767,
22.245787864934));
#15831=CARTESIAN_POINT('Ctrl Pts',(-9.68822500000005,0.0989100500917286,
22.2497623706194));
#15832=CARTESIAN_POINT('Ctrl Pts',(-9.688225,-5.80202552669107E-13,22.2537368763049));
#15833=CARTESIAN_POINT('Origin',(-8.5,0.,1.8));
#15834=CARTESIAN_POINT('',(-9.688225,1.09501296918779E-12,22.5962631236951));
#15835=CARTESIAN_POINT('',(-9.688225,-6.22168982999938E-13,22.5537368763049));
#15836=CARTESIAN_POINT('',(-9.688225,-1.45515594291686E-16,1.8));
#15837=CARTESIAN_POINT('Ctrl Pts',(-9.688225,1.16262555138746E-12,22.5962631236951));
#15838=CARTESIAN_POINT('Ctrl Pts',(-9.68822499999971,0.298712821307267,
22.5842599369058));
#15839=CARTESIAN_POINT('Ctrl Pts',(-9.57054245632527,0.595858078272598,
22.5722567501165));
#15840=CARTESIAN_POINT('Ctrl Pts',(-9.36601586214853,0.813569405233591,
22.5602535633272));
#15841=CARTESIAN_POINT('Ctrl Pts',(-9.16148926797179,1.03128073219458,22.5482503765379));
#15842=CARTESIAN_POINT('Ctrl Pts',(-8.87226522412727,1.16727314847174,22.5362471897485));
#15843=CARTESIAN_POINT('Ctrl Pts',(-8.57413435701328,1.18591009260198,22.5242440029592));
#15844=CARTESIAN_POINT('Ctrl Pts',(-8.27600348989929,1.20454703673221,22.5122408161699));
#15845=CARTESIAN_POINT('Ctrl Pts',(-7.97209482031979,1.10563290540055,22.5002376293806));
#15846=CARTESIAN_POINT('Ctrl Pts',(-7.74204705371966,0.915087963995784,
22.4882344425913));
#15847=CARTESIAN_POINT('Ctrl Pts',(-7.51199928711953,0.72454302259102,22.4762312558019));
#15848=CARTESIAN_POINT('Ctrl Pts',(-7.35822688079587,0.444367128060261,
22.4642280690126));
#15849=CARTESIAN_POINT('Ctrl Pts',(-7.32102560975801,0.147979855989039,
22.4522248822233));
#15850=CARTESIAN_POINT('Ctrl Pts',(-7.28382433872016,-0.148407416082184,
22.440221695434));
#15851=CARTESIAN_POINT('Ctrl Pts',(-7.36358464744686,-0.45789534472319,
22.4282185086447));
#15852=CARTESIAN_POINT('Ctrl Pts',(-7.53940549437958,-0.699383189958745,
22.4162153218554));
#15853=CARTESIAN_POINT('Ctrl Pts',(-7.71522634131231,-0.9408710351943,22.404212135066));
#15854=CARTESIAN_POINT('Ctrl Pts',(-7.98526240565907,-1.1118242708314,22.3922089482767));
#15855=CARTESIAN_POINT('Ctrl Pts',(-8.27875123560247,-1.16744491727771,
22.3802057614874));
#15856=CARTESIAN_POINT('Ctrl Pts',(-8.57224006554587,-1.22306556372403,
22.3682025746981));
#15857=CARTESIAN_POINT('Ctrl Pts',(-8.88610136060073,-1.16276985666981,
22.3561993879088));
#15858=CARTESIAN_POINT('Ctrl Pts',(-9.13808834820208,-1.00235817476276,
22.3441962011194));
#15859=CARTESIAN_POINT('Ctrl Pts',(-9.39007533580344,-0.84194649285572,
22.3321930143301));
#15860=CARTESIAN_POINT('Ctrl Pts',(-9.57754329642204,-0.583102430601666,
22.3201898275408));
#15861=CARTESIAN_POINT('Ctrl Pts',(-9.65136659729225,-0.293655596344872,
22.3081866407515));
#15862=CARTESIAN_POINT('Ctrl Pts',(-9.67581103310563,-0.197813707971238,
22.304212135066));
#15863=CARTESIAN_POINT('Ctrl Pts',(-9.68822500000009,-0.0989100500912168,
22.3002376293806));
#15864=CARTESIAN_POINT('Ctrl Pts',(-9.688225,1.06947783962141E-12,22.2962631236951));
#15865=CARTESIAN_POINT('Ctrl Pts',(-9.688225,-5.80202552669107E-13,22.2537368763049));
#15866=CARTESIAN_POINT('Ctrl Pts',(-9.68822499999985,-0.298712821306662,
22.2657400630942));
#15867=CARTESIAN_POINT('Ctrl Pts',(-9.57054245632558,-0.595858078272029,
22.2777432498835));
#15868=CARTESIAN_POINT('Ctrl Pts',(-9.36601586214897,-0.813569405233117,
22.2897464366728));
#15869=CARTESIAN_POINT('Ctrl Pts',(-9.16148926797237,-1.03128073219421,
22.3017496234621));
#15870=CARTESIAN_POINT('Ctrl Pts',(-8.87226522412795,-1.16727314847152,
22.3137528102515));
#15871=CARTESIAN_POINT('Ctrl Pts',(-8.57413435701399,-1.18591009260193,
22.3257559970408));
#15872=CARTESIAN_POINT('Ctrl Pts',(-8.27600348990004,-1.20454703673235,
22.3377591838301));
#15873=CARTESIAN_POINT('Ctrl Pts',(-7.9720948203205,-1.10563290540088,22.3497623706194));
#15874=CARTESIAN_POINT('Ctrl Pts',(-7.74204705372026,-0.915087963996284,
22.3617655574087));
#15875=CARTESIAN_POINT('Ctrl Pts',(-7.51199928712002,-0.724543022591687,
22.373768744198));
#15876=CARTESIAN_POINT('Ctrl Pts',(-7.35822688079619,-0.444367128061058,
22.3857719309874));
#15877=CARTESIAN_POINT('Ctrl Pts',(-7.32102560975812,-0.147979855989884,
22.3977751177767));
#15878=CARTESIAN_POINT('Ctrl Pts',(-7.28382433872005,0.148407416081289,
22.409778304566));
#15879=CARTESIAN_POINT('Ctrl Pts',(-7.36358464744652,0.457895344722328,
22.4217814913553));
#15880=CARTESIAN_POINT('Ctrl Pts',(-7.53940549437904,0.699383189958001,
22.4337846781446));
#15881=CARTESIAN_POINT('Ctrl Pts',(-7.71522634131157,0.940871035193674,
22.4457878649339));
#15882=CARTESIAN_POINT('Ctrl Pts',(-7.98526240565817,1.11182427083097,22.4577910517233));
#15883=CARTESIAN_POINT('Ctrl Pts',(-8.2787512356015,1.16744491727753,22.4697942385126));
#15884=CARTESIAN_POINT('Ctrl Pts',(-8.57224006554483,1.22306556372409,22.4817974253019));
#15885=CARTESIAN_POINT('Ctrl Pts',(-8.88610136059971,1.16276985667014,22.4938006120912));
#15886=CARTESIAN_POINT('Ctrl Pts',(-9.13808834820119,1.00235817476333,22.5058037988805));
#15887=CARTESIAN_POINT('Ctrl Pts',(-9.39007533580267,0.841946492856522,
22.5178069856698));
#15888=CARTESIAN_POINT('Ctrl Pts',(-9.5775432964215,0.583102430602662,22.5298101724592));
#15889=CARTESIAN_POINT('Ctrl Pts',(-9.65136659729197,0.29365559634596,22.5418133592485));
#15890=CARTESIAN_POINT('Ctrl Pts',(-9.67581103310549,0.197813707972153,
22.5457878649339));
#15891=CARTESIAN_POINT('Ctrl Pts',(-9.68822500000005,0.0989100500919342,
22.5497623706194));
#15892=CARTESIAN_POINT('Ctrl Pts',(-9.688225,-5.54667423102728E-13,22.5537368763049));
#15893=CARTESIAN_POINT('Origin',(-8.5,0.,1.8));
#15894=CARTESIAN_POINT('',(-9.688225,1.12065912105663E-12,22.8962631236951));
#15895=CARTESIAN_POINT('',(-9.688225,-5.96633853433559E-13,22.8537368763049));
#15896=CARTESIAN_POINT('',(-9.688225,-1.45515594291686E-16,1.8));
#15897=CARTESIAN_POINT('Ctrl Pts',(-9.688225,1.12065912105663E-12,22.8962631236951));
#15898=CARTESIAN_POINT('Ctrl Pts',(-9.68822499999972,0.298712821307135,
22.8842599369058));
#15899=CARTESIAN_POINT('Ctrl Pts',(-9.57054245632536,0.595858078272383,
22.8722567501165));
#15900=CARTESIAN_POINT('Ctrl Pts',(-9.36601586214874,0.813569405233364,
22.8602535633272));
#15901=CARTESIAN_POINT('Ctrl Pts',(-9.16148926797212,1.03128073219435,22.8482503765379));
#15902=CARTESIAN_POINT('Ctrl Pts',(-8.87226522412775,1.16727314847156,22.8362471897486));
#15903=CARTESIAN_POINT('Ctrl Pts',(-8.57413435701386,1.18591009260194,22.8242440029592));
#15904=CARTESIAN_POINT('Ctrl Pts',(-8.27600348989997,1.20454703673232,22.8122408161699));
#15905=CARTESIAN_POINT('Ctrl Pts',(-7.97209482032051,1.10563290540087,22.8002376293806));
#15906=CARTESIAN_POINT('Ctrl Pts',(-7.74204705372031,0.915087963996328,
22.7882344425913));
#15907=CARTESIAN_POINT('Ctrl Pts',(-7.51199928712012,0.724543022591786,
22.776231255802));
#15908=CARTESIAN_POINT('Ctrl Pts',(-7.35822688079628,0.44436712806125,22.7642280690127));
#15909=CARTESIAN_POINT('Ctrl Pts',(-7.32102560975815,0.147979855990152,
22.7522248822234));
#15910=CARTESIAN_POINT('Ctrl Pts',(-7.28382433872003,-0.148407416080945,
22.740221695434));
#15911=CARTESIAN_POINT('Ctrl Pts',(-7.36358464744637,-0.457895344721931,
22.7282185086447));
#15912=CARTESIAN_POINT('Ctrl Pts',(-7.53940549437876,-0.699383189957619,
22.7162153218554));
#15913=CARTESIAN_POINT('Ctrl Pts',(-7.71522634131116,-0.940871035193307,
22.7042121350661));
#15914=CARTESIAN_POINT('Ctrl Pts',(-7.9852624056576,-1.11182427083069,22.6922089482768));
#15915=CARTESIAN_POINT('Ctrl Pts',(-8.27875123560084,-1.1674449172774,22.6802057614875));
#15916=CARTESIAN_POINT('Ctrl Pts',(-8.57224006554407,-1.22306556372412,
22.6682025746982));
#15917=CARTESIAN_POINT('Ctrl Pts',(-8.88610136059891,-1.16276985667039,
22.6561993879088));
#15918=CARTESIAN_POINT('Ctrl Pts',(-9.13808834820045,-1.0023581747638,22.6441962011195));
#15919=CARTESIAN_POINT('Ctrl Pts',(-9.39007533580199,-0.841946492857216,
22.6321930143302));
#15920=CARTESIAN_POINT('Ctrl Pts',(-9.57754329642098,-0.583102430603576,
22.6201898275409));
#15921=CARTESIAN_POINT('Ctrl Pts',(-9.65136659729171,-0.293655596347007,
22.6081866407516));
#15922=CARTESIAN_POINT('Ctrl Pts',(-9.67581103310545,-0.197813707972676,
22.6042121350661));
#15923=CARTESIAN_POINT('Ctrl Pts',(-9.6882250000001,-0.0989100500918892,
22.6002376293806));
#15924=CARTESIAN_POINT('Ctrl Pts',(-9.688225,1.16262555138746E-12,22.5962631236951));
#15925=CARTESIAN_POINT('Ctrl Pts',(-9.688225,-5.54667423102728E-13,22.5537368763049));
#15926=CARTESIAN_POINT('Ctrl Pts',(-9.68822499999986,-0.298712821306682,
22.5657400630942));
#15927=CARTESIAN_POINT('Ctrl Pts',(-9.57054245632555,-0.595858078272095,
22.5777432498835));
#15928=CARTESIAN_POINT('Ctrl Pts',(-9.3660158621489,-0.813569405233197,
22.5897464366728));
#15929=CARTESIAN_POINT('Ctrl Pts',(-9.16148926797224,-1.0312807321943,22.6017496234621));
#15930=CARTESIAN_POINT('Ctrl Pts',(-8.87226522412775,-1.16727314847159,
22.6137528102515));
#15931=CARTESIAN_POINT('Ctrl Pts',(-8.57413435701375,-1.18591009260195,
22.6257559970408));
#15932=CARTESIAN_POINT('Ctrl Pts',(-8.27600348989974,-1.2045470367323,22.6377591838301));
#15933=CARTESIAN_POINT('Ctrl Pts',(-7.97209482032018,-1.10563290540074,
22.6497623706194));
#15934=CARTESIAN_POINT('Ctrl Pts',(-7.74204705371997,-0.915087963996042,
22.6617655574087));
#15935=CARTESIAN_POINT('Ctrl Pts',(-7.51199928711976,-0.724543022591342,
22.6737687441981));
#15936=CARTESIAN_POINT('Ctrl Pts',(-7.358226880796,-0.444367128060608,22.6857719309874));
#15937=CARTESIAN_POINT('Ctrl Pts',(-7.32102560975806,-0.147979855989374,
22.6977751177767));
#15938=CARTESIAN_POINT('Ctrl Pts',(-7.28382433872011,0.14840741608186,22.709778304566));
#15939=CARTESIAN_POINT('Ctrl Pts',(-7.36358464744674,0.457895344722913,
22.7217814913553));
#15940=CARTESIAN_POINT('Ctrl Pts',(-7.53940549437942,0.699383189958526,
22.7337846781447));
#15941=CARTESIAN_POINT('Ctrl Pts',(-7.71522634131211,0.940871035194139,
22.745787864934));
#15942=CARTESIAN_POINT('Ctrl Pts',(-7.98526240565886,1.1118242708313,22.7577910517233));
#15943=CARTESIAN_POINT('Ctrl Pts',(-8.27875123560227,1.16744491727768,22.7697942385126));
#15944=CARTESIAN_POINT('Ctrl Pts',(-8.57224006554569,1.22306556372405,22.7817974253019));
#15945=CARTESIAN_POINT('Ctrl Pts',(-8.88610136060057,1.16276985666986,22.7938006120912));
#15946=CARTESIAN_POINT('Ctrl Pts',(-9.13808834820197,1.00235817476284,22.8058037988806));
#15947=CARTESIAN_POINT('Ctrl Pts',(-9.39007533580336,0.841946492855809,
22.8178069856699));
#15948=CARTESIAN_POINT('Ctrl Pts',(-9.577543296422,0.583102430601749,22.8298101724592));
#15949=CARTESIAN_POINT('Ctrl Pts',(-9.65136659729223,0.293655596344938,
22.8418133592485));
#15950=CARTESIAN_POINT('Ctrl Pts',(-9.67581103310559,0.197813707971436,
22.845787864934));
#15951=CARTESIAN_POINT('Ctrl Pts',(-9.68822500000005,0.0989100500915545,
22.8497623706194));
#15952=CARTESIAN_POINT('Ctrl Pts',(-9.688225,-5.96633853433559E-13,22.8537368763049));
#15953=CARTESIAN_POINT('Origin',(-8.5,0.,1.8));
#15954=CARTESIAN_POINT('',(-9.688225,1.14630527292547E-12,23.1962631236951));
#15955=CARTESIAN_POINT('',(-9.688225,-5.70987701564718E-13,23.1537368763049));
#15956=CARTESIAN_POINT('',(-9.688225,-1.45515594291686E-16,1.8));
#15957=CARTESIAN_POINT('Ctrl Pts',(-9.688225,1.21391785512515E-12,23.1962631236951));
#15958=CARTESIAN_POINT('Ctrl Pts',(-9.6882249999997,0.298712821307319,23.1842599369058));
#15959=CARTESIAN_POINT('Ctrl Pts',(-9.57054245632524,0.595858078272645,
23.1722567501165));
#15960=CARTESIAN_POINT('Ctrl Pts',(-9.36601586214849,0.813569405233629,
23.1602535633272));
#15961=CARTESIAN_POINT('Ctrl Pts',(-9.16148926797175,1.03128073219461,23.1482503765379));
#15962=CARTESIAN_POINT('Ctrl Pts',(-8.87226522412722,1.16727314847176,23.1362471897485));
#15963=CARTESIAN_POINT('Ctrl Pts',(-8.57413435701323,1.18591009260198,23.1242440029592));
#15964=CARTESIAN_POINT('Ctrl Pts',(-8.27600348989924,1.2045470367322,23.1122408161699));
#15965=CARTESIAN_POINT('Ctrl Pts',(-7.97209482031974,1.10563290540052,23.1002376293806));
#15966=CARTESIAN_POINT('Ctrl Pts',(-7.74204705371962,0.915087963995751,
23.0882344425913));
#15967=CARTESIAN_POINT('Ctrl Pts',(-7.5119992871195,0.724543022590977,23.0762312558019));
#15968=CARTESIAN_POINT('Ctrl Pts',(-7.35822688079585,0.444367128060212,
23.0642280690126));
#15969=CARTESIAN_POINT('Ctrl Pts',(-7.32102560975801,0.147979855988988,
23.0522248822233));
#15970=CARTESIAN_POINT('Ctrl Pts',(-7.28382433872016,-0.148407416082236,
23.040221695434));
#15971=CARTESIAN_POINT('Ctrl Pts',(-7.36358464744688,-0.457895344723239,
23.0282185086447));
#15972=CARTESIAN_POINT('Ctrl Pts',(-7.53940549437961,-0.699383189958786,
23.0162153218554));
#15973=CARTESIAN_POINT('Ctrl Pts',(-7.71522634131235,-0.940871035194334,
23.004212135066));
#15974=CARTESIAN_POINT('Ctrl Pts',(-7.98526240565912,-1.11182427083142,
22.9922089482767));
#15975=CARTESIAN_POINT('Ctrl Pts',(-8.27875123560252,-1.16744491727772,
22.9802057614874));
#15976=CARTESIAN_POINT('Ctrl Pts',(-8.57224006554592,-1.22306556372403,
22.9682025746981));
#15977=CARTESIAN_POINT('Ctrl Pts',(-8.88610136060078,-1.16276985666979,
22.9561993879088));
#15978=CARTESIAN_POINT('Ctrl Pts',(-9.13808834820213,-1.00235817476274,
22.9441962011194));
#15979=CARTESIAN_POINT('Ctrl Pts',(-9.39007533580348,-0.841946492855682,
22.9321930143301));
#15980=CARTESIAN_POINT('Ctrl Pts',(-9.57754329642207,-0.583102430601619,
22.9201898275408));
#15981=CARTESIAN_POINT('Ctrl Pts',(-9.65136659729226,-0.293655596344823,
22.9081866407515));
#15982=CARTESIAN_POINT('Ctrl Pts',(-9.67581103310564,-0.197813707971187,
22.904212135066));
#15983=CARTESIAN_POINT('Ctrl Pts',(-9.6882250000001,-0.0989100500911656,
22.9002376293806));
#15984=CARTESIAN_POINT('Ctrl Pts',(-9.688225,1.12065912105663E-12,22.8962631236951));
#15985=CARTESIAN_POINT('Ctrl Pts',(-9.688225,-5.96633853433559E-13,22.8537368763049));
#15986=CARTESIAN_POINT('Ctrl Pts',(-9.68822499999985,-0.298712821306679,
22.8657400630942));
#15987=CARTESIAN_POINT('Ctrl Pts',(-9.57054245632557,-0.595858078272044,
22.8777432498835));
#15988=CARTESIAN_POINT('Ctrl Pts',(-9.36601586214896,-0.813569405233129,
22.8897464366728));
#15989=CARTESIAN_POINT('Ctrl Pts',(-9.16148926797235,-1.03128073219422,
22.9017496234621));
#15990=CARTESIAN_POINT('Ctrl Pts',(-8.87226522412793,-1.16727314847152,
22.9137528102515));
#15991=CARTESIAN_POINT('Ctrl Pts',(-8.57413435701398,-1.18591009260193,
22.9257559970408));
#15992=CARTESIAN_POINT('Ctrl Pts',(-8.27600348990002,-1.20454703673234,
22.9377591838301));
#15993=CARTESIAN_POINT('Ctrl Pts',(-7.97209482032048,-1.10563290540087,
22.9497623706194));
#15994=CARTESIAN_POINT('Ctrl Pts',(-7.74204705372025,-0.915087963996274,
22.9617655574087));
#15995=CARTESIAN_POINT('Ctrl Pts',(-7.51199928712001,-0.724543022591673,
22.973768744198));
#15996=CARTESIAN_POINT('Ctrl Pts',(-7.35822688079618,-0.444367128061042,
22.9857719309874));
#15997=CARTESIAN_POINT('Ctrl Pts',(-7.32102560975812,-0.147979855989868,
22.9977751177767));
#15998=CARTESIAN_POINT('Ctrl Pts',(-7.28382433872006,0.148407416081306,
23.009778304566));
#15999=CARTESIAN_POINT('Ctrl Pts',(-7.36358464744652,0.457895344722344,
23.0217814913553));
#16000=CARTESIAN_POINT('Ctrl Pts',(-7.53940549437905,0.699383189958014,
23.0337846781446));
#16001=CARTESIAN_POINT('Ctrl Pts',(-7.71522634131158,0.940871035193684,
23.0457878649339));
#16002=CARTESIAN_POINT('Ctrl Pts',(-7.98526240565818,1.11182427083098,23.0577910517233));
#16003=CARTESIAN_POINT('Ctrl Pts',(-8.27875123560152,1.16744491727753,23.0697942385126));
#16004=CARTESIAN_POINT('Ctrl Pts',(-8.57224006554485,1.22306556372409,23.0817974253019));
#16005=CARTESIAN_POINT('Ctrl Pts',(-8.88610136059973,1.16276985667013,23.0938006120912));
#16006=CARTESIAN_POINT('Ctrl Pts',(-9.13808834820121,1.00235817476332,23.1058037988805));
#16007=CARTESIAN_POINT('Ctrl Pts',(-9.39007533580268,0.84194649285651,23.1178069856698));
#16008=CARTESIAN_POINT('Ctrl Pts',(-9.57754329642151,0.583102430602647,
23.1298101724592));
#16009=CARTESIAN_POINT('Ctrl Pts',(-9.65136659729198,0.293655596345944,
23.1418133592485));
#16010=CARTESIAN_POINT('Ctrl Pts',(-9.67581103310549,0.19781370797218,23.1457878649339));
#16011=CARTESIAN_POINT('Ctrl Pts',(-9.68822500000003,0.098910050092008,
23.1497623706194));
#16012=CARTESIAN_POINT('Ctrl Pts',(-9.688225,-4.35929070619068E-13,23.1537368763049));
#16013=CARTESIAN_POINT('Origin',(-8.5,0.,1.8));
#16014=CARTESIAN_POINT('',(-9.688225,1.17184040249185E-12,23.4962631236951));
#16015=CARTESIAN_POINT('',(-9.688225,-5.45341549695877E-13,23.4537368763049));
#16016=CARTESIAN_POINT('',(-9.688225,-1.45515594291686E-16,1.8));
#16017=CARTESIAN_POINT('Ctrl Pts',(-9.688225,1.23945298469152E-12,23.4962631236951));
#16018=CARTESIAN_POINT('Ctrl Pts',(-9.68822499999969,0.298712821307322,
23.4842599369058));
#16019=CARTESIAN_POINT('Ctrl Pts',(-9.57054245632525,0.595858078272623,
23.4722567501165));
#16020=CARTESIAN_POINT('Ctrl Pts',(-9.36601586214852,0.813569405233598,
23.4602535633272));
#16021=CARTESIAN_POINT('Ctrl Pts',(-9.1614892679718,1.03128073219457,23.4482503765379));
#16022=CARTESIAN_POINT('Ctrl Pts',(-8.8722652241273,1.16727314847172,23.4362471897485));
#16023=CARTESIAN_POINT('Ctrl Pts',(-8.57413435701333,1.18591009260197,23.4242440029592));
#16024=CARTESIAN_POINT('Ctrl Pts',(-8.27600348989937,1.20454703673222,23.4122408161699));
#16025=CARTESIAN_POINT('Ctrl Pts',(-7.97209482031989,1.10563290540059,23.4002376293806));
#16026=CARTESIAN_POINT('Ctrl Pts',(-7.74204705371975,0.915087963995864,
23.3882344425913));
#16027=CARTESIAN_POINT('Ctrl Pts',(-7.51199928711962,0.724543022591139,
23.376231255802));
#16028=CARTESIAN_POINT('Ctrl Pts',(-7.35822688079594,0.444367128060424,
23.3642280690126));
#16029=CARTESIAN_POINT('Ctrl Pts',(-7.32102560975804,0.14797985598923,23.3522248822233));
#16030=CARTESIAN_POINT('Ctrl Pts',(-7.28382433872014,-0.148407416081964,
23.340221695434));
#16031=CARTESIAN_POINT('Ctrl Pts',(-7.36358464744677,-0.457895344722959,
23.3282185086447));
#16032=CARTESIAN_POINT('Ctrl Pts',(-7.53940549437943,-0.699383189958534,
23.3162153218554));
#16033=CARTESIAN_POINT('Ctrl Pts',(-7.71522634131209,-0.940871035194109,
23.304212135066));
#16034=CARTESIAN_POINT('Ctrl Pts',(-7.98526240565878,-1.11182427083126,
23.2922089482767));
#16035=CARTESIAN_POINT('Ctrl Pts',(-8.27875123560215,-1.16744491727765,
23.2802057614874));
#16036=CARTESIAN_POINT('Ctrl Pts',(-8.57224006554551,-1.22306556372405,
23.2682025746981));
#16037=CARTESIAN_POINT('Ctrl Pts',(-8.88610136060036,-1.16276985666992,
23.2561993879088));
#16038=CARTESIAN_POINT('Ctrl Pts',(-9.13808834820175,-1.00235817476298,
23.2441962011195));
#16039=CARTESIAN_POINT('Ctrl Pts',(-9.39007533580314,-0.841946492856029,
23.2321930143301));
#16040=CARTESIAN_POINT('Ctrl Pts',(-9.57754329642182,-0.583102430602064,
23.2201898275408));
#16041=CARTESIAN_POINT('Ctrl Pts',(-9.65136659729214,-0.293655596345322,
23.2081866407515));
#16042=CARTESIAN_POINT('Ctrl Pts',(-9.6758110331056,-0.1978137079715,23.2042121350661));
#16043=CARTESIAN_POINT('Ctrl Pts',(-9.6882250000001,-0.098910050091275,
23.2002376293806));
#16044=CARTESIAN_POINT('Ctrl Pts',(-9.688225,1.21391785512515E-12,23.1962631236951));
#16045=CARTESIAN_POINT('Ctrl Pts',(-9.688225,-4.35929070619068E-13,23.1537368763049));
#16046=CARTESIAN_POINT('Ctrl Pts',(-9.68822499999989,-0.298712821306496,
23.1657400630942));
#16047=CARTESIAN_POINT('Ctrl Pts',(-9.57054245632567,-0.595858078271855,
23.1777432498835));
#16048=CARTESIAN_POINT('Ctrl Pts',(-9.36601586214912,-0.813569405232963,
23.1897464366728));
#16049=CARTESIAN_POINT('Ctrl Pts',(-9.16148926797257,-1.03128073219407,
23.2017496234621));
#16050=CARTESIAN_POINT('Ctrl Pts',(-8.8722652241282,-1.16727314847143,23.2137528102514));
#16051=CARTESIAN_POINT('Ctrl Pts',(-8.57413435701427,-1.18591009260191,
23.2257559970408));
#16052=CARTESIAN_POINT('Ctrl Pts',(-8.27600348990034,-1.2045470367324,23.2377591838301));
#16053=CARTESIAN_POINT('Ctrl Pts',(-7.97209482032081,-1.10563290540102,
23.2497623706194));
#16054=CARTESIAN_POINT('Ctrl Pts',(-7.74204705372053,-0.915087963996506,
23.2617655574087));
#16055=CARTESIAN_POINT('Ctrl Pts',(-7.51199928712025,-0.72454302259199,
23.273768744198));
#16056=CARTESIAN_POINT('Ctrl Pts',(-7.35822688079634,-0.444367128061434,
23.2857719309873));
#16057=CARTESIAN_POINT('Ctrl Pts',(-7.32102560975817,-0.147979855990296,
23.2977751177767));
#16058=CARTESIAN_POINT('Ctrl Pts',(-7.28382433872001,0.148407416080842,
23.309778304566));
#16059=CARTESIAN_POINT('Ctrl Pts',(-7.36358464744634,0.457895344721885,
23.3217814913553));
#16060=CARTESIAN_POINT('Ctrl Pts',(-7.53940549437876,0.699383189957611,
23.3337846781446));
#16061=CARTESIAN_POINT('Ctrl Pts',(-7.71522634131117,0.940871035193337,
23.3457878649339));
#16062=CARTESIAN_POINT('Ctrl Pts',(-7.98526240565768,1.11182427083074,23.3577910517232));
#16063=CARTESIAN_POINT('Ctrl Pts',(-8.27875123560096,1.16744491727743,23.3697942385126));
#16064=CARTESIAN_POINT('Ctrl Pts',(-8.57224006554425,1.22306556372412,23.3817974253019));
#16065=CARTESIAN_POINT('Ctrl Pts',(-8.88610136059913,1.16276985667033,23.3938006120912));
#16066=CARTESIAN_POINT('Ctrl Pts',(-9.13808834820067,1.00235817476366,23.4058037988805));
#16067=CARTESIAN_POINT('Ctrl Pts',(-9.39007533580222,0.841946492856997,
23.4178069856698));
#16068=CARTESIAN_POINT('Ctrl Pts',(-9.57754329642117,0.583102430603261,
23.4298101724591));
#16069=CARTESIAN_POINT('Ctrl Pts',(-9.6513665972918,0.293655596346624,23.4418133592485));
#16070=CARTESIAN_POINT('Ctrl Pts',(-9.67581103310543,0.197813707972634,
23.4457878649339));
#16071=CARTESIAN_POINT('Ctrl Pts',(-9.68822500000004,0.0989100500922138,
23.4497623706194));
#16072=CARTESIAN_POINT('Ctrl Pts',(-9.688225,-4.77784478647436E-13,23.4537368763049));
#16073=CARTESIAN_POINT('Origin',(-8.5,0.,1.8));
#16074=CARTESIAN_POINT('',(-9.688225,1.19748655436069E-12,23.7962631236951));
#16075=CARTESIAN_POINT('',(-9.688225,-5.19806420129498E-13,23.7537368763049));
#16076=CARTESIAN_POINT('',(-9.688225,-1.45515594291686E-16,1.8));
#16077=CARTESIAN_POINT('Ctrl Pts',(-9.688225,1.33260069645758E-12,23.7962631236951));
#16078=CARTESIAN_POINT('Ctrl Pts',(-9.68822499999967,0.298712821307437,
23.7842599369058));
#16079=CARTESIAN_POINT('Ctrl Pts',(-9.57054245632518,0.595858078272752,
23.7722567501165));
#16080=CARTESIAN_POINT('Ctrl Pts',(-9.36601586214841,0.813569405233715,
23.7602535633272));
#16081=CARTESIAN_POINT('Ctrl Pts',(-9.16148926797164,1.03128073219468,23.7482503765379));
#16082=CARTESIAN_POINT('Ctrl Pts',(-8.8722652241271,1.16727314847179,23.7362471897485));
#16083=CARTESIAN_POINT('Ctrl Pts',(-8.57413435701311,1.18591009260199,23.7242440029592));
#16084=CARTESIAN_POINT('Ctrl Pts',(-8.27600348989911,1.20454703673218,23.7122408161699));
#16085=CARTESIAN_POINT('Ctrl Pts',(-7.97209482031963,1.10563290540047,23.7002376293806));
#16086=CARTESIAN_POINT('Ctrl Pts',(-7.74204705371953,0.915087963995675,
23.6882344425913));
#16087=CARTESIAN_POINT('Ctrl Pts',(-7.51199928711942,0.724543022590878,
23.6762312558019));
#16088=CARTESIAN_POINT('Ctrl Pts',(-7.35822688079581,0.444367128060098,
23.6642280690126));
#16089=CARTESIAN_POINT('Ctrl Pts',(-7.32102560975799,0.14797985598887,23.6522248822233));
#16090=CARTESIAN_POINT('Ctrl Pts',(-7.28382433872018,-0.148407416082358,
23.640221695434));
#16091=CARTESIAN_POINT('Ctrl Pts',(-7.36358464744692,-0.457895344723353,
23.6282185086447));
#16092=CARTESIAN_POINT('Ctrl Pts',(-7.53940549437968,-0.699383189958882,
23.6162153218553));
#16093=CARTESIAN_POINT('Ctrl Pts',(-7.71522634131245,-0.940871035194412,
23.604212135066));
#16094=CARTESIAN_POINT('Ctrl Pts',(-7.98526240565923,-1.11182427083147,
23.5922089482767));
#16095=CARTESIAN_POINT('Ctrl Pts',(-8.27875123560264,-1.16744491727775,
23.5802057614874));
#16096=CARTESIAN_POINT('Ctrl Pts',(-8.57224006554605,-1.22306556372402,
23.5682025746981));
#16097=CARTESIAN_POINT('Ctrl Pts',(-8.88610136060089,-1.16276985666975,
23.5561993879088));
#16098=CARTESIAN_POINT('Ctrl Pts',(-9.13808834820223,-1.00235817476267,
23.5441962011194));
#16099=CARTESIAN_POINT('Ctrl Pts',(-9.39007533580356,-0.841946492855593,
23.5321930143301));
#16100=CARTESIAN_POINT('Ctrl Pts',(-9.57754329642213,-0.583102430601512,
23.5201898275408));
#16101=CARTESIAN_POINT('Ctrl Pts',(-9.65136659729229,-0.293655596344708,
23.5081866407515));
#16102=CARTESIAN_POINT('Ctrl Pts',(-9.67581103310566,-0.19781370797107,
23.504212135066));
#16103=CARTESIAN_POINT('Ctrl Pts',(-9.6882250000001,-0.0989100500910468,
23.5002376293806));
#16104=CARTESIAN_POINT('Ctrl Pts',(-9.688225,1.23945298469152E-12,23.4962631236951));
#16105=CARTESIAN_POINT('Ctrl Pts',(-9.688225,-4.77784478647436E-13,23.4537368763049));
#16106=CARTESIAN_POINT('Ctrl Pts',(-9.68822499999988,-0.298712821306605,
23.4657400630942));
#16107=CARTESIAN_POINT('Ctrl Pts',(-9.57054245632559,-0.595858078272026,
23.4777432498835));
#16108=CARTESIAN_POINT('Ctrl Pts',(-9.36601586214895,-0.813569405233141,
23.4897464366728));
#16109=CARTESIAN_POINT('Ctrl Pts',(-9.16148926797231,-1.03128073219426,
23.5017496234621));
#16110=CARTESIAN_POINT('Ctrl Pts',(-8.87226522412783,-1.16727314847157,
23.5137528102515));
#16111=CARTESIAN_POINT('Ctrl Pts',(-8.57413435701383,-1.18591009260194,
23.5257559970408));
#16112=CARTESIAN_POINT('Ctrl Pts',(-8.27600348989982,-1.20454703673232,
23.5377591838301));
#16113=CARTESIAN_POINT('Ctrl Pts',(-7.97209482032025,-1.10563290540078,
23.5497623706194));
#16114=CARTESIAN_POINT('Ctrl Pts',(-7.74204705372003,-0.915087963996091,
23.5617655574087));
#16115=CARTESIAN_POINT('Ctrl Pts',(-7.5119992871198,-0.724543022591406,
23.5737687441981));
#16116=CARTESIAN_POINT('Ctrl Pts',(-7.35822688079603,-0.444367128060682,
23.5857719309874));
#16117=CARTESIAN_POINT('Ctrl Pts',(-7.32102560975807,-0.14797985598945,
23.5977751177767));
#16118=CARTESIAN_POINT('Ctrl Pts',(-7.2838243387201,0.148407416081782,23.609778304566));
#16119=CARTESIAN_POINT('Ctrl Pts',(-7.36358464744671,0.45789534472284,23.6217814913553));
#16120=CARTESIAN_POINT('Ctrl Pts',(-7.53940549437938,0.699383189958464,
23.6337846781447));
#16121=CARTESIAN_POINT('Ctrl Pts',(-7.71522634131205,0.940871035194088,
23.645787864934));
#16122=CARTESIAN_POINT('Ctrl Pts',(-7.98526240565879,1.11182427083127,23.6577910517233));
#16123=CARTESIAN_POINT('Ctrl Pts',(-8.2787512356022,1.16744491727766,23.6697942385126));
#16124=CARTESIAN_POINT('Ctrl Pts',(-8.57224006554561,1.22306556372405,23.6817974253019));
#16125=CARTESIAN_POINT('Ctrl Pts',(-8.8861013606005,1.16276985666989,23.6938006120912));
#16126=CARTESIAN_POINT('Ctrl Pts',(-9.1380883482019,1.00235817476288,23.7058037988806));
#16127=CARTESIAN_POINT('Ctrl Pts',(-9.39007533580331,0.841946492855867,
23.7178069856699));
#16128=CARTESIAN_POINT('Ctrl Pts',(-9.57754329642197,0.583102430601818,
23.7298101724592));
#16129=CARTESIAN_POINT('Ctrl Pts',(-9.65136659729222,0.293655596345012,
23.7418133592485));
#16130=CARTESIAN_POINT('Ctrl Pts',(-9.67581103310558,0.19781370797149,23.745787864934));
#16131=CARTESIAN_POINT('Ctrl Pts',(-9.68822500000005,0.0989100500915865,
23.7497623706194));
#16132=CARTESIAN_POINT('Ctrl Pts',(-9.688225,-5.87252468875477E-13,23.7537368763049));
#16133=CARTESIAN_POINT('Origin',(-8.5,0.,1.8));
#16134=CARTESIAN_POINT('',(-9.688225,1.223243728532E-12,24.0962631236951));
#16135=CARTESIAN_POINT('',(-9.688225,-4.94104757109426E-13,24.0537368763049));
#16136=CARTESIAN_POINT('',(-9.688225,-1.45515594291686E-16,1.8));
#16137=CARTESIAN_POINT('Ctrl Pts',(-9.688225,1.223243728532E-12,24.0962631236951));
#16138=CARTESIAN_POINT('Ctrl Pts',(-9.68822499999969,0.298712821307283,
24.0842599369058));
#16139=CARTESIAN_POINT('Ctrl Pts',(-9.57054245632528,0.595858078272564,
24.0722567501165));
#16140=CARTESIAN_POINT('Ctrl Pts',(-9.36601586214858,0.813569405233537,
24.0602535633272));
#16141=CARTESIAN_POINT('Ctrl Pts',(-9.16148926797189,1.03128073219451,24.0482503765379));
#16142=CARTESIAN_POINT('Ctrl Pts',(-8.87226522412743,1.16727314847168,24.0362471897486));
#16143=CARTESIAN_POINT('Ctrl Pts',(-8.57413435701348,1.18591009260196,24.0242440029592));
#16144=CARTESIAN_POINT('Ctrl Pts',(-8.27600348989954,1.20454703673225,24.0122408161699));
#16145=CARTESIAN_POINT('Ctrl Pts',(-7.97209482032007,1.10563290540067,24.0002376293806));
#16146=CARTESIAN_POINT('Ctrl Pts',(-7.74204705371992,0.915087963996004,
23.9882344425913));
#16147=CARTESIAN_POINT('Ctrl Pts',(-7.51199928711977,0.724543022591335,
23.976231255802));
#16148=CARTESIAN_POINT('Ctrl Pts',(-7.35822688079604,0.444367128060677,
23.9642280690127));
#16149=CARTESIAN_POINT('Ctrl Pts',(-7.32102560975807,0.147979855989515,
23.9522248822233));
#16150=CARTESIAN_POINT('Ctrl Pts',(-7.2838243387201,-0.148407416081648,
23.940221695434));
#16151=CARTESIAN_POINT('Ctrl Pts',(-7.36358464744665,-0.457895344722638,
23.9282185086447));
#16152=CARTESIAN_POINT('Ctrl Pts',(-7.53940549437922,-0.699383189958248,
23.9162153218554));
#16153=CARTESIAN_POINT('Ctrl Pts',(-7.7152263413118,-0.940871035193857,
23.9042121350661));
#16154=CARTESIAN_POINT('Ctrl Pts',(-7.98526240565841,-1.11182427083108,
23.8922089482768));
#16155=CARTESIAN_POINT('Ctrl Pts',(-8.27875123560173,-1.16744491727757,
23.8802057614874));
#16156=CARTESIAN_POINT('Ctrl Pts',(-8.57224006554505,-1.22306556372407,
23.8682025746981));
#16157=CARTESIAN_POINT('Ctrl Pts',(-8.8861013605999,-1.16276985667007,23.8561993879088));
#16158=CARTESIAN_POINT('Ctrl Pts',(-9.13808834820134,-1.00235817476324,
23.8441962011195));
#16159=CARTESIAN_POINT('Ctrl Pts',(-9.39007533580278,-0.841946492856407,
23.8321930143302));
#16160=CARTESIAN_POINT('Ctrl Pts',(-9.57754329642155,-0.583102430602547,
23.8201898275409));
#16161=CARTESIAN_POINT('Ctrl Pts',(-9.651366597292,-0.293655596345861,23.8081866407515));
#16162=CARTESIAN_POINT('Ctrl Pts',(-9.67581103310557,-0.197813707971833,
23.8042121350661));
#16163=CARTESIAN_POINT('Ctrl Pts',(-9.68822500000011,-0.0989100500913815,
23.8002376293806));
#16164=CARTESIAN_POINT('Ctrl Pts',(-9.688225,1.33260069645758E-12,23.7962631236951));
#16165=CARTESIAN_POINT('Ctrl Pts',(-9.688225,-5.87252468875477E-13,23.7537368763049));
#16166=CARTESIAN_POINT('Ctrl Pts',(-9.68822499999985,-0.298712821306647,
23.7657400630942));
#16167=CARTESIAN_POINT('Ctrl Pts',(-9.57054245632559,-0.595858078271991,
23.7777432498835));
#16168=CARTESIAN_POINT('Ctrl Pts',(-9.36601586214902,-0.813569405233074,
23.7897464366728));
#16169=CARTESIAN_POINT('Ctrl Pts',(-9.16148926797244,-1.03128073219416,
23.8017496234621));
#16170=CARTESIAN_POINT('Ctrl Pts',(-8.87226522412805,-1.16727314847148,
23.8137528102514));
#16171=CARTESIAN_POINT('Ctrl Pts',(-8.57413435701412,-1.18591009260192,
23.8257559970408));
#16172=CARTESIAN_POINT('Ctrl Pts',(-8.27600348990019,-1.20454703673237,
23.8377591838301));
#16173=CARTESIAN_POINT('Ctrl Pts',(-7.97209482032066,-1.10563290540095,
23.8497623706194));
#16174=CARTESIAN_POINT('Ctrl Pts',(-7.74204705372041,-0.915087963996409,
23.8617655574087));
#16175=CARTESIAN_POINT('Ctrl Pts',(-7.51199928712016,-0.724543022591864,
23.873768744198));
#16176=CARTESIAN_POINT('Ctrl Pts',(-7.35822688079628,-0.444367128061288,
23.8857719309873));
#16177=CARTESIAN_POINT('Ctrl Pts',(-7.32102560975815,-0.147979855990145,
23.8977751177767));
#16178=CARTESIAN_POINT('Ctrl Pts',(-7.28382433872002,0.148407416080997,
23.909778304566));
#16179=CARTESIAN_POINT('Ctrl Pts',(-7.3635846474464,0.45789534472203,23.9217814913553));
#16180=CARTESIAN_POINT('Ctrl Pts',(-7.53940549437885,0.699383189957734,
23.9337846781446));
#16181=CARTESIAN_POINT('Ctrl Pts',(-7.7152263413113,0.940871035193437,23.9457878649339));
#16182=CARTESIAN_POINT('Ctrl Pts',(-7.98526240565782,1.1118242708308,23.9577910517232));
#16183=CARTESIAN_POINT('Ctrl Pts',(-8.27875123560111,1.16744491727746,23.9697942385126));
#16184=CARTESIAN_POINT('Ctrl Pts',(-8.5722400655444,1.22306556372411,23.9817974253019));
#16185=CARTESIAN_POINT('Ctrl Pts',(-8.88610136059927,1.16276985667028,23.9938006120912));
#16186=CARTESIAN_POINT('Ctrl Pts',(-9.1380883482008,1.00235817476358,24.0058037988805));
#16187=CARTESIAN_POINT('Ctrl Pts',(-9.39007533580232,0.841946492856883,
24.0178069856698));
#16188=CARTESIAN_POINT('Ctrl Pts',(-9.57754329642124,0.583102430603124,
24.0298101724591));
#16189=CARTESIAN_POINT('Ctrl Pts',(-9.65136659729184,0.293655596346477,
24.0418133592485));
#16190=CARTESIAN_POINT('Ctrl Pts',(-9.67581103310544,0.197813707972528,
24.0457878649339));
#16191=CARTESIAN_POINT('Ctrl Pts',(-9.68822500000004,0.0989100500921524,
24.0497623706194));
#16192=CARTESIAN_POINT('Ctrl Pts',(-9.688225,-4.94104757109426E-13,24.0537368763049));
#16193=CARTESIAN_POINT('Origin',(-8.5,0.,1.8));
#16194=CARTESIAN_POINT('',(-9.688225,1.24877885809838E-12,24.3962631236951));
#16195=CARTESIAN_POINT('',(-9.688225,-4.68514116391816E-13,24.3537368763049));
#16196=CARTESIAN_POINT('',(-9.688225,-1.45515594291686E-16,1.8));
#16197=CARTESIAN_POINT('Ctrl Pts',(-9.688225,1.1811662758987E-12,24.3962631236951));
#16198=CARTESIAN_POINT('Ctrl Pts',(-9.6882249999997,0.298712821307263,24.3842599369058));
#16199=CARTESIAN_POINT('Ctrl Pts',(-9.57054245632528,0.595858078272571,
24.3722567501165));
#16200=CARTESIAN_POINT('Ctrl Pts',(-9.36601586214856,0.813569405233556,
24.3602535633272));
#16201=CARTESIAN_POINT('Ctrl Pts',(-9.16148926797185,1.03128073219454,24.3482503765379));
#16202=CARTESIAN_POINT('Ctrl Pts',(-8.87226522412736,1.16727314847171,24.3362471897485));
#16203=CARTESIAN_POINT('Ctrl Pts',(-8.57413435701339,1.18591009260197,24.3242440029592));
#16204=CARTESIAN_POINT('Ctrl Pts',(-8.27600348989943,1.20454703673223,24.3122408161699));
#16205=CARTESIAN_POINT('Ctrl Pts',(-7.97209482031994,1.10563290540062,24.3002376293806));
#16206=CARTESIAN_POINT('Ctrl Pts',(-7.7420470537198,0.915087963995901,24.2882344425913));
#16207=CARTESIAN_POINT('Ctrl Pts',(-7.51199928711966,0.724543022591188,
24.276231255802));
#16208=CARTESIAN_POINT('Ctrl Pts',(-7.35822688079596,0.44436712806048,24.2642280690126));
#16209=CARTESIAN_POINT('Ctrl Pts',(-7.32102560975804,0.147979855989288,
24.2522248822233));
#16210=CARTESIAN_POINT('Ctrl Pts',(-7.28382433872013,-0.148407416081904,
24.240221695434));
#16211=CARTESIAN_POINT('Ctrl Pts',(-7.36358464744675,-0.457895344722903,
24.2282185086447));
#16212=CARTESIAN_POINT('Ctrl Pts',(-7.5394054943794,-0.699383189958487,
24.2162153218554));
#16213=CARTESIAN_POINT('Ctrl Pts',(-7.71522634131205,-0.940871035194071,
24.2042121350661));
#16214=CARTESIAN_POINT('Ctrl Pts',(-7.98526240565873,-1.11182427083123,
24.1922089482767));
#16215=CARTESIAN_POINT('Ctrl Pts',(-8.27875123560209,-1.16744491727764,
24.1802057614874));
#16216=CARTESIAN_POINT('Ctrl Pts',(-8.57224006554545,-1.22306556372405,
24.1682025746981));
#16217=CARTESIAN_POINT('Ctrl Pts',(-8.8861013606003,-1.16276985666994,24.1561993879088));
#16218=CARTESIAN_POINT('Ctrl Pts',(-9.1380883482017,-1.00235817476301,24.1441962011195));
#16219=CARTESIAN_POINT('Ctrl Pts',(-9.3900753358031,-0.841946492856072,
24.1321930143301));
#16220=CARTESIAN_POINT('Ctrl Pts',(-9.57754329642179,-0.583102430602117,
24.1201898275408));
#16221=CARTESIAN_POINT('Ctrl Pts',(-9.65136659729212,-0.293655596345378,
24.1081866407515));
#16222=CARTESIAN_POINT('Ctrl Pts',(-9.6758110331056,-0.197813707971536,
24.1042121350661));
#16223=CARTESIAN_POINT('Ctrl Pts',(-9.6882250000001,-0.0989100500912883,
24.1002376293806));
#16224=CARTESIAN_POINT('Ctrl Pts',(-9.688225,1.223243728532E-12,24.0962631236951));
#16225=CARTESIAN_POINT('Ctrl Pts',(-9.688225,-4.94104757109426E-13,24.0537368763049));
#16226=CARTESIAN_POINT('Ctrl Pts',(-9.68822499999987,-0.298712821306554,
24.0657400630942));
#16227=CARTESIAN_POINT('Ctrl Pts',(-9.57054245632564,-0.595858078271907,
24.0777432498835));
#16228=CARTESIAN_POINT('Ctrl Pts',(-9.36601586214908,-0.813569405233006,
24.0897464366728));
#16229=CARTESIAN_POINT('Ctrl Pts',(-9.16148926797252,-1.0312807321941,24.1017496234621));
#16230=CARTESIAN_POINT('Ctrl Pts',(-8.87226522412814,-1.16727314847145,
24.1137528102514));
#16231=CARTESIAN_POINT('Ctrl Pts',(-8.57413435701421,-1.18591009260192,
24.1257559970408));
#16232=CARTESIAN_POINT('Ctrl Pts',(-8.27600348990028,-1.20454703673239,
24.1377591838301));
#16233=CARTESIAN_POINT('Ctrl Pts',(-7.97209482032075,-1.105632905401,24.1497623706194));
#16234=CARTESIAN_POINT('Ctrl Pts',(-7.74204705372048,-0.915087963996469,
24.1617655574087));
#16235=CARTESIAN_POINT('Ctrl Pts',(-7.51199928712022,-0.724543022591941,
24.173768744198));
#16236=CARTESIAN_POINT('Ctrl Pts',(-7.35822688079632,-0.444367128061378,
24.1857719309873));
#16237=CARTESIAN_POINT('Ctrl Pts',(-7.32102560975816,-0.147979855990238,
24.1977751177767));
#16238=CARTESIAN_POINT('Ctrl Pts',(-7.28382433872001,0.148407416080902,
24.209778304566));
#16239=CARTESIAN_POINT('Ctrl Pts',(-7.36358464744637,0.457895344721941,
24.2217814913553));
#16240=CARTESIAN_POINT('Ctrl Pts',(-7.53940549437879,0.699383189957658,
24.2337846781446));
#16241=CARTESIAN_POINT('Ctrl Pts',(-7.71522634131122,0.940871035193376,
24.2457878649339));
#16242=CARTESIAN_POINT('Ctrl Pts',(-7.98526240565773,1.11182427083076,24.2577910517232));
#16243=CARTESIAN_POINT('Ctrl Pts',(-8.27875123560102,1.16744491727744,24.2697942385126));
#16244=CARTESIAN_POINT('Ctrl Pts',(-8.5722400655443,1.22306556372411,24.2817974253019));
#16245=CARTESIAN_POINT('Ctrl Pts',(-8.88610136059918,1.16276985667031,24.2938006120912));
#16246=CARTESIAN_POINT('Ctrl Pts',(-9.13808834820072,1.00235817476363,24.3058037988805));
#16247=CARTESIAN_POINT('Ctrl Pts',(-9.39007533580226,0.841946492856953,
24.3178069856698));
#16248=CARTESIAN_POINT('Ctrl Pts',(-9.5775432964212,0.583102430603208,24.3298101724591));
#16249=CARTESIAN_POINT('Ctrl Pts',(-9.65136659729182,0.293655596346567,
24.3418133592485));
#16250=CARTESIAN_POINT('Ctrl Pts',(-9.67581103310543,0.197813707972598,
24.3457878649339));
#16251=CARTESIAN_POINT('Ctrl Pts',(-9.68822500000004,0.0989100500922005,
24.3497623706194));
#16252=CARTESIAN_POINT('Ctrl Pts',(-9.688225,-4.68514116391816E-13,24.3537368763049));
#16253=CARTESIAN_POINT('Origin',(-8.5,0.,1.8));
#16254=CARTESIAN_POINT('',(-9.688225,1.27431398766475E-12,24.6962631236951));
#16255=CARTESIAN_POINT('',(-9.688225,-4.42923475674206E-13,24.6537368763049));
#16256=CARTESIAN_POINT('',(-9.688225,-1.45515594291686E-16,1.8));
#16257=CARTESIAN_POINT('Ctrl Pts',(-9.688225,1.27431398766475E-12,24.6962631236951));
#16258=CARTESIAN_POINT('Ctrl Pts',(-9.68822499999968,0.298712821307379,
24.6842599369058));
#16259=CARTESIAN_POINT('Ctrl Pts',(-9.57054245632521,0.595858078272699,
24.6722567501165));
#16260=CARTESIAN_POINT('Ctrl Pts',(-9.36601586214845,0.813569405233673,
24.6602535633272));
#16261=CARTESIAN_POINT('Ctrl Pts',(-9.16148926797169,1.03128073219465,24.6482503765379));
#16262=CARTESIAN_POINT('Ctrl Pts',(-8.87226522412716,1.16727314847178,24.6362471897485));
#16263=CARTESIAN_POINT('Ctrl Pts',(-8.57413435701316,1.18591009260198,24.6242440029592));
#16264=CARTESIAN_POINT('Ctrl Pts',(-8.27600348989917,1.20454703673219,24.6122408161699));
#16265=CARTESIAN_POINT('Ctrl Pts',(-7.97209482031968,1.1056329054005,24.6002376293806));
#16266=CARTESIAN_POINT('Ctrl Pts',(-7.74204705371957,0.915087963995712,
24.5882344425913));
#16267=CARTESIAN_POINT('Ctrl Pts',(-7.51199928711946,0.724543022590927,
24.5762312558019));
#16268=CARTESIAN_POINT('Ctrl Pts',(-7.35822688079583,0.444367128060154,
24.5642280690126));
#16269=CARTESIAN_POINT('Ctrl Pts',(-7.321025609758,0.147979855988928,24.5522248822233));
#16270=CARTESIAN_POINT('Ctrl Pts',(-7.28382433872017,-0.148407416082298,
24.540221695434));
#16271=CARTESIAN_POINT('Ctrl Pts',(-7.3635846474469,-0.457895344723297,
24.5282185086447));
#16272=CARTESIAN_POINT('Ctrl Pts',(-7.53940549437965,-0.699383189958835,
24.5162153218554));
#16273=CARTESIAN_POINT('Ctrl Pts',(-7.7152263413124,-0.940871035194374,
24.504212135066));
#16274=CARTESIAN_POINT('Ctrl Pts',(-7.98526240565917,-1.11182427083144,
24.4922089482767));
#16275=CARTESIAN_POINT('Ctrl Pts',(-8.27875123560258,-1.16744491727773,
24.4802057614874));
#16276=CARTESIAN_POINT('Ctrl Pts',(-8.57224006554599,-1.22306556372402,
24.4682025746981));
#16277=CARTESIAN_POINT('Ctrl Pts',(-8.88610136060084,-1.16276985666977,
24.4561993879088));
#16278=CARTESIAN_POINT('Ctrl Pts',(-9.13808834820218,-1.0023581747627,24.4441962011194));
#16279=CARTESIAN_POINT('Ctrl Pts',(-9.39007533580352,-0.841946492855636,
24.4321930143301));
#16280=CARTESIAN_POINT('Ctrl Pts',(-9.5775432964221,-0.583102430601564,
24.4201898275408));
#16281=CARTESIAN_POINT('Ctrl Pts',(-9.65136659729228,-0.293655596344764,
24.4081866407515));
#16282=CARTESIAN_POINT('Ctrl Pts',(-9.67581103310565,-0.197813707971127,
24.404212135066));
#16283=CARTESIAN_POINT('Ctrl Pts',(-9.6882250000001,-0.0989100500911051,
24.4002376293806));
#16284=CARTESIAN_POINT('Ctrl Pts',(-9.688225,1.1811662758987E-12,24.3962631236951));
#16285=CARTESIAN_POINT('Ctrl Pts',(-9.688225,-4.68514116391816E-13,24.3537368763049));
#16286=CARTESIAN_POINT('Ctrl Pts',(-9.68822499999988,-0.298712821306551,
24.3657400630942));
#16287=CARTESIAN_POINT('Ctrl Pts',(-9.57054245632564,-0.595858078271928,
24.3777432498835));
#16288=CARTESIAN_POINT('Ctrl Pts',(-9.36601586214905,-0.813569405233036,
24.3897464366728));
#16289=CARTESIAN_POINT('Ctrl Pts',(-9.16148926797247,-1.03128073219414,
24.4017496234621));
#16290=CARTESIAN_POINT('Ctrl Pts',(-8.87226522412806,-1.16727314847148,
24.4137528102514));
#16291=CARTESIAN_POINT('Ctrl Pts',(-8.5741343570141,-1.18591009260192,24.4257559970408));
#16292=CARTESIAN_POINT('Ctrl Pts',(-8.27600348990015,-1.20454703673237,
24.4377591838301));
#16293=CARTESIAN_POINT('Ctrl Pts',(-7.97209482032061,-1.10563290540093,
24.4497623706194));
#16294=CARTESIAN_POINT('Ctrl Pts',(-7.74204705372035,-0.915087963996356,
24.4617655574087));
#16295=CARTESIAN_POINT('Ctrl Pts',(-7.51199928712009,-0.72454302259178,
24.473768744198));
#16296=CARTESIAN_POINT('Ctrl Pts',(-7.35822688079623,-0.444367128061165,
24.4857719309874));
#16297=CARTESIAN_POINT('Ctrl Pts',(-7.32102560975813,-0.147979855989995,
24.4977751177767));
#16298=CARTESIAN_POINT('Ctrl Pts',(-7.28382433872004,0.148407416081174,
24.509778304566));
#16299=CARTESIAN_POINT('Ctrl Pts',(-7.36358464744647,0.457895344722221,
24.5217814913553));
#16300=CARTESIAN_POINT('Ctrl Pts',(-7.53940549437898,0.699383189957911,
24.5337846781446));
#16301=CARTESIAN_POINT('Ctrl Pts',(-7.71522634131148,0.9408710351936,24.5457878649339));
#16302=CARTESIAN_POINT('Ctrl Pts',(-7.98526240565806,1.11182427083092,24.5577910517233));
#16303=CARTESIAN_POINT('Ctrl Pts',(-8.27875123560139,1.16744491727751,24.5697942385126));
#16304=CARTESIAN_POINT('Ctrl Pts',(-8.57224006554472,1.22306556372409,24.5817974253019));
#16305=CARTESIAN_POINT('Ctrl Pts',(-8.8861013605996,1.16276985667017,24.5938006120912));
#16306=CARTESIAN_POINT('Ctrl Pts',(-9.1380883482011,1.00235817476339,24.6058037988805));
#16307=CARTESIAN_POINT('Ctrl Pts',(-9.39007533580259,0.841946492856606,
24.6178069856698));
#16308=CARTESIAN_POINT('Ctrl Pts',(-9.57754329642144,0.583102430602763,
24.6298101724592));
#16309=CARTESIAN_POINT('Ctrl Pts',(-9.65136659729195,0.293655596346069,
24.6418133592485));
#16310=CARTESIAN_POINT('Ctrl Pts',(-9.67581103310547,0.197813707972285,
24.6457878649339));
#16311=CARTESIAN_POINT('Ctrl Pts',(-9.68822500000003,0.0989100500920911,
24.6497623706194));
#16312=CARTESIAN_POINT('Ctrl Pts',(-9.688225,-3.75310893474534E-13,24.6537368763049));
#16313=CARTESIAN_POINT('Origin',(-8.5,0.,1.8));
#16314=CARTESIAN_POINT('',(-9.68868882774917,0.000480291784193624,24.9962631236951));
#16315=CARTESIAN_POINT('',(-9.688225,-4.17277323805365E-13,24.9537368763049));
#16316=CARTESIAN_POINT('',(-9.688225,-1.45515594291686E-16,1.8));
#16317=CARTESIAN_POINT('Ctrl Pts',(-9.688225,1.2999601395336E-12,24.9962631236951));
#16318=CARTESIAN_POINT('Ctrl Pts',(-9.68822499999967,0.298712821307405,
24.9842599369058));
#16319=CARTESIAN_POINT('Ctrl Pts',(-9.5705424563252,0.595858078272722,24.9722567501165));
#16320=CARTESIAN_POINT('Ctrl Pts',(-9.36601586214844,0.813569405233692,
24.9602535633272));
#16321=CARTESIAN_POINT('Ctrl Pts',(-9.16148926797167,1.03128073219466,24.9482503765379));
#16322=CARTESIAN_POINT('Ctrl Pts',(-8.87226522412713,1.16727314847178,24.9362471897485));
#16323=CARTESIAN_POINT('Ctrl Pts',(-8.57413435701314,1.18591009260199,24.9242440029592));
#16324=CARTESIAN_POINT('Ctrl Pts',(-8.27600348989915,1.20454703673219,24.9122408161699));
#16325=CARTESIAN_POINT('Ctrl Pts',(-7.97209482031966,1.10563290540049,24.9002376293806));
#16326=CARTESIAN_POINT('Ctrl Pts',(-7.74204705371955,0.915087963995696,
24.8882344425913));
#16327=CARTESIAN_POINT('Ctrl Pts',(-7.51199928711944,0.724543022590906,
24.8762312558019));
#16328=CARTESIAN_POINT('Ctrl Pts',(-7.35822688079582,0.444367128060129,
24.8642280690126));
#16329=CARTESIAN_POINT('Ctrl Pts',(-7.321025609758,0.147979855988902,24.8522248822233));
#16330=CARTESIAN_POINT('Ctrl Pts',(-7.28382433872017,-0.148407416082324,
24.840221695434));
#16331=CARTESIAN_POINT('Ctrl Pts',(-7.36358464744691,-0.457895344723321,
24.8282185086447));
#16332=CARTESIAN_POINT('Ctrl Pts',(-7.53940549437966,-0.699383189958856,
24.8162153218554));
#16333=CARTESIAN_POINT('Ctrl Pts',(-7.71522634131242,-0.940871035194391,
24.804212135066));
#16334=CARTESIAN_POINT('Ctrl Pts',(-7.9852624056592,-1.11182427083146,24.7922089482767));
#16335=CARTESIAN_POINT('Ctrl Pts',(-8.27875123560261,-1.16744491727774,
24.7802057614874));
#16336=CARTESIAN_POINT('Ctrl Pts',(-8.57224006554601,-1.22306556372402,
24.7682025746981));
#16337=CARTESIAN_POINT('Ctrl Pts',(-8.88610136060086,-1.16276985666976,
24.7561993879088));
#16338=CARTESIAN_POINT('Ctrl Pts',(-9.1380883482022,-1.00235817476269,24.7441962011194));
#16339=CARTESIAN_POINT('Ctrl Pts',(-9.39007533580354,-0.841946492855617,
24.7321930143301));
#16340=CARTESIAN_POINT('Ctrl Pts',(-9.57754329642211,-0.583102430601541,
24.7201898275408));
#16341=CARTESIAN_POINT('Ctrl Pts',(-9.65136659729229,-0.293655596344739,
24.7081866407515));
#16342=CARTESIAN_POINT('Ctrl Pts',(-9.67581103310566,-0.19781370797108,
24.704212135066));
#16343=CARTESIAN_POINT('Ctrl Pts',(-9.68822500000011,-0.0989100500910345,
24.7002376293806));
#16344=CARTESIAN_POINT('Ctrl Pts',(-9.688225,1.27431398766475E-12,24.6962631236951));
#16345=CARTESIAN_POINT('Ctrl Pts',(-9.688225,-3.75310893474534E-13,24.6537368763049));
#16346=CARTESIAN_POINT('Ctrl Pts',(-9.68822499999991,-0.298712821306457,
24.6657400630942));
#16347=CARTESIAN_POINT('Ctrl Pts',(-9.57054245632568,-0.595858078271845,
24.6777432498835));
#16348=CARTESIAN_POINT('Ctrl Pts',(-9.36601586214912,-0.813569405232968,
24.6897464366728));
#16349=CARTESIAN_POINT('Ctrl Pts',(-9.16148926797255,-1.03128073219409,
24.7017496234621));
#16350=CARTESIAN_POINT('Ctrl Pts',(-8.87226522412815,-1.16727314847145,
24.7137528102514));
#16351=CARTESIAN_POINT('Ctrl Pts',(-8.5741343570142,-1.18591009260192,24.7257559970408));
#16352=CARTESIAN_POINT('Ctrl Pts',(-8.27600348990024,-1.20454703673238,
24.7377591838301));
#16353=CARTESIAN_POINT('Ctrl Pts',(-7.97209482032069,-1.10563290540097,
24.7497623706194));
#16354=CARTESIAN_POINT('Ctrl Pts',(-7.74204705372042,-0.915087963996415,
24.7617655574087));
#16355=CARTESIAN_POINT('Ctrl Pts',(-7.51199928712015,-0.724543022591857,
24.773768744198));
#16356=CARTESIAN_POINT('Ctrl Pts',(-7.35822688079626,-0.444367128061255,
24.7857719309873));
#16357=CARTESIAN_POINT('Ctrl Pts',(-7.32102560975814,-0.147979855990088,
24.7977751177767));
#16358=CARTESIAN_POINT('Ctrl Pts',(-7.28382433872003,0.148407416081079,
24.809778304566));
#16359=CARTESIAN_POINT('Ctrl Pts',(-7.36358464744644,0.457895344722132,
24.8217814913553));
#16360=CARTESIAN_POINT('Ctrl Pts',(-7.53940549437892,0.699383189957835,
24.8337846781446));
#16361=CARTESIAN_POINT('Ctrl Pts',(-7.71522634131141,0.940871035193538,
24.8457878649339));
#16362=CARTESIAN_POINT('Ctrl Pts',(-7.98526240565798,1.11182427083088,24.8577910517233));
#16363=CARTESIAN_POINT('Ctrl Pts',(-8.2787512356013,1.16744491727749,24.8697942385126));
#16364=CARTESIAN_POINT('Ctrl Pts',(-8.57224006554462,1.2230655637241,24.8817974253019));
#16365=CARTESIAN_POINT('Ctrl Pts',(-8.88610136059951,1.1627698566702,24.8938006120912));
#16366=CARTESIAN_POINT('Ctrl Pts',(-9.13808834820102,1.00235817476344,24.9058037988805));
#16367=CARTESIAN_POINT('Ctrl Pts',(-9.39007533580253,0.841946492856676,
24.9178069856698));
#16368=CARTESIAN_POINT('Ctrl Pts',(-9.5775432964214,0.583102430602848,24.9298101724592));
#16369=CARTESIAN_POINT('Ctrl Pts',(-9.65136659729192,0.293655596346159,
24.9418133592485));
#16370=CARTESIAN_POINT('Ctrl Pts',(-9.67581103310546,0.197813707972355,
24.9457878649339));
#16371=CARTESIAN_POINT('Ctrl Pts',(-9.68822500000003,0.0989100500921392,
24.9497623706194));
#16372=CARTESIAN_POINT('Ctrl Pts',(-9.688225,-3.49664741605693E-13,24.9537368763049));
#16373=CARTESIAN_POINT('Origin',(-8.5,0.,1.8));
#16374=CARTESIAN_POINT('',(-9.6871905929363,0.000217402971942964,25.2962631236951));
#16375=CARTESIAN_POINT('',(-9.688225,-3.91631171936524E-13,25.2537368763049));
#16376=CARTESIAN_POINT('',(-9.688225,-1.45515594291686E-16,1.8));
#16377=CARTESIAN_POINT('Ctrl Pts',(-9.68646993064437,0.000368865704102106,
25.2962631236951));
#16378=CARTESIAN_POINT('Ctrl Pts',(-9.68708439251358,0.173016958435834,
25.2893486417863));
#16379=CARTESIAN_POINT('Ctrl Pts',(-9.65191323401855,0.345465200581628,
25.2824341598775));
#16380=CARTESIAN_POINT('Ctrl Pts',(-9.5797823988822,0.500859996551334,25.2755196779686));
#16381=CARTESIAN_POINT('Ctrl Pts',(-9.41383940890919,0.858358658818528,
25.259612336817));
#16382=CARTESIAN_POINT('Ctrl Pts',(-9.05228055867788,1.12559883272073,25.2437049956654));
#16383=CARTESIAN_POINT('Ctrl Pts',(-8.66213915242611,1.17921575971508,25.2277976545138));
#16384=CARTESIAN_POINT('Ctrl Pts',(-8.2719977461744,1.23283268670942,25.2118903133621));
#16385=CARTESIAN_POINT('Ctrl Pts',(-7.85327378390223,1.07282636679594,25.1959829722105));
#16386=CARTESIAN_POINT('Ctrl Pts',(-7.59622570194734,0.773747699679508,
25.1800756310589));
#16387=CARTESIAN_POINT('Ctrl Pts',(-7.46770166096987,0.624208366121258,
25.1721219604831));
#16388=CARTESIAN_POINT('Ctrl Pts',(-7.37959659007174,0.439900945762252,
25.1641682899073));
#16389=CARTESIAN_POINT('Ctrl Pts',(-7.3385132018884,0.245648673673906,25.1562146193315));
#16390=CARTESIAN_POINT('Ctrl Pts',(-7.29742981370506,0.0513964015856042,
25.1482609487557));
#16391=CARTESIAN_POINT('Ctrl Pts',(-7.3033681082365,-0.152800722232033,
25.1403072781799));
#16392=CARTESIAN_POINT('Ctrl Pts',(-7.36034118769235,-0.34157177299863,
25.1323536076041));
#16393=CARTESIAN_POINT('Ctrl Pts',(-7.47428734660405,-0.719113874531823,
25.1164462664524));
#16394=CARTESIAN_POINT('Ctrl Pts',(-7.7923726452134,-1.03495168386085,25.1005389253008));
#16395=CARTESIAN_POINT('Ctrl Pts',(-8.1708146320899,-1.1438863170192,25.0846315841492));
#16396=CARTESIAN_POINT('Ctrl Pts',(-8.54925661896646,-1.25282095017757,
25.0687242429976));
#16397=CARTESIAN_POINT('Ctrl Pts',(-8.98805529411019,-1.1548524071652,25.052816901846));
#16398=CARTESIAN_POINT('Ctrl Pts',(-9.28453253432374,-0.895153320760619,
25.0369095606943));
#16399=CARTESIAN_POINT('Ctrl Pts',(-9.53705207548348,-0.673958958281899,
25.0233607483613));
#16400=CARTESIAN_POINT('Ctrl Pts',(-9.68632458412737,-0.335437232707008,
25.0098119360282));
#16401=CARTESIAN_POINT('Ctrl Pts',(-9.68908827253991,0.000893915270617441,
24.9962631236951));
#16402=CARTESIAN_POINT('Ctrl Pts',(-9.688225,-3.49664741605693E-13,24.9537368763049));
#16403=CARTESIAN_POINT('Ctrl Pts',(-9.68822499999991,-0.298712821306432,
24.9657400630942));
#16404=CARTESIAN_POINT('Ctrl Pts',(-9.57054245632569,-0.595858078271821,
24.9777432498835));
#16405=CARTESIAN_POINT('Ctrl Pts',(-9.36601586214913,-0.81356940523295,
24.9897464366728));
#16406=CARTESIAN_POINT('Ctrl Pts',(-9.16148926797257,-1.03128073219408,
25.0017496234621));
#16407=CARTESIAN_POINT('Ctrl Pts',(-8.87226522412817,-1.16727314847144,
25.0137528102514));
#16408=CARTESIAN_POINT('Ctrl Pts',(-8.57413435701422,-1.18591009260192,
25.0257559970408));
#16409=CARTESIAN_POINT('Ctrl Pts',(-8.27600348990027,-1.20454703673239,
25.0377591838301));
#16410=CARTESIAN_POINT('Ctrl Pts',(-7.97209482032071,-1.10563290540098,
25.0497623706194));
#16411=CARTESIAN_POINT('Ctrl Pts',(-7.74204705372044,-0.915087963996431,
25.0617655574087));
#16412=CARTESIAN_POINT('Ctrl Pts',(-7.51199928712016,-0.724543022591879,
25.073768744198));
#16413=CARTESIAN_POINT('Ctrl Pts',(-7.35822688079627,-0.444367128061279,
25.0857719309873));
#16414=CARTESIAN_POINT('Ctrl Pts',(-7.32102560975815,-0.147979855990113,
25.0977751177767));
#16415=CARTESIAN_POINT('Ctrl Pts',(-7.28382433872002,0.148407416081053,
25.109778304566));
#16416=CARTESIAN_POINT('Ctrl Pts',(-7.36358464744643,0.457895344722108,
25.1217814913553));
#16417=CARTESIAN_POINT('Ctrl Pts',(-7.53940549437891,0.699383189957815,
25.1337846781446));
#16418=CARTESIAN_POINT('Ctrl Pts',(-7.71522634131139,0.940871035193521,
25.1457878649339));
#16419=CARTESIAN_POINT('Ctrl Pts',(-7.98526240565795,1.11182427083087,25.1577910517233));
#16420=CARTESIAN_POINT('Ctrl Pts',(-8.27875123560127,1.16744491727749,25.1697942385126));
#16421=CARTESIAN_POINT('Ctrl Pts',(-8.57224006554459,1.2230655637241,25.1817974253019));
#16422=CARTESIAN_POINT('Ctrl Pts',(-8.88610136059949,1.16276985667021,25.1938006120912));
#16423=CARTESIAN_POINT('Ctrl Pts',(-9.138088348201,1.00235817476345,25.2058037988805));
#16424=CARTESIAN_POINT('Ctrl Pts',(-9.39007533580251,0.841946492856695,
25.2178069856698));
#16425=CARTESIAN_POINT('Ctrl Pts',(-9.57754329642138,0.583102430602871,
25.2298101724592));
#16426=CARTESIAN_POINT('Ctrl Pts',(-9.65136659729192,0.293655596346184,
25.2418133592485));
#16427=CARTESIAN_POINT('Ctrl Pts',(-9.67581103310546,0.197813707972359,
25.2457878649339));
#16428=CARTESIAN_POINT('Ctrl Pts',(-9.68822500000003,0.0989100500921199,
25.2497623706194));
#16429=CARTESIAN_POINT('Ctrl Pts',(-9.688225,-3.91631171936524E-13,25.2537368763049));
#16430=CARTESIAN_POINT('Origin',(-8.5,0.,1.8));
#16431=CARTESIAN_POINT('',(-9.688225,1.35125244327128E-12,25.5962631236951));
#16432=CARTESIAN_POINT('',(-9.688225,-3.66040531218914E-13,25.5537368763049));
#16433=CARTESIAN_POINT('',(-9.688225,-1.45515594291686E-16,1.8));
#16434=CARTESIAN_POINT('Ctrl Pts',(-9.688225,1.41875400316849E-12,25.5962631236951));
#16435=CARTESIAN_POINT('Ctrl Pts',(-9.68822499999964,0.298712821307546,
25.5842599369058));
#16436=CARTESIAN_POINT('Ctrl Pts',(-9.57054245632512,0.595858078272874,
25.5722567501165));
#16437=CARTESIAN_POINT('Ctrl Pts',(-9.36601586214831,0.813569405233827,
25.5602535633272));
#16438=CARTESIAN_POINT('Ctrl Pts',(-9.16148926797149,1.03128073219478,25.5482503765378));
#16439=CARTESIAN_POINT('Ctrl Pts',(-8.8722652241269,1.16727314847186,25.5362471897485));
#16440=CARTESIAN_POINT('Ctrl Pts',(-8.57413435701289,1.185910092602,25.5242440029592));
#16441=CARTESIAN_POINT('Ctrl Pts',(-8.27600348989887,1.20454703673214,25.5122408161699));
#16442=CARTESIAN_POINT('Ctrl Pts',(-7.97209482031938,1.10563290540036,25.5002376293806));
#16443=CARTESIAN_POINT('Ctrl Pts',(-7.7420470537193,0.915087963995491,25.4882344425912));
#16444=CARTESIAN_POINT('Ctrl Pts',(-7.51199928711923,0.724543022590624,
25.4762312558019));
#16445=CARTESIAN_POINT('Ctrl Pts',(-7.35822688079568,0.444367128059778,
25.4642280690126));
#16446=CARTESIAN_POINT('Ctrl Pts',(-7.32102560975795,0.147979855988516,
25.4522248822233));
#16447=CARTESIAN_POINT('Ctrl Pts',(-7.28382433872022,-0.148407416082745,
25.440221695434));
#16448=CARTESIAN_POINT('Ctrl Pts',(-7.36358464744707,-0.45789534472374,
25.4282185086447));
#16449=CARTESIAN_POINT('Ctrl Pts',(-7.53940549437993,-0.699383189959225,
25.4162153218553));
#16450=CARTESIAN_POINT('Ctrl Pts',(-7.7152263413128,-0.94087103519471,25.404212135066));
#16451=CARTESIAN_POINT('Ctrl Pts',(-7.98526240565967,-1.11182427083168,
25.3922089482767));
#16452=CARTESIAN_POINT('Ctrl Pts',(-8.27875123560312,-1.16744491727784,
25.3802057614874));
#16453=CARTESIAN_POINT('Ctrl Pts',(-8.57224006554658,-1.223065563724,25.3682025746981));
#16454=CARTESIAN_POINT('Ctrl Pts',(-8.88610136060142,-1.16276985666958,
25.3561993879087));
#16455=CARTESIAN_POINT('Ctrl Pts',(-9.1380883482027,-1.00235817476237,25.3441962011194));
#16456=CARTESIAN_POINT('Ctrl Pts',(-9.39007533580398,-0.841946492855162,
25.3321930143301));
#16457=CARTESIAN_POINT('Ctrl Pts',(-9.57754329642243,-0.583102430600965,
25.3201898275408));
#16458=CARTESIAN_POINT('Ctrl Pts',(-9.65136659729245,-0.293655596344101,
25.3081866407515));
#16459=CARTESIAN_POINT('Ctrl Pts',(-9.67581103310572,-0.197813707970602,
25.304212135066));
#16460=CARTESIAN_POINT('Ctrl Pts',(-9.68822500000012,-0.0989100500907355,
25.3002376293806));
#16461=CARTESIAN_POINT('Ctrl Pts',(-9.688225,1.39321887360211E-12,25.2962631236951));
#16462=CARTESIAN_POINT('Ctrl Pts',(-9.688225,-3.91631171936524E-13,25.2537368763049));
#16463=CARTESIAN_POINT('Ctrl Pts',(-9.6882249999999,-0.298712821306451,
25.2657400630942));
#16464=CARTESIAN_POINT('Ctrl Pts',(-9.57054245632569,-0.595858078271815,
25.2777432498835));
#16465=CARTESIAN_POINT('Ctrl Pts',(-9.36601586214915,-0.813569405232931,
25.2897464366728));
#16466=CARTESIAN_POINT('Ctrl Pts',(-9.16148926797261,-1.03128073219405,
25.3017496234621));
#16467=CARTESIAN_POINT('Ctrl Pts',(-8.87226522412824,-1.16727314847142,
25.3137528102514));
#16468=CARTESIAN_POINT('Ctrl Pts',(-8.57413435701432,-1.18591009260191,
25.3257559970408));
#16469=CARTESIAN_POINT('Ctrl Pts',(-8.27600348990039,-1.20454703673241,
25.3377591838301));
#16470=CARTESIAN_POINT('Ctrl Pts',(-7.97209482032085,-1.10563290540104,
25.3497623706194));
#16471=CARTESIAN_POINT('Ctrl Pts',(-7.74204705372056,-0.915087963996534,
25.3617655574087));
#16472=CARTESIAN_POINT('Ctrl Pts',(-7.51199928712028,-0.724543022592027,
25.373768744198));
#16473=CARTESIAN_POINT('Ctrl Pts',(-7.35822688079636,-0.444367128061476,
25.3857719309873));
#16474=CARTESIAN_POINT('Ctrl Pts',(-7.32102560975818,-0.14797985599034,
25.3977751177767));
#16475=CARTESIAN_POINT('Ctrl Pts',(-7.28382433872,0.148407416080797,25.409778304566));
#16476=CARTESIAN_POINT('Ctrl Pts',(-7.36358464744633,0.457895344721843,
25.4217814913553));
#16477=CARTESIAN_POINT('Ctrl Pts',(-7.53940549437873,0.699383189957575,
25.4337846781446));
#16478=CARTESIAN_POINT('Ctrl Pts',(-7.71522634131114,0.940871035193308,
25.4457878649339));
#16479=CARTESIAN_POINT('Ctrl Pts',(-7.98526240565763,1.11182427083072,25.4577910517232));
#16480=CARTESIAN_POINT('Ctrl Pts',(-8.27875123560092,1.16744491727742,25.4697942385126));
#16481=CARTESIAN_POINT('Ctrl Pts',(-8.5722400655442,1.22306556372412,25.4817974253019));
#16482=CARTESIAN_POINT('Ctrl Pts',(-8.88610136059908,1.16276985667034,25.4938006120912));
#16483=CARTESIAN_POINT('Ctrl Pts',(-9.13808834820063,1.00235817476368,25.5058037988805));
#16484=CARTESIAN_POINT('Ctrl Pts',(-9.39007533580219,0.84194649285703,25.5178069856698));
#16485=CARTESIAN_POINT('Ctrl Pts',(-9.57754329642115,0.583102430603301,
25.5298101724591));
#16486=CARTESIAN_POINT('Ctrl Pts',(-9.65136659729179,0.293655596346667,
25.5418133592485));
#16487=CARTESIAN_POINT('Ctrl Pts',(-9.67581103310542,0.197813707972699,
25.5457878649339));
#16488=CARTESIAN_POINT('Ctrl Pts',(-9.68822500000003,0.0989100500923029,
25.5497623706194));
#16489=CARTESIAN_POINT('Ctrl Pts',(-9.688225,-3.66040531218914E-13,25.5537368763049));
#16490=CARTESIAN_POINT('Origin',(-8.5,0.,1.8));
#16491=CARTESIAN_POINT('',(-9.688225,1.37678757283766E-12,25.8962631236951));
#16492=CARTESIAN_POINT('',(-9.688225,-3.40394379350073E-13,25.8537368763049));
#16493=CARTESIAN_POINT('',(-9.688225,-1.45515594291686E-16,1.8));
#16494=CARTESIAN_POINT('Ctrl Pts',(-9.688225,1.37678757283766E-12,25.8962631236951));
#16495=CARTESIAN_POINT('Ctrl Pts',(-9.68822499999965,0.298712821307437,
25.8842599369058));
#16496=CARTESIAN_POINT('Ctrl Pts',(-9.5705424563252,0.595858078272703,25.8722567501165));
#16497=CARTESIAN_POINT('Ctrl Pts',(-9.36601586214848,0.813569405233649,
25.8602535633272));
#16498=CARTESIAN_POINT('Ctrl Pts',(-9.16148926797175,1.0312807321946,25.8482503765379));
#16499=CARTESIAN_POINT('Ctrl Pts',(-8.87226522412728,1.16727314847173,25.8362471897485));
#16500=CARTESIAN_POINT('Ctrl Pts',(-8.57413435701333,1.18591009260197,25.8242440029592));
#16501=CARTESIAN_POINT('Ctrl Pts',(-8.27600348989939,1.20454703673222,25.8122408161699));
#16502=CARTESIAN_POINT('Ctrl Pts',(-7.97209482031993,1.1056329054006,25.8002376293806));
#16503=CARTESIAN_POINT('Ctrl Pts',(-7.7420470537198,0.915087963995906,25.7882344425913));
#16504=CARTESIAN_POINT('Ctrl Pts',(-7.51199928711968,0.724543022591208,
25.776231255802));
#16505=CARTESIAN_POINT('Ctrl Pts',(-7.35822688079599,0.44436712806053,25.7642280690126));
#16506=CARTESIAN_POINT('Ctrl Pts',(-7.32102560975805,0.147979855989362,
25.7522248822233));
#16507=CARTESIAN_POINT('Ctrl Pts',(-7.28382433872012,-0.148407416081805,
25.740221695434));
#16508=CARTESIAN_POINT('Ctrl Pts',(-7.36358464744671,-0.457895344722785,
25.7282185086447));
#16509=CARTESIAN_POINT('Ctrl Pts',(-7.53940549437931,-0.699383189958372,
25.7162153218554));
#16510=CARTESIAN_POINT('Ctrl Pts',(-7.71522634131192,-0.940871035193959,
25.7042121350661));
#16511=CARTESIAN_POINT('Ctrl Pts',(-7.98526240565856,-1.11182427083115,
25.6922089482767));
#16512=CARTESIAN_POINT('Ctrl Pts',(-8.27875123560188,-1.1674449172776,25.6802057614874));
#16513=CARTESIAN_POINT('Ctrl Pts',(-8.57224006554521,-1.22306556372406,
25.6682025746981));
#16514=CARTESIAN_POINT('Ctrl Pts',(-8.88610136060005,-1.16276985667002,
25.6561993879088));
#16515=CARTESIAN_POINT('Ctrl Pts',(-9.13808834820147,-1.00235817476316,
25.6441962011195));
#16516=CARTESIAN_POINT('Ctrl Pts',(-9.39007533580288,-0.841946492856292,
25.6321930143302));
#16517=CARTESIAN_POINT('Ctrl Pts',(-9.57754329642163,-0.583102430602408,
25.6201898275408));
#16518=CARTESIAN_POINT('Ctrl Pts',(-9.65136659729204,-0.293655596345712,
25.6081866407515));
#16519=CARTESIAN_POINT('Ctrl Pts',(-9.67581103310559,-0.197813707971703,
25.6042121350661));
#16520=CARTESIAN_POINT('Ctrl Pts',(-9.68822500000012,-0.0989100500912729,
25.6002376293806));
#16521=CARTESIAN_POINT('Ctrl Pts',(-9.688225,1.41875400316849E-12,25.5962631236951));
#16522=CARTESIAN_POINT('Ctrl Pts',(-9.688225,-3.66040531218914E-13,25.5537368763049));
#16523=CARTESIAN_POINT('Ctrl Pts',(-9.68822499999991,-0.298712821306471,
25.5657400630942));
#16524=CARTESIAN_POINT('Ctrl Pts',(-9.57054245632567,-0.595858078271881,
25.5777432498835));
#16525=CARTESIAN_POINT('Ctrl Pts',(-9.36601586214907,-0.813569405233011,
25.5897464366728));
#16526=CARTESIAN_POINT('Ctrl Pts',(-9.16148926797248,-1.03128073219414,
25.6017496234621));
#16527=CARTESIAN_POINT('Ctrl Pts',(-8.87226522412805,-1.16727314847149,
25.6137528102514));
#16528=CARTESIAN_POINT('Ctrl Pts',(-8.57413435701407,-1.18591009260193,
25.6257559970408));
#16529=CARTESIAN_POINT('Ctrl Pts',(-8.27600348990009,-1.20454703673236,
25.6377591838301));
#16530=CARTESIAN_POINT('Ctrl Pts',(-7.97209482032053,-1.1056329054009,25.6497623706194));
#16531=CARTESIAN_POINT('Ctrl Pts',(-7.74204705372027,-0.915087963996292,
25.6617655574087));
#16532=CARTESIAN_POINT('Ctrl Pts',(-7.51199928712001,-0.724543022591682,
25.673768744198));
#16533=CARTESIAN_POINT('Ctrl Pts',(-7.35822688079617,-0.444367128061026,
25.6857719309874));
#16534=CARTESIAN_POINT('Ctrl Pts',(-7.32102560975811,-0.147979855989829,
25.6977751177767));
#16535=CARTESIAN_POINT('Ctrl Pts',(-7.28382433872006,0.148407416081368,
25.709778304566));
#16536=CARTESIAN_POINT('Ctrl Pts',(-7.36358464744655,0.457895344722428,
25.7217814913553));
#16537=CARTESIAN_POINT('Ctrl Pts',(-7.53940549437912,0.699383189958101,
25.7337846781446));
#16538=CARTESIAN_POINT('Ctrl Pts',(-7.71522634131168,0.940871035193773,
25.7457878649339));
#16539=CARTESIAN_POINT('Ctrl Pts',(-7.98526240565833,1.11182427083105,25.7577910517233));
#16540=CARTESIAN_POINT('Ctrl Pts',(-8.27875123560169,1.16744491727756,25.7697942385126));
#16541=CARTESIAN_POINT('Ctrl Pts',(-8.57224006554505,1.22306556372408,25.7817974253019));
#16542=CARTESIAN_POINT('Ctrl Pts',(-8.88610136059995,1.16276985667006,25.7938006120912));
#16543=CARTESIAN_POINT('Ctrl Pts',(-9.13808834820141,1.00235817476319,25.8058037988805));
#16544=CARTESIAN_POINT('Ctrl Pts',(-9.39007533580287,0.841946492856317,
25.8178069856699));
#16545=CARTESIAN_POINT('Ctrl Pts',(-9.57754329642165,0.583102430602388,
25.8298101724592));
#16546=CARTESIAN_POINT('Ctrl Pts',(-9.65136659729205,0.293655596345644,
25.8418133592485));
#16547=CARTESIAN_POINT('Ctrl Pts',(-9.6758110331055,0.197813707972026,25.8457878649339));
#16548=CARTESIAN_POINT('Ctrl Pts',(-9.68822500000002,0.0989100500920135,
25.8497623706194));
#16549=CARTESIAN_POINT('Ctrl Pts',(-9.688225,-2.72781797150401E-13,25.8537368763049));
#16550=CARTESIAN_POINT('Origin',(-8.5,0.,1.8));
#16551=CARTESIAN_POINT('',(-9.688225,1.40254474700896E-12,26.1962631236951));
#16552=CARTESIAN_POINT('',(-9.688225,-3.14803738632463E-13,26.1537368763049));
#16553=CARTESIAN_POINT('',(-9.688225,-1.45515594291686E-16,1.8));
#16554=CARTESIAN_POINT('Ctrl Pts',(-9.688225,1.40254474700896E-12,26.1962631236951));
#16555=CARTESIAN_POINT('Ctrl Pts',(-9.68822499999965,0.298712821307485,
26.1842599369058));
#16556=CARTESIAN_POINT('Ctrl Pts',(-9.57054245632517,0.59585807827277,26.1722567501165));
#16557=CARTESIAN_POINT('Ctrl Pts',(-9.36601586214841,0.813569405233717,
26.1602535633272));
#16558=CARTESIAN_POINT('Ctrl Pts',(-9.16148926797166,1.03128073219466,26.1482503765379));
#16559=CARTESIAN_POINT('Ctrl Pts',(-8.87226522412714,1.16727314847177,26.1362471897485));
#16560=CARTESIAN_POINT('Ctrl Pts',(-8.57413435701317,1.18591009260198,26.1242440029592));
#16561=CARTESIAN_POINT('Ctrl Pts',(-8.2760034898992,1.20454703673219,26.1122408161699));
#16562=CARTESIAN_POINT('Ctrl Pts',(-7.97209482031974,1.10563290540052,26.1002376293806));
#16563=CARTESIAN_POINT('Ctrl Pts',(-7.74204705371963,0.91508796399576,26.0882344425913));
#16564=CARTESIAN_POINT('Ctrl Pts',(-7.51199928711952,0.724543022591003,
26.076231255802));
#16565=CARTESIAN_POINT('Ctrl Pts',(-7.35822688079588,0.444367128060268,
26.0642280690126));
#16566=CARTESIAN_POINT('Ctrl Pts',(-7.32102560975802,0.147979855989069,
26.0522248822233));
#16567=CARTESIAN_POINT('Ctrl Pts',(-7.28382433872016,-0.14840741608213,
26.040221695434));
#16568=CARTESIAN_POINT('Ctrl Pts',(-7.36358464744683,-0.457895344723115,
26.0282185086447));
#16569=CARTESIAN_POINT('Ctrl Pts',(-7.53940549437953,-0.699383189958666,
26.0162153218554));
#16570=CARTESIAN_POINT('Ctrl Pts',(-7.71522634131222,-0.940871035194217,
26.004212135066));
#16571=CARTESIAN_POINT('Ctrl Pts',(-7.98526240565894,-1.11182427083133,
25.9922089482767));
#16572=CARTESIAN_POINT('Ctrl Pts',(-8.27875123560231,-1.16744491727768,
25.9802057614874));
#16573=CARTESIAN_POINT('Ctrl Pts',(-8.57224006554568,-1.22306556372404,
25.9682025746981));
#16574=CARTESIAN_POINT('Ctrl Pts',(-8.88610136060052,-1.16276985666987,
25.9561993879088));
#16575=CARTESIAN_POINT('Ctrl Pts',(-9.13808834820189,-1.00235817476289,
25.9441962011195));
#16576=CARTESIAN_POINT('Ctrl Pts',(-9.39007533580326,-0.841946492855907,
25.9321930143301));
#16577=CARTESIAN_POINT('Ctrl Pts',(-9.5775432964219,-0.583102430601916,
25.9201898275408));
#16578=CARTESIAN_POINT('Ctrl Pts',(-9.65136659729218,-0.293655596345164,
25.9081866407515));
#16579=CARTESIAN_POINT('Ctrl Pts',(-9.67581103310563,-0.197813707971339,
25.904212135066));
#16580=CARTESIAN_POINT('Ctrl Pts',(-9.68822500000012,-0.0989100500911121,
25.9002376293806));
#16581=CARTESIAN_POINT('Ctrl Pts',(-9.688225,1.37678757283766E-12,25.8962631236951));
#16582=CARTESIAN_POINT('Ctrl Pts',(-9.688225,-2.72781797150401E-13,25.8537368763049));
#16583=CARTESIAN_POINT('Ctrl Pts',(-9.68822499999993,-0.2987128213064,25.8657400630942));
#16584=CARTESIAN_POINT('Ctrl Pts',(-9.5705424563257,-0.595858078271841,
25.8777432498835));
#16585=CARTESIAN_POINT('Ctrl Pts',(-9.36601586214909,-0.813569405232992,
25.8897464366728));
#16586=CARTESIAN_POINT('Ctrl Pts',(-9.16148926797249,-1.03128073219414,
25.9017496234621));
#16587=CARTESIAN_POINT('Ctrl Pts',(-8.87226522412803,-1.1672731484715,25.9137528102514));
#16588=CARTESIAN_POINT('Ctrl Pts',(-8.57413435701403,-1.18591009260193,
25.9257559970408));
#16589=CARTESIAN_POINT('Ctrl Pts',(-8.27600348990003,-1.20454703673236,
25.9377591838301));
#16590=CARTESIAN_POINT('Ctrl Pts',(-7.97209482032044,-1.10563290540087,
25.9497623706194));
#16591=CARTESIAN_POINT('Ctrl Pts',(-7.74204705372019,-0.915087963996222,
25.9617655574087));
#16592=CARTESIAN_POINT('Ctrl Pts',(-7.51199928711993,-0.724543022591577,
25.973768744198));
#16593=CARTESIAN_POINT('Ctrl Pts',(-7.3582268807961,-0.444367128060879,
25.9857719309874));
#16594=CARTESIAN_POINT('Ctrl Pts',(-7.32102560975809,-0.147979855989653,
25.9977751177767));
#16595=CARTESIAN_POINT('Ctrl Pts',(-7.28382433872008,0.148407416081572,
26.009778304566));
#16596=CARTESIAN_POINT('Ctrl Pts',(-7.36358464744663,0.457895344722644,
26.0217814913553));
#16597=CARTESIAN_POINT('Ctrl Pts',(-7.53940549437926,0.699383189958299,
26.0337846781446));
#16598=CARTESIAN_POINT('Ctrl Pts',(-7.71522634131189,0.940871035193953,
26.045787864934));
#16599=CARTESIAN_POINT('Ctrl Pts',(-7.98526240565859,1.11182427083118,26.0577910517233));
#16600=CARTESIAN_POINT('Ctrl Pts',(-8.27875123560199,1.16744491727762,26.0697942385126));
#16601=CARTESIAN_POINT('Ctrl Pts',(-8.5722400655454,1.22306556372406,26.0817974253019));
#16602=CARTESIAN_POINT('Ctrl Pts',(-8.8861013606003,1.16276985666995,26.0938006120912));
#16603=CARTESIAN_POINT('Ctrl Pts',(-9.13808834820173,1.00235817476299,26.1058037988806));
#16604=CARTESIAN_POINT('Ctrl Pts',(-9.39007533580316,0.84194649285602,26.1178069856699));
#16605=CARTESIAN_POINT('Ctrl Pts',(-9.57754329642187,0.583102430602004,
26.1298101724592));
#16606=CARTESIAN_POINT('Ctrl Pts',(-9.65136659729217,0.293655596345211,
26.1418133592485));
#16607=CARTESIAN_POINT('Ctrl Pts',(-9.67581103310554,0.197813707971715,
26.145787864934));
#16608=CARTESIAN_POINT('Ctrl Pts',(-9.68822500000003,0.0989100500918363,
26.1497623706194));
#16609=CARTESIAN_POINT('Ctrl Pts',(-9.688225,-3.14803738632463E-13,26.1537368763049));
#16610=CARTESIAN_POINT('Origin',(-8.5,0.,1.8));
#16611=CARTESIAN_POINT('',(-9.688225,1.42807987657534E-12,26.4962631236951));
#16612=CARTESIAN_POINT('',(-9.68738609224838,-0.000346572711688259,26.4537368763049));
#16613=CARTESIAN_POINT('',(-9.688225,-1.45515594291686E-16,1.8));
#16614=CARTESIAN_POINT('Ctrl Pts',(-9.688225,1.56308299636976E-12,26.4962631236951));
#16615=CARTESIAN_POINT('Ctrl Pts',(-9.68822499999961,0.2987128213076,26.4842599369058));
#16616=CARTESIAN_POINT('Ctrl Pts',(-9.57054245632512,0.595858078272826,
26.4722567501165));
#16617=CARTESIAN_POINT('Ctrl Pts',(-9.36601586214839,0.813569405233736,
26.4602535633272));
#16618=CARTESIAN_POINT('Ctrl Pts',(-9.16148926797167,1.03128073219465,26.4482503765379));
#16619=CARTESIAN_POINT('Ctrl Pts',(-8.8722652241272,1.16727314847174,26.4362471897485));
#16620=CARTESIAN_POINT('Ctrl Pts',(-8.57413435701328,1.18591009260198,26.4242440029592));
#16621=CARTESIAN_POINT('Ctrl Pts',(-8.27600348989936,1.20454703673221,26.4122408161699));
#16622=CARTESIAN_POINT('Ctrl Pts',(-7.97209482031993,1.1056329054006,26.4002376293806));
#16623=CARTESIAN_POINT('Ctrl Pts',(-7.74204705371982,0.915087963995916,
26.3882344425913));
#16624=CARTESIAN_POINT('Ctrl Pts',(-7.51199928711971,0.724543022591235,
26.376231255802));
#16625=CARTESIAN_POINT('Ctrl Pts',(-7.35822688079601,0.444367128060588,
26.3642280690126));
#16626=CARTESIAN_POINT('Ctrl Pts',(-7.32102560975806,0.147979855989445,
26.3522248822233));
#16627=CARTESIAN_POINT('Ctrl Pts',(-7.28382433872011,-0.148407416081697,
26.340221695434));
#16628=CARTESIAN_POINT('Ctrl Pts',(-7.36358464744666,-0.457895344722659,
26.3282185086447));
#16629=CARTESIAN_POINT('Ctrl Pts',(-7.53940549437922,-0.69938318995825,
26.3162153218554));
#16630=CARTESIAN_POINT('Ctrl Pts',(-7.71522634131179,-0.940871035193841,
26.3042121350661));
#16631=CARTESIAN_POINT('Ctrl Pts',(-7.98526240565837,-1.11182427083106,
26.2922089482768));
#16632=CARTESIAN_POINT('Ctrl Pts',(-8.27875123560167,-1.16744491727756,
26.2802057614874));
#16633=CARTESIAN_POINT('Ctrl Pts',(-8.57224006554497,-1.22306556372407,
26.2682025746981));
#16634=CARTESIAN_POINT('Ctrl Pts',(-8.88610136059979,-1.1627698566701,26.2561993879088));
#16635=CARTESIAN_POINT('Ctrl Pts',(-9.13808834820122,-1.00235817476331,
26.2441962011195));
#16636=CARTESIAN_POINT('Ctrl Pts',(-9.39007533580266,-0.841946492856519,
26.2321930143302));
#16637=CARTESIAN_POINT('Ctrl Pts',(-9.57754329642146,-0.583102430602707,
26.2201898275409));
#16638=CARTESIAN_POINT('Ctrl Pts',(-9.65136659729195,-0.293655596346055,
26.2081866407515));
#16639=CARTESIAN_POINT('Ctrl Pts',(-9.67581103310556,-0.197813707971944,
26.2042121350661));
#16640=CARTESIAN_POINT('Ctrl Pts',(-9.68822500000012,-0.0989100500914016,
26.2002376293806));
#16641=CARTESIAN_POINT('Ctrl Pts',(-9.688225,1.40254474700896E-12,26.1962631236951));
#16642=CARTESIAN_POINT('Ctrl Pts',(-9.688225,-3.14803738632463E-13,26.1537368763049));
#16643=CARTESIAN_POINT('Ctrl Pts',(-9.68822499999992,-0.298712821306329,
26.1657400630942));
#16644=CARTESIAN_POINT('Ctrl Pts',(-9.57054245632577,-0.595858078271657,
26.1777432498835));
#16645=CARTESIAN_POINT('Ctrl Pts',(-9.3660158621493,-0.813569405232776,
26.1897464366728));
#16646=CARTESIAN_POINT('Ctrl Pts',(-9.16148926797282,-1.0312807321939,26.2017496234621));
#16647=CARTESIAN_POINT('Ctrl Pts',(-8.87226522412854,-1.16727314847131,
26.2137528102514));
#16648=CARTESIAN_POINT('Ctrl Pts',(-8.57413435701466,-1.18591009260189,
26.2257559970407));
#16649=CARTESIAN_POINT('Ctrl Pts',(-8.27600348990081,-1.20454703673247,
26.2377591838301));
#16650=CARTESIAN_POINT('Ctrl Pts',(-7.97209482032131,-1.10563290540124,
26.2497623706194));
#16651=CARTESIAN_POINT('Ctrl Pts',(-7.74204705372099,-0.915087963996884,
26.2617655574087));
#16652=CARTESIAN_POINT('Ctrl Pts',(-7.51199928712063,-0.724543022592498,
26.273768744198));
#16653=CARTESIAN_POINT('Ctrl Pts',(-7.35822688079658,-0.444367128062047,
26.2857719309873));
#16654=CARTESIAN_POINT('Ctrl Pts',(-7.32102560975825,-0.147979855990952,
26.2977751177766));
#16655=CARTESIAN_POINT('Ctrl Pts',(-7.28382433871992,0.148407416080143,
26.3097783045659));
#16656=CARTESIAN_POINT('Ctrl Pts',(-7.36358464744607,0.457895344721206,
26.3217814913553));
#16657=CARTESIAN_POINT('Ctrl Pts',(-7.53940549437833,0.699383189957022,
26.3337846781446));
#16658=CARTESIAN_POINT('Ctrl Pts',(-7.71522634131058,0.940871035192837,
26.3457878649339));
#16659=CARTESIAN_POINT('Ctrl Pts',(-7.98526240565695,1.1118242708304,26.3577910517232));
#16660=CARTESIAN_POINT('Ctrl Pts',(-8.27875123560018,1.16744491727728,26.3697942385125));
#16661=CARTESIAN_POINT('Ctrl Pts',(-8.5722400655434,1.22306556372416,26.3817974253018));
#16662=CARTESIAN_POINT('Ctrl Pts',(-8.8861013605983,1.16276985667059,26.3938006120912));
#16663=CARTESIAN_POINT('Ctrl Pts',(-9.13808834819994,1.00235817476413,26.4058037988805));
#16664=CARTESIAN_POINT('Ctrl Pts',(-9.39007533580159,0.841946492857656,
26.4178069856698));
#16665=CARTESIAN_POINT('Ctrl Pts',(-9.57754329642071,0.583102430604084,
26.4298101724591));
#16666=CARTESIAN_POINT('Ctrl Pts',(-9.65136659729157,0.293655596347526,
26.4418133592484));
#16667=CARTESIAN_POINT('Ctrl Pts',(-9.67581103310532,0.197813707973359,
26.4457878649339));
#16668=CARTESIAN_POINT('Ctrl Pts',(-9.68822500000001,0.0989100500927401,
26.4497623706194));
#16669=CARTESIAN_POINT('Ctrl Pts',(-9.688225,-1.54098955817972E-13,26.4537368763048));
#16670=CARTESIAN_POINT('Origin',(-8.5,0.,1.8));
#16671=CARTESIAN_POINT('',(-9.688225,1.45372602844418E-12,26.7962631236951));
#16672=CARTESIAN_POINT('',(-9.68877351310573,-0.000284106499024444,26.7537368763048));
#16673=CARTESIAN_POINT('',(-9.688225,-1.45515594291686E-16,1.8));
#16674=CARTESIAN_POINT('Ctrl Pts',(-9.688225,1.45372602844418E-12,26.7962631236951));
#16675=CARTESIAN_POINT('Ctrl Pts',(-9.68822499999964,0.298712821307536,
26.7842599369058));
#16676=CARTESIAN_POINT('Ctrl Pts',(-9.57054245632514,0.595858078272816,
26.7722567501165));
#16677=CARTESIAN_POINT('Ctrl Pts',(-9.36601586214838,0.813569405233754,
26.7602535633272));
#16678=CARTESIAN_POINT('Ctrl Pts',(-9.16148926797161,1.03128073219469,26.7482503765379));
#16679=CARTESIAN_POINT('Ctrl Pts',(-8.87226522412709,1.16727314847179,26.7362471897485));
#16680=CARTESIAN_POINT('Ctrl Pts',(-8.57413435701312,1.18591009260199,26.7242440029592));
#16681=CARTESIAN_POINT('Ctrl Pts',(-8.27600348989915,1.20454703673218,26.7122408161699));
#16682=CARTESIAN_POINT('Ctrl Pts',(-7.97209482031969,1.10563290540049,26.7002376293806));
#16683=CARTESIAN_POINT('Ctrl Pts',(-7.74204705371959,0.915087963995727,
26.6882344425913));
#16684=CARTESIAN_POINT('Ctrl Pts',(-7.51199928711949,0.724543022590961,
26.6762312558019));
#16685=CARTESIAN_POINT('Ctrl Pts',(-7.35822688079586,0.444367128060219,
26.6642280690126));
#16686=CARTESIAN_POINT('Ctrl Pts',(-7.32102560975801,0.147979855989018,
26.6522248822233));
#16687=CARTESIAN_POINT('Ctrl Pts',(-7.28382433872016,-0.148407416082183,
26.640221695434));
#16688=CARTESIAN_POINT('Ctrl Pts',(-7.36358464744685,-0.457895344723164,
26.6282185086447));
#16689=CARTESIAN_POINT('Ctrl Pts',(-7.53940549437956,-0.699383189958707,
26.6162153218554));
#16690=CARTESIAN_POINT('Ctrl Pts',(-7.71522634131226,-0.940871035194251,
26.604212135066));
#16691=CARTESIAN_POINT('Ctrl Pts',(-7.98526240565899,-1.11182427083135,
26.5922089482767));
#16692=CARTESIAN_POINT('Ctrl Pts',(-8.27875123560236,-1.16744491727769,
26.5802057614874));
#16693=CARTESIAN_POINT('Ctrl Pts',(-8.57224006554573,-1.22306556372403,
26.5682025746981));
#16694=CARTESIAN_POINT('Ctrl Pts',(-8.88610136060057,-1.16276985666985,
26.5561993879088));
#16695=CARTESIAN_POINT('Ctrl Pts',(-9.13808834820193,-1.00235817476286,
26.5441962011195));
#16696=CARTESIAN_POINT('Ctrl Pts',(-9.39007533580329,-0.841946492855868,
26.5321930143301));
#16697=CARTESIAN_POINT('Ctrl Pts',(-9.57754329642193,-0.58310243060187,
26.5201898275408));
#16698=CARTESIAN_POINT('Ctrl Pts',(-9.65136659729219,-0.293655596345114,
26.5081866407515));
#16699=CARTESIAN_POINT('Ctrl Pts',(-9.67581103310565,-0.197813707971245,
26.504212135066));
#16700=CARTESIAN_POINT('Ctrl Pts',(-9.68822500000013,-0.0989100500909709,
26.5002376293806));
#16701=CARTESIAN_POINT('Ctrl Pts',(-9.688225,1.56308299636976E-12,26.4962631236951));
#16702=CARTESIAN_POINT('Ctrl Pts',(-9.68674334601053,-0.000612106443772073,
26.4537368763049));
#16703=CARTESIAN_POINT('Ctrl Pts',(-9.68760064018175,-0.15491495328169,
26.4599199595912));
#16704=CARTESIAN_POINT('Ctrl Pts',(-9.65970073938658,-0.308953253913664,
26.4661030428775));
#16705=CARTESIAN_POINT('Ctrl Pts',(-9.60165140328844,-0.450727135541932,
26.4722861261638));
#16706=CARTESIAN_POINT('Ctrl Pts',(-9.45230672359085,-0.815471616089674,
26.4881934673154));
#16707=CARTESIAN_POINT('Ctrl Pts',(-9.10340632447576,-1.09903928742264,
26.504100808467));
#16708=CARTESIAN_POINT('Ctrl Pts',(-8.71613991619992,-1.17052229766671,
26.5200081496187));
#16709=CARTESIAN_POINT('Ctrl Pts',(-8.32887350792413,-1.24200530791077,
26.5359154907703));
#16710=CARTESIAN_POINT('Ctrl Pts',(-7.90324109048761,-1.10140365706596,
26.5518228319219));
#16711=CARTESIAN_POINT('Ctrl Pts',(-7.63272502524997,-0.81444926346103,
26.5677301730735));
#16712=CARTESIAN_POINT('Ctrl Pts',(-7.49746699263114,-0.670972066658563,
26.5756838436493));
#16713=CARTESIAN_POINT('Ctrl Pts',(-7.40098804806204,-0.490906684166065,
26.5836375142251));
#16714=CARTESIAN_POINT('Ctrl Pts',(-7.35102428689118,-0.298746822161143,
26.591591184801));
#16715=CARTESIAN_POINT('Ctrl Pts',(-7.3010605257203,-0.106586960156177,
26.5995448553768));
#16716=CARTESIAN_POINT('Ctrl Pts',(-7.29761194794768,0.0976673813612168,
26.6074985259526));
#16717=CARTESIAN_POINT('Ctrl Pts',(-7.34585293277445,0.288856420725844,
26.6154521965284));
#16718=CARTESIAN_POINT('Ctrl Pts',(-7.44233490242797,0.671234499455056,
26.63135953768));
#16719=CARTESIAN_POINT('Ctrl Pts',(-7.74557512247899,1.00135136957321,26.6472668788316));
#16720=CARTESIAN_POINT('Ctrl Pts',(-8.11861322531683,1.1275562251199,26.6631742199833));
#16721=CARTESIAN_POINT('Ctrl Pts',(-8.49165132815463,1.25376108066657,26.6790815611349));
#16722=CARTESIAN_POINT('Ctrl Pts',(-8.93448731377924,1.17605392164181,26.6949889022865));
#16723=CARTESIAN_POINT('Ctrl Pts',(-9.24258185301928,0.930248868124899,
26.7108962434381));
#16724=CARTESIAN_POINT('Ctrl Pts',(-9.51916201639636,0.709586723225101,
26.7251764543937));
#16725=CARTESIAN_POINT('Ctrl Pts',(-9.68715582329318,0.353456699772103,
26.7394566653493));
#16726=CARTESIAN_POINT('Ctrl Pts',(-9.68953524092888,-0.000678649168437481,
26.7537368763049));
#16727=CARTESIAN_POINT('Origin',(-8.5,0.,1.8));
#16728=CARTESIAN_POINT('',(-9.688225,1.47926115801056E-12,27.0962631236951));
#16729=CARTESIAN_POINT('',(-9.688225,-2.37920794177171E-13,27.0537368763048));
#16730=CARTESIAN_POINT('',(-9.688225,-1.45515594291686E-16,1.8));
#16731=CARTESIAN_POINT('Ctrl Pts',(-9.688225,1.6144863224099E-12,27.0962631236951));
#16732=CARTESIAN_POINT('Ctrl Pts',(-9.6882249999996,0.298712821307742,27.0842599369058));
#16733=CARTESIAN_POINT('Ctrl Pts',(-9.57054245632502,0.59585807827305,27.0722567501165));
#16734=CARTESIAN_POINT('Ctrl Pts',(-9.36601586214817,0.81356940523397,27.0602535633272));
#16735=CARTESIAN_POINT('Ctrl Pts',(-9.16148926797132,1.03128073219489,27.0482503765378));
#16736=CARTESIAN_POINT('Ctrl Pts',(-8.87226522412671,1.16727314847192,27.0362471897485));
#16737=CARTESIAN_POINT('Ctrl Pts',(-8.57413435701269,1.18591009260201,27.0242440029592));
#16738=CARTESIAN_POINT('Ctrl Pts',(-8.27600348989867,1.2045470367321,27.0122408161699));
#16739=CARTESIAN_POINT('Ctrl Pts',(-7.9720948203192,1.10563290540027,27.0002376293806));
#16740=CARTESIAN_POINT('Ctrl Pts',(-7.74204705371915,0.915087963995366,
26.9882344425912));
#16741=CARTESIAN_POINT('Ctrl Pts',(-7.51199928711911,0.724543022590461,
26.9762312558019));
#16742=CARTESIAN_POINT('Ctrl Pts',(-7.3582268807956,0.44436712805959,26.9642280690126));
#16743=CARTESIAN_POINT('Ctrl Pts',(-7.32102560975792,0.147979855988322,
26.9522248822233));
#16744=CARTESIAN_POINT('Ctrl Pts',(-7.28382433872024,-0.148407416082945,
26.940221695434));
#16745=CARTESIAN_POINT('Ctrl Pts',(-7.36358464744715,-0.457895344723927,
26.9282185086446));
#16746=CARTESIAN_POINT('Ctrl Pts',(-7.53940549438005,-0.699383189959383,
26.9162153218553));
#16747=CARTESIAN_POINT('Ctrl Pts',(-7.71522634131295,-0.94087103519484,
26.904212135066));
#16748=CARTESIAN_POINT('Ctrl Pts',(-7.98526240565985,-1.11182427083176,
26.8922089482767));
#16749=CARTESIAN_POINT('Ctrl Pts',(-8.27875123560331,-1.16744491727787,
26.8802057614874));
#16750=CARTESIAN_POINT('Ctrl Pts',(-8.57224006554678,-1.22306556372398,
26.8682025746981));
#16751=CARTESIAN_POINT('Ctrl Pts',(-8.88610136060161,-1.16276985666952,
26.8561993879087));
#16752=CARTESIAN_POINT('Ctrl Pts',(-9.13808834820286,-1.00235817476227,
26.8441962011194));
#16753=CARTESIAN_POINT('Ctrl Pts',(-9.39007533580411,-0.841946492855016,
26.8321930143301));
#16754=CARTESIAN_POINT('Ctrl Pts',(-9.57754329642253,-0.583102430600788,
26.8201898275408));
#16755=CARTESIAN_POINT('Ctrl Pts',(-9.6513665972925,-0.293655596343911,
26.8081866407515));
#16756=CARTESIAN_POINT('Ctrl Pts',(-9.67581103310575,-0.197813707970453,
26.804212135066));
#16757=CARTESIAN_POINT('Ctrl Pts',(-9.68822500000012,-0.09891005009063,
26.8002376293806));
#16758=CARTESIAN_POINT('Ctrl Pts',(-9.688225,1.45372602844418E-12,26.7962631236951));
#16759=CARTESIAN_POINT('Ctrl Pts',(-9.688225,-1.28397292797899E-13,26.7537368763048));
#16760=CARTESIAN_POINT('Ctrl Pts',(-9.68822499999997,-0.298712821306256,
26.7657400630942));
#16761=CARTESIAN_POINT('Ctrl Pts',(-9.57054245632577,-0.595858078271711,
26.7777432498835));
#16762=CARTESIAN_POINT('Ctrl Pts',(-9.36601586214919,-0.813569405232887,
26.7897464366728));
#16763=CARTESIAN_POINT('Ctrl Pts',(-9.16148926797261,-1.03128073219406,
26.8017496234621));
#16764=CARTESIAN_POINT('Ctrl Pts',(-8.87226522412817,-1.16727314847146,
26.8137528102514));
#16765=CARTESIAN_POINT('Ctrl Pts',(-8.57413435701417,-1.18591009260192,
26.8257559970408));
#16766=CARTESIAN_POINT('Ctrl Pts',(-8.27600348990018,-1.20454703673238,
26.8377591838301));
#16767=CARTESIAN_POINT('Ctrl Pts',(-7.97209482032058,-1.10563290540093,
26.8497623706194));
#16768=CARTESIAN_POINT('Ctrl Pts',(-7.7420470537203,-0.915087963996314,
26.8617655574087));
#16769=CARTESIAN_POINT('Ctrl Pts',(-7.51199928712002,-0.724543022591697,
26.873768744198));
#16770=CARTESIAN_POINT('Ctrl Pts',(-7.35822688079616,-0.444367128061017,
26.8857719309874));
#16771=CARTESIAN_POINT('Ctrl Pts',(-7.32102560975811,-0.147979855989797,
26.8977751177767));
#16772=CARTESIAN_POINT('Ctrl Pts',(-7.28382433872006,0.148407416081424,
26.909778304566));
#16773=CARTESIAN_POINT('Ctrl Pts',(-7.36358464744657,0.457895344722506,
26.9217814913553));
#16774=CARTESIAN_POINT('Ctrl Pts',(-7.53940549437917,0.699383189958182,
26.9337846781446));
#16775=CARTESIAN_POINT('Ctrl Pts',(-7.71522634131177,0.940871035193858,
26.945787864934));
#16776=CARTESIAN_POINT('Ctrl Pts',(-7.98526240565846,1.11182427083112,26.9577910517233));
#16777=CARTESIAN_POINT('Ctrl Pts',(-8.27875123560185,1.1674449172776,26.9697942385126));
#16778=CARTESIAN_POINT('Ctrl Pts',(-8.57224006554525,1.22306556372407,26.9817974253019));
#16779=CARTESIAN_POINT('Ctrl Pts',(-8.88610136060016,1.16276985667,26.9938006120912));
#16780=CARTESIAN_POINT('Ctrl Pts',(-9.13808834820161,1.00235817476306,27.0058037988805));
#16781=CARTESIAN_POINT('Ctrl Pts',(-9.39007533580306,0.841946492856128,
27.0178069856699));
#16782=CARTESIAN_POINT('Ctrl Pts',(-9.5775432964218,0.583102430602135,27.0298101724592));
#16783=CARTESIAN_POINT('Ctrl Pts',(-9.65136659729213,0.293655596345351,
27.0418133592485));
#16784=CARTESIAN_POINT('Ctrl Pts',(-9.67581103310552,0.197813707971836,
27.045787864934));
#16785=CARTESIAN_POINT('Ctrl Pts',(-9.68822500000002,0.0989100500919358,
27.0497623706194));
#16786=CARTESIAN_POINT('Ctrl Pts',(-9.688225,-2.37920794177171E-13,27.0537368763048));
#16787=CARTESIAN_POINT('Origin',(-8.5,0.,1.8));
#16788=CARTESIAN_POINT('',(-9.688225,1.5049073098794E-12,27.3962631236951));
#16789=CARTESIAN_POINT('',(-9.688225,-2.12330153459561E-13,27.3537368763049));
#16790=CARTESIAN_POINT('',(-9.688225,-1.45515594291686E-16,1.8));
#16791=CARTESIAN_POINT('Ctrl Pts',(-9.688225,1.5049073098794E-12,27.3962631236951));
#16792=CARTESIAN_POINT('Ctrl Pts',(-9.68822499999962,0.298712821307587,
27.3842599369058));
#16793=CARTESIAN_POINT('Ctrl Pts',(-9.57054245632511,0.595858078272862,
27.3722567501165));
#16794=CARTESIAN_POINT('Ctrl Pts',(-9.36601586214834,0.813569405233792,
27.3602535633272));
#16795=CARTESIAN_POINT('Ctrl Pts',(-9.16148926797157,1.03128073219472,27.3482503765378));
#16796=CARTESIAN_POINT('Ctrl Pts',(-8.87226522412704,1.16727314847181,27.3362471897485));
#16797=CARTESIAN_POINT('Ctrl Pts',(-8.57413435701307,1.18591009260199,27.3242440029592));
#16798=CARTESIAN_POINT('Ctrl Pts',(-8.2760034898991,1.20454703673217,27.3122408161699));
#16799=CARTESIAN_POINT('Ctrl Pts',(-7.97209482031964,1.10563290540047,27.3002376293806));
#16800=CARTESIAN_POINT('Ctrl Pts',(-7.74204705371955,0.915087963995695,
27.2882344425913));
#16801=CARTESIAN_POINT('Ctrl Pts',(-7.51199928711946,0.724543022590918,
27.2762312558019));
#16802=CARTESIAN_POINT('Ctrl Pts',(-7.35822688079584,0.444367128060169,
27.2642280690126));
#16803=CARTESIAN_POINT('Ctrl Pts',(-7.321025609758,0.147979855988967,27.2522248822233));
#16804=CARTESIAN_POINT('Ctrl Pts',(-7.28382433872017,-0.148407416082235,
27.240221695434));
#16805=CARTESIAN_POINT('Ctrl Pts',(-7.36358464744687,-0.457895344723213,
27.2282185086447));
#16806=CARTESIAN_POINT('Ctrl Pts',(-7.53940549437959,-0.699383189958749,
27.2162153218554));
#16807=CARTESIAN_POINT('Ctrl Pts',(-7.7152263413123,-0.940871035194285,
27.204212135066));
#16808=CARTESIAN_POINT('Ctrl Pts',(-7.98526240565903,-1.11182427083137,
27.1922089482767));
#16809=CARTESIAN_POINT('Ctrl Pts',(-8.27875123560241,-1.1674449172777,27.1802057614874));
#16810=CARTESIAN_POINT('Ctrl Pts',(-8.57224006554578,-1.22306556372403,
27.1682025746981));
#16811=CARTESIAN_POINT('Ctrl Pts',(-8.88610136060062,-1.16276985666984,
27.1561993879088));
#16812=CARTESIAN_POINT('Ctrl Pts',(-9.13808834820197,-1.00235817476283,
27.1441962011195));
#16813=CARTESIAN_POINT('Ctrl Pts',(-9.39007533580333,-0.84194649285583,
27.1321930143301));
#16814=CARTESIAN_POINT('Ctrl Pts',(-9.57754329642195,-0.583102430601823,
27.1201898275408));
#16815=CARTESIAN_POINT('Ctrl Pts',(-9.6513665972922,-0.293655596345064,
27.1081866407515));
#16816=CARTESIAN_POINT('Ctrl Pts',(-9.67581103310566,-0.197813707971194,
27.104212135066));
#16817=CARTESIAN_POINT('Ctrl Pts',(-9.68822500000014,-0.0989100500909195,
27.1002376293806));
#16818=CARTESIAN_POINT('Ctrl Pts',(-9.688225,1.6144863224099E-12,27.0962631236951));
#16819=CARTESIAN_POINT('Ctrl Pts',(-9.688225,-2.37920794177171E-13,27.0537368763048));
#16820=CARTESIAN_POINT('Ctrl Pts',(-9.68822499999994,-0.29871282130632,
27.0657400630942));
#16821=CARTESIAN_POINT('Ctrl Pts',(-9.57054245632575,-0.595858078271721,
27.0777432498835));
#16822=CARTESIAN_POINT('Ctrl Pts',(-9.36601586214921,-0.813569405232868,
27.0897464366728));
#16823=CARTESIAN_POINT('Ctrl Pts',(-9.16148926797267,-1.03128073219402,
27.1017496234621));
#16824=CARTESIAN_POINT('Ctrl Pts',(-8.87226522412828,-1.16727314847141,
27.1137528102514));
#16825=CARTESIAN_POINT('Ctrl Pts',(-8.57413435701433,-1.18591009260191,
27.1257559970408));
#16826=CARTESIAN_POINT('Ctrl Pts',(-8.27600348990038,-1.20454703673241,
27.1377591838301));
#16827=CARTESIAN_POINT('Ctrl Pts',(-7.97209482032082,-1.10563290540103,
27.1497623706194));
#16828=CARTESIAN_POINT('Ctrl Pts',(-7.74204705372053,-0.915087963996503,
27.1617655574087));
#16829=CARTESIAN_POINT('Ctrl Pts',(-7.51199928712023,-0.724543022591972,
27.173768744198));
#16830=CARTESIAN_POINT('Ctrl Pts',(-7.35822688079631,-0.444367128061387,
27.1857719309873));
#16831=CARTESIAN_POINT('Ctrl Pts',(-7.32102560975816,-0.147979855990224,
27.1977751177767));
#16832=CARTESIAN_POINT('Ctrl Pts',(-7.28382433872001,0.148407416080939,
27.209778304566));
#16833=CARTESIAN_POINT('Ctrl Pts',(-7.36358464744638,0.457895344722001,
27.2217814913553));
#16834=CARTESIAN_POINT('Ctrl Pts',(-7.53940549437884,0.699383189957724,
27.2337846781446));
#16835=CARTESIAN_POINT('Ctrl Pts',(-7.7152263413113,0.940871035193448,27.2457878649339));
#16836=CARTESIAN_POINT('Ctrl Pts',(-7.98526240565785,1.11182427083082,27.2577910517232));
#16837=CARTESIAN_POINT('Ctrl Pts',(-8.27875123560116,1.16744491727747,27.2697942385126));
#16838=CARTESIAN_POINT('Ctrl Pts',(-8.57224006554448,1.22306556372411,27.2817974253019));
#16839=CARTESIAN_POINT('Ctrl Pts',(-8.88610136059938,1.16276985667025,27.2938006120912));
#16840=CARTESIAN_POINT('Ctrl Pts',(-9.1380883482009,1.00235817476351,27.3058037988805));
#16841=CARTESIAN_POINT('Ctrl Pts',(-9.39007533580243,0.841946492856779,
27.3178069856698));
#16842=CARTESIAN_POINT('Ctrl Pts',(-9.57754329642133,0.583102430602972,
27.3298101724592));
#16843=CARTESIAN_POINT('Ctrl Pts',(-9.65136659729189,0.293655596346292,
27.3418133592485));
#16844=CARTESIAN_POINT('Ctrl Pts',(-9.67581103310544,0.197813707972491,
27.3457878649339));
#16845=CARTESIAN_POINT('Ctrl Pts',(-9.68822500000002,0.0989100500922765,
27.3497623706194));
#16846=CARTESIAN_POINT('Ctrl Pts',(-9.688225,-2.12330153459561E-13,27.3537368763049));
#16847=CARTESIAN_POINT('Origin',(-8.5,0.,1.8));
#16848=CARTESIAN_POINT('',(-9.688225,1.53055346174824E-12,27.6962631236951));
#16849=CARTESIAN_POINT('',(-9.688225,-1.8668400159072E-13,27.6537368763048));
#16850=CARTESIAN_POINT('',(-9.688225,-1.45515594291686E-16,1.8));
#16851=CARTESIAN_POINT('Ctrl Pts',(-9.688225,1.53055346174824E-12,27.6962631236951));
#16852=CARTESIAN_POINT('Ctrl Pts',(-9.68822499999962,0.298712821307613,
27.6842599369058));
#16853=CARTESIAN_POINT('Ctrl Pts',(-9.5705424563251,0.595858078272886,27.6722567501165));
#16854=CARTESIAN_POINT('Ctrl Pts',(-9.36601586214832,0.81356940523381,27.6602535633272));
#16855=CARTESIAN_POINT('Ctrl Pts',(-9.16148926797154,1.03128073219474,27.6482503765378));
#16856=CARTESIAN_POINT('Ctrl Pts',(-8.87226522412701,1.16727314847182,27.6362471897485));
#16857=CARTESIAN_POINT('Ctrl Pts',(-8.57413435701304,1.18591009260199,27.6242440029592));
#16858=CARTESIAN_POINT('Ctrl Pts',(-8.27600348989907,1.20454703673217,27.6122408161699));
#16859=CARTESIAN_POINT('Ctrl Pts',(-7.97209482031962,1.10563290540046,27.6002376293806));
#16860=CARTESIAN_POINT('Ctrl Pts',(-7.74204705371953,0.915087963995678,
27.5882344425913));
#16861=CARTESIAN_POINT('Ctrl Pts',(-7.51199928711944,0.724543022590897,
27.5762312558019));
#16862=CARTESIAN_POINT('Ctrl Pts',(-7.35822688079583,0.444367128060145,
27.5642280690126));
#16863=CARTESIAN_POINT('Ctrl Pts',(-7.321025609758,0.147979855988942,27.5522248822233));
#16864=CARTESIAN_POINT('Ctrl Pts',(-7.28382433872017,-0.148407416082262,
27.540221695434));
#16865=CARTESIAN_POINT('Ctrl Pts',(-7.36358464744688,-0.457895344723237,
27.5282185086447));
#16866=CARTESIAN_POINT('Ctrl Pts',(-7.5394054943796,-0.699383189958769,
27.5162153218554));
#16867=CARTESIAN_POINT('Ctrl Pts',(-7.71522634131232,-0.940871035194301,
27.504212135066));
#16868=CARTESIAN_POINT('Ctrl Pts',(-7.98526240565906,-1.11182427083138,
27.4922089482767));
#16869=CARTESIAN_POINT('Ctrl Pts',(-8.27875123560243,-1.16744491727771,
27.4802057614874));
#16870=CARTESIAN_POINT('Ctrl Pts',(-8.57224006554581,-1.22306556372403,
27.4682025746981));
#16871=CARTESIAN_POINT('Ctrl Pts',(-8.88610136060064,-1.16276985666983,
27.4561993879088));
#16872=CARTESIAN_POINT('Ctrl Pts',(-9.138088348202,-1.00235817476282,27.4441962011195));
#16873=CARTESIAN_POINT('Ctrl Pts',(-9.39007533580335,-0.841946492855811,
27.4321930143301));
#16874=CARTESIAN_POINT('Ctrl Pts',(-9.57754329642196,-0.5831024306018,27.4201898275408));
#16875=CARTESIAN_POINT('Ctrl Pts',(-9.65136659729221,-0.293655596345039,
27.4081866407515));
#16876=CARTESIAN_POINT('Ctrl Pts',(-9.67581103310565,-0.197813707971212,
27.404212135066));
#16877=CARTESIAN_POINT('Ctrl Pts',(-9.68822500000013,-0.098910050090984,
27.4002376293806));
#16878=CARTESIAN_POINT('Ctrl Pts',(-9.688225,1.5049073098794E-12,27.3962631236951));
#16879=CARTESIAN_POINT('Ctrl Pts',(-9.688225,-2.12330153459561E-13,27.3537368763049));
#16880=CARTESIAN_POINT('Ctrl Pts',(-9.68822499999995,-0.298712821306295,
27.3657400630942));
#16881=CARTESIAN_POINT('Ctrl Pts',(-9.57054245632576,-0.595858078271698,
27.3777432498835));
#16882=CARTESIAN_POINT('Ctrl Pts',(-9.36601586214923,-0.813569405232849,
27.3897464366728));
#16883=CARTESIAN_POINT('Ctrl Pts',(-9.16148926797269,-1.031280732194,27.4017496234621));
#16884=CARTESIAN_POINT('Ctrl Pts',(-8.87226522412831,-1.1672731484714,27.4137528102514));
#16885=CARTESIAN_POINT('Ctrl Pts',(-8.57413435701436,-1.18591009260191,
27.4257559970408));
#16886=CARTESIAN_POINT('Ctrl Pts',(-8.27600348990041,-1.20454703673242,
27.4377591838301));
#16887=CARTESIAN_POINT('Ctrl Pts',(-7.97209482032084,-1.10563290540105,
27.4497623706194));
#16888=CARTESIAN_POINT('Ctrl Pts',(-7.74204705372055,-0.915087963996519,
27.4617655574087));
#16889=CARTESIAN_POINT('Ctrl Pts',(-7.51199928712025,-0.724543022591993,
27.473768744198));
#16890=CARTESIAN_POINT('Ctrl Pts',(-7.35822688079632,-0.444367128061411,
27.4857719309873));
#16891=CARTESIAN_POINT('Ctrl Pts',(-7.32102560975817,-0.14797985599025,
27.4977751177767));
#16892=CARTESIAN_POINT('Ctrl Pts',(-7.28382433872001,0.148407416080912,
27.509778304566));
#16893=CARTESIAN_POINT('Ctrl Pts',(-7.36358464744637,0.457895344721976,
27.5217814913553));
#16894=CARTESIAN_POINT('Ctrl Pts',(-7.53940549437883,0.699383189957703,
27.5337846781446));
#16895=CARTESIAN_POINT('Ctrl Pts',(-7.71522634131128,0.940871035193431,
27.5457878649339));
#16896=CARTESIAN_POINT('Ctrl Pts',(-7.98526240565782,1.11182427083081,27.5577910517232));
#16897=CARTESIAN_POINT('Ctrl Pts',(-8.27875123560114,1.16744491727746,27.5697942385126));
#16898=CARTESIAN_POINT('Ctrl Pts',(-8.57224006554445,1.22306556372411,27.5817974253019));
#16899=CARTESIAN_POINT('Ctrl Pts',(-8.88610136059935,1.16276985667026,27.5938006120912));
#16900=CARTESIAN_POINT('Ctrl Pts',(-9.13808834820088,1.00235817476353,27.6058037988805));
#16901=CARTESIAN_POINT('Ctrl Pts',(-9.39007533580241,0.841946492856798,
27.6178069856698));
#16902=CARTESIAN_POINT('Ctrl Pts',(-9.57754329642132,0.583102430602995,
27.6298101724592));
#16903=CARTESIAN_POINT('Ctrl Pts',(-9.65136659729188,0.293655596346317,
27.6418133592485));
#16904=CARTESIAN_POINT('Ctrl Pts',(-9.67581103310542,0.19781370797256,27.6457878649339));
#16905=CARTESIAN_POINT('Ctrl Pts',(-9.688225,0.0989100500923923,27.6497623706194));
#16906=CARTESIAN_POINT('Ctrl Pts',(-9.688225,-5.15698594938385E-14,27.6537368763048));
#16907=CARTESIAN_POINT('Origin',(-8.5,0.,1.8));
#16908=CARTESIAN_POINT('',(-9.688225,1.55619961361708E-12,27.9962631236951));
#16909=CARTESIAN_POINT('',(-9.688225,-1.61037849721879E-13,27.9537368763048));
#16910=CARTESIAN_POINT('',(-9.688225,-1.45515594291686E-16,1.8));
#16911=CARTESIAN_POINT('Ctrl Pts',(-9.688225,1.55619961361708E-12,27.9962631236951));
#16912=CARTESIAN_POINT('Ctrl Pts',(-9.68822499999961,0.298712821307638,
27.9842599369058));
#16913=CARTESIAN_POINT('Ctrl Pts',(-9.57054245632509,0.595858078272909,
27.9722567501165));
#16914=CARTESIAN_POINT('Ctrl Pts',(-9.36601586214831,0.813569405233829,
27.9602535633272));
#16915=CARTESIAN_POINT('Ctrl Pts',(-9.16148926797152,1.03128073219475,27.9482503765378));
#16916=CARTESIAN_POINT('Ctrl Pts',(-8.87226522412699,1.16727314847182,27.9362471897485));
#16917=CARTESIAN_POINT('Ctrl Pts',(-8.57413435701302,1.18591009260199,27.9242440029592));
#16918=CARTESIAN_POINT('Ctrl Pts',(-8.27600348989905,1.20454703673216,27.9122408161699));
#16919=CARTESIAN_POINT('Ctrl Pts',(-7.97209482031959,1.10563290540045,27.9002376293806));
#16920=CARTESIAN_POINT('Ctrl Pts',(-7.74204705371951,0.915087963995662,
27.8882344425913));
#16921=CARTESIAN_POINT('Ctrl Pts',(-7.51199928711943,0.724543022590876,
27.8762312558019));
#16922=CARTESIAN_POINT('Ctrl Pts',(-7.35822688079582,0.44436712806012,27.8642280690126));
#16923=CARTESIAN_POINT('Ctrl Pts',(-7.321025609758,0.147979855988916,27.8522248822233));
#16924=CARTESIAN_POINT('Ctrl Pts',(-7.28382433872017,-0.148407416082288,
27.840221695434));
#16925=CARTESIAN_POINT('Ctrl Pts',(-7.36358464744689,-0.457895344723262,
27.8282185086447));
#16926=CARTESIAN_POINT('Ctrl Pts',(-7.53940549437962,-0.69938318995879,
27.8162153218554));
#16927=CARTESIAN_POINT('Ctrl Pts',(-7.71522634131234,-0.940871035194318,
27.804212135066));
#16928=CARTESIAN_POINT('Ctrl Pts',(-7.98526240565908,-1.1118242708314,27.7922089482767));
#16929=CARTESIAN_POINT('Ctrl Pts',(-8.27875123560246,-1.16744491727771,
27.7802057614874));
#16930=CARTESIAN_POINT('Ctrl Pts',(-8.57224006554584,-1.22306556372403,
27.7682025746981));
#16931=CARTESIAN_POINT('Ctrl Pts',(-8.88610136060067,-1.16276985666982,
27.7561993879088));
#16932=CARTESIAN_POINT('Ctrl Pts',(-9.13808834820202,-1.00235817476281,
27.7441962011195));
#16933=CARTESIAN_POINT('Ctrl Pts',(-9.39007533580337,-0.841946492855791,
27.7321930143301));
#16934=CARTESIAN_POINT('Ctrl Pts',(-9.57754329642198,-0.583102430601777,
27.7201898275408));
#16935=CARTESIAN_POINT('Ctrl Pts',(-9.65136659729222,-0.293655596345015,
27.7081866407515));
#16936=CARTESIAN_POINT('Ctrl Pts',(-9.67581103310565,-0.197813707971187,
27.704212135066));
#16937=CARTESIAN_POINT('Ctrl Pts',(-9.68822500000013,-0.0989100500909583,
27.7002376293806));
#16938=CARTESIAN_POINT('Ctrl Pts',(-9.688225,1.53055346174824E-12,27.6962631236951));
#16939=CARTESIAN_POINT('Ctrl Pts',(-9.688225,-5.15698594938385E-14,27.6537368763048));
#16940=CARTESIAN_POINT('Ctrl Pts',(-9.68822499999999,-0.298712821306134,
27.6657400630942));
#16941=CARTESIAN_POINT('Ctrl Pts',(-9.57054245632584,-0.595858078271553,
27.6777432498835));
#16942=CARTESIAN_POINT('Ctrl Pts',(-9.36601586214934,-0.813569405232732,
27.6897464366728));
#16943=CARTESIAN_POINT('Ctrl Pts',(-9.16148926797283,-1.03128073219391,
27.7017496234621));
#16944=CARTESIAN_POINT('Ctrl Pts',(-8.87226522412847,-1.16727314847135,
27.7137528102514));
#16945=CARTESIAN_POINT('Ctrl Pts',(-8.57413435701452,-1.1859100926019,27.7257559970407));
#16946=CARTESIAN_POINT('Ctrl Pts',(-8.27600348990057,-1.20454703673245,
27.7377591838301));
#16947=CARTESIAN_POINT('Ctrl Pts',(-7.97209482032099,-1.10563290540112,
27.7497623706194));
#16948=CARTESIAN_POINT('Ctrl Pts',(-7.74204705372067,-0.915087963996622,
27.7617655574087));
#16949=CARTESIAN_POINT('Ctrl Pts',(-7.51199928712035,-0.724543022592127,
27.773768744198));
#16950=CARTESIAN_POINT('Ctrl Pts',(-7.35822688079638,-0.444367128061566,
27.7857719309873));
#16951=CARTESIAN_POINT('Ctrl Pts',(-7.32102560975819,-0.147979855990409,
27.7977751177767));
#16952=CARTESIAN_POINT('Ctrl Pts',(-7.28382433871999,0.148407416080748,
27.809778304566));
#16953=CARTESIAN_POINT('Ctrl Pts',(-7.36358464744631,0.457895344721823,
27.8217814913553));
#16954=CARTESIAN_POINT('Ctrl Pts',(-7.53940549437873,0.699383189957574,
27.8337846781446));
#16955=CARTESIAN_POINT('Ctrl Pts',(-7.71522634131115,0.940871035193324,
27.8457878649339));
#16956=CARTESIAN_POINT('Ctrl Pts',(-7.98526240565767,1.11182427083074,27.8577910517232));
#16957=CARTESIAN_POINT('Ctrl Pts',(-8.27875123560098,1.16744491727743,27.8697942385126));
#16958=CARTESIAN_POINT('Ctrl Pts',(-8.57224006554429,1.22306556372412,27.8817974253019));
#16959=CARTESIAN_POINT('Ctrl Pts',(-8.88610136059919,1.16276985667031,27.8938006120912));
#16960=CARTESIAN_POINT('Ctrl Pts',(-9.13808834820075,1.00235817476361,27.9058037988805));
#16961=CARTESIAN_POINT('Ctrl Pts',(-9.3900753358023,0.841946492856918,27.9178069856698));
#16962=CARTESIAN_POINT('Ctrl Pts',(-9.57754329642124,0.583102430603141,
27.9298101724591));
#16963=CARTESIAN_POINT('Ctrl Pts',(-9.65136659729184,0.293655596346473,
27.9418133592485));
#16964=CARTESIAN_POINT('Ctrl Pts',(-9.67581103310542,0.197813707972632,
27.9457878649339));
#16965=CARTESIAN_POINT('Ctrl Pts',(-9.68822500000001,0.0989100500923729,
27.9497623706194));
#16966=CARTESIAN_POINT('Ctrl Pts',(-9.688225,-1.61037849721879E-13,27.9537368763048));
#16967=CARTESIAN_POINT('Origin',(-8.5,0.,1.8));
#16968=CARTESIAN_POINT('',(-9.688225,1.58184576548592E-12,28.2962631236951));
#16969=CARTESIAN_POINT('',(-9.688225,-1.35447209004269E-13,28.2537368763048));
#16970=CARTESIAN_POINT('',(-9.688225,-1.45515594291686E-16,1.8));
#16971=CARTESIAN_POINT('Ctrl Pts',(-9.688225,1.71684888528034E-12,28.2962631236951));
#16972=CARTESIAN_POINT('Ctrl Pts',(-9.68822499999957,0.298712821307844,
28.2842599369058));
#16973=CARTESIAN_POINT('Ctrl Pts',(-9.57054245632497,0.595858078273142,
28.2722567501165));
#16974=CARTESIAN_POINT('Ctrl Pts',(-9.3660158621481,0.813569405234045,28.2602535633272));
#16975=CARTESIAN_POINT('Ctrl Pts',(-9.16148926797123,1.03128073219495,28.2482503765378));
#16976=CARTESIAN_POINT('Ctrl Pts',(-8.87226522412661,1.16727314847196,28.2362471897485));
#16977=CARTESIAN_POINT('Ctrl Pts',(-8.57413435701259,1.18591009260202,28.2242440029592));
#16978=CARTESIAN_POINT('Ctrl Pts',(-8.27600348989856,1.20454703673208,28.2122408161699));
#16979=CARTESIAN_POINT('Ctrl Pts',(-7.9720948203191,1.10563290540023,28.2002376293806));
#16980=CARTESIAN_POINT('Ctrl Pts',(-7.74204705371907,0.915087963995301,
28.1882344425912));
#16981=CARTESIAN_POINT('Ctrl Pts',(-7.51199928711905,0.724543022590376,
28.1762312558019));
#16982=CARTESIAN_POINT('Ctrl Pts',(-7.35822688079556,0.444367128059491,
28.1642280690126));
#16983=CARTESIAN_POINT('Ctrl Pts',(-7.32102560975791,0.147979855988221,
28.1522248822233));
#16984=CARTESIAN_POINT('Ctrl Pts',(-7.28382433872026,-0.14840741608305,
28.140221695434));
#16985=CARTESIAN_POINT('Ctrl Pts',(-7.36358464744719,-0.457895344724025,
28.1282185086446));
#16986=CARTESIAN_POINT('Ctrl Pts',(-7.53940549438011,-0.699383189959466,
28.1162153218553));
#16987=CARTESIAN_POINT('Ctrl Pts',(-7.71522634131303,-0.940871035194907,
28.104212135066));
#16988=CARTESIAN_POINT('Ctrl Pts',(-7.98526240565995,-1.11182427083181,
28.0922089482767));
#16989=CARTESIAN_POINT('Ctrl Pts',(-8.27875123560341,-1.16744491727789,
28.0802057614874));
#16990=CARTESIAN_POINT('Ctrl Pts',(-8.57224006554688,-1.22306556372398,
28.068202574698));
#16991=CARTESIAN_POINT('Ctrl Pts',(-8.88610136060171,-1.16276985666948,
28.0561993879087));
#16992=CARTESIAN_POINT('Ctrl Pts',(-9.13808834820295,-1.00235817476221,
28.0441962011194));
#16993=CARTESIAN_POINT('Ctrl Pts',(-9.39007533580419,-0.841946492854939,
28.0321930143301));
#16994=CARTESIAN_POINT('Ctrl Pts',(-9.57754329642258,-0.583102430600695,
28.0201898275408));
#16995=CARTESIAN_POINT('Ctrl Pts',(-9.65136659729252,-0.293655596343812,
28.0081866407515));
#16996=CARTESIAN_POINT('Ctrl Pts',(-9.67581103310576,-0.197813707970351,
28.004212135066));
#16997=CARTESIAN_POINT('Ctrl Pts',(-9.68822500000013,-0.0989100500905275,
28.0002376293806));
#16998=CARTESIAN_POINT('Ctrl Pts',(-9.688225,1.55619961361708E-12,27.9962631236951));
#16999=CARTESIAN_POINT('Ctrl Pts',(-9.688225,-1.61037849721879E-13,27.9537368763048));
#17000=CARTESIAN_POINT('Ctrl Pts',(-9.68822499999996,-0.298712821306243,
27.9657400630942));
#17001=CARTESIAN_POINT('Ctrl Pts',(-9.57054245632579,-0.595858078271651,
27.9777432498835));
#17002=CARTESIAN_POINT('Ctrl Pts',(-9.36601586214926,-0.813569405232812,
27.9897464366728));
#17003=CARTESIAN_POINT('Ctrl Pts',(-9.16148926797273,-1.03128073219397,
28.0017496234621));
#17004=CARTESIAN_POINT('Ctrl Pts',(-8.87226522412836,-1.16727314847139,
28.0137528102514));
#17005=CARTESIAN_POINT('Ctrl Pts',(-8.57413435701441,-1.18591009260191,
28.0257559970408));
#17006=CARTESIAN_POINT('Ctrl Pts',(-8.27600348990046,-1.20454703673243,
28.0377591838301));
#17007=CARTESIAN_POINT('Ctrl Pts',(-7.97209482032089,-1.10563290540107,
28.0497623706194));
#17008=CARTESIAN_POINT('Ctrl Pts',(-7.74204705372058,-0.915087963996552,
28.0617655574087));
#17009=CARTESIAN_POINT('Ctrl Pts',(-7.51199928712028,-0.724543022592035,
28.073768744198));
#17010=CARTESIAN_POINT('Ctrl Pts',(-7.35822688079634,-0.444367128061461,
28.0857719309873));
#17011=CARTESIAN_POINT('Ctrl Pts',(-7.32102560975817,-0.1479798559903,28.0977751177767));
#17012=CARTESIAN_POINT('Ctrl Pts',(-7.28382433872,0.14840741608086,28.109778304566));
#17013=CARTESIAN_POINT('Ctrl Pts',(-7.36358464744635,0.457895344721927,
28.1217814913553));
#17014=CARTESIAN_POINT('Ctrl Pts',(-7.5394054943788,0.699383189957662,28.1337846781446));
#17015=CARTESIAN_POINT('Ctrl Pts',(-7.71522634131124,0.940871035193397,
28.1457878649339));
#17016=CARTESIAN_POINT('Ctrl Pts',(-7.98526240565778,1.11182427083079,28.1577910517232));
#17017=CARTESIAN_POINT('Ctrl Pts',(-8.27875123560109,1.16744491727745,28.1697942385126));
#17018=CARTESIAN_POINT('Ctrl Pts',(-8.5722400655444,1.22306556372411,28.1817974253019));
#17019=CARTESIAN_POINT('Ctrl Pts',(-8.8861013605993,1.16276985667027,28.1938006120912));
#17020=CARTESIAN_POINT('Ctrl Pts',(-9.13808834820084,1.00235817476355,28.2058037988805));
#17021=CARTESIAN_POINT('Ctrl Pts',(-9.39007533580238,0.841946492856836,
28.2178069856698));
#17022=CARTESIAN_POINT('Ctrl Pts',(-9.57754329642129,0.583102430603042,
28.2298101724591));
#17023=CARTESIAN_POINT('Ctrl Pts',(-9.65136659729187,0.293655596346366,
28.2418133592485));
#17024=CARTESIAN_POINT('Ctrl Pts',(-9.67581103310542,0.197813707972567,
28.2457878649339));
#17025=CARTESIAN_POINT('Ctrl Pts',(-9.68822500000001,0.0989100500923534,
28.2497623706194));
#17026=CARTESIAN_POINT('Ctrl Pts',(-9.688225,-1.35447209004269E-13,28.2537368763048));
#17027=CARTESIAN_POINT('Origin',(-8.5,0.,1.8));
#17028=CARTESIAN_POINT('',(-9.688225,1.6073808950523E-12,28.5962631236951));
#17029=CARTESIAN_POINT('',(-9.688225,-1.09801057135428E-13,28.5537368763048));
#17030=CARTESIAN_POINT('',(-9.688225,-1.45515594291686E-16,1.8));
#17031=CARTESIAN_POINT('Ctrl Pts',(-9.688225,1.74249503714918E-12,28.5962631236951));
#17032=CARTESIAN_POINT('Ctrl Pts',(-9.68822499999956,0.29871282130778,28.5842599369058));
#17033=CARTESIAN_POINT('Ctrl Pts',(-9.57054245632503,0.595858078272988,
28.5722567501165));
#17034=CARTESIAN_POINT('Ctrl Pts',(-9.36601586214827,0.813569405233866,
28.5602535633272));
#17035=CARTESIAN_POINT('Ctrl Pts',(-9.16148926797151,1.03128073219475,28.5482503765379));
#17036=CARTESIAN_POINT('Ctrl Pts',(-8.87226522412703,1.1672731484718,28.5362471897485));
#17037=CARTESIAN_POINT('Ctrl Pts',(-8.5741343570131,1.18591009260199,28.5242440029592));
#17038=CARTESIAN_POINT('Ctrl Pts',(-8.27600348989918,1.20454703673218,28.5122408161699));
#17039=CARTESIAN_POINT('Ctrl Pts',(-7.97209482031976,1.10563290540052,28.5002376293806));
#17040=CARTESIAN_POINT('Ctrl Pts',(-7.74204705371968,0.915087963995802,
28.4882344425913));
#17041=CARTESIAN_POINT('Ctrl Pts',(-7.5119992871196,0.724543022591086,28.476231255802));
#17042=CARTESIAN_POINT('Ctrl Pts',(-7.35822688079595,0.444367128060416,
28.4642280690126));
#17043=CARTESIAN_POINT('Ctrl Pts',(-7.32102560975804,0.147979855989267,
28.4522248822233));
#17044=CARTESIAN_POINT('Ctrl Pts',(-7.28382433872014,-0.148407416081881,
28.440221695434));
#17045=CARTESIAN_POINT('Ctrl Pts',(-7.36358464744673,-0.45789534472283,
28.4282185086447));
#17046=CARTESIAN_POINT('Ctrl Pts',(-7.53940549437933,-0.699383189958395,
28.4162153218554));
#17047=CARTESIAN_POINT('Ctrl Pts',(-7.71522634131193,-0.940871035193959,
28.4042121350661));
#17048=CARTESIAN_POINT('Ctrl Pts',(-7.98526240565854,-1.11182427083113,
28.3922089482767));
#17049=CARTESIAN_POINT('Ctrl Pts',(-8.27875123560185,-1.1674449172776,28.3802057614874));
#17050=CARTESIAN_POINT('Ctrl Pts',(-8.57224006554515,-1.22306556372406,
28.3682025746981));
#17051=CARTESIAN_POINT('Ctrl Pts',(-8.88610136059996,-1.16276985667004,
28.3561993879088));
#17052=CARTESIAN_POINT('Ctrl Pts',(-9.13808834820138,-1.00235817476321,
28.3441962011195));
#17053=CARTESIAN_POINT('Ctrl Pts',(-9.39007533580279,-0.841946492856384,
28.3321930143302));
#17054=CARTESIAN_POINT('Ctrl Pts',(-9.57754329642155,-0.583102430602544,
28.3201898275409));
#17055=CARTESIAN_POINT('Ctrl Pts',(-9.65136659729199,-0.293655596345881,
28.3081866407515));
#17056=CARTESIAN_POINT('Ctrl Pts',(-9.6758110331056,-0.197813707971723,
28.3042121350661));
#17057=CARTESIAN_POINT('Ctrl Pts',(-9.68822500000014,-0.0989100500911323,
28.3002376293806));
#17058=CARTESIAN_POINT('Ctrl Pts',(-9.688225,1.71684888528034E-12,28.2962631236951));
#17059=CARTESIAN_POINT('Ctrl Pts',(-9.688225,-1.35447209004269E-13,28.2537368763048));
#17060=CARTESIAN_POINT('Ctrl Pts',(-9.68822499999997,-0.298712821306263,
28.2657400630942));
#17061=CARTESIAN_POINT('Ctrl Pts',(-9.57054245632576,-0.595858078271717,
28.2777432498835));
#17062=CARTESIAN_POINT('Ctrl Pts',(-9.36601586214919,-0.813569405232892,
28.2897464366728));
#17063=CARTESIAN_POINT('Ctrl Pts',(-9.16148926797261,-1.03128073219407,
28.3017496234621));
#17064=CARTESIAN_POINT('Ctrl Pts',(-8.87226522412817,-1.16727314847146,
28.3137528102514));
#17065=CARTESIAN_POINT('Ctrl Pts',(-8.57413435701417,-1.18591009260192,
28.3257559970408));
#17066=CARTESIAN_POINT('Ctrl Pts',(-8.27600348990017,-1.20454703673238,
28.3377591838301));
#17067=CARTESIAN_POINT('Ctrl Pts',(-7.97209482032057,-1.10563290540093,
28.3497623706194));
#17068=CARTESIAN_POINT('Ctrl Pts',(-7.74204705372029,-0.91508796399631,
28.3617655574087));
#17069=CARTESIAN_POINT('Ctrl Pts',(-7.51199928712001,-0.724543022591691,
28.373768744198));
#17070=CARTESIAN_POINT('Ctrl Pts',(-7.35822688079616,-0.444367128061011,
28.3857719309874));
#17071=CARTESIAN_POINT('Ctrl Pts',(-7.32102560975811,-0.14797985598979,
28.3977751177767));
#17072=CARTESIAN_POINT('Ctrl Pts',(-7.28382433872006,0.148407416081431,
28.409778304566));
#17073=CARTESIAN_POINT('Ctrl Pts',(-7.36358464744658,0.457895344722512,
28.4217814913553));
#17074=CARTESIAN_POINT('Ctrl Pts',(-7.53940549437918,0.699383189958187,
28.4337846781446));
#17075=CARTESIAN_POINT('Ctrl Pts',(-7.71522634131178,0.940871035193862,
28.445787864934));
#17076=CARTESIAN_POINT('Ctrl Pts',(-7.98526240565847,1.11182427083112,28.4577910517233));
#17077=CARTESIAN_POINT('Ctrl Pts',(-8.27875123560186,1.1674449172776,28.4697942385126));
#17078=CARTESIAN_POINT('Ctrl Pts',(-8.57224006554525,1.22306556372407,28.4817974253019));
#17079=CARTESIAN_POINT('Ctrl Pts',(-8.88610136060016,1.16276985667,28.4938006120912));
#17080=CARTESIAN_POINT('Ctrl Pts',(-9.13808834820161,1.00235817476306,28.5058037988805));
#17081=CARTESIAN_POINT('Ctrl Pts',(-9.39007533580306,0.841946492856123,
28.5178069856699));
#17082=CARTESIAN_POINT('Ctrl Pts',(-9.5775432964218,0.583102430602129,28.5298101724592));
#17083=CARTESIAN_POINT('Ctrl Pts',(-9.65136659729213,0.293655596345344,
28.5418133592485));
#17084=CARTESIAN_POINT('Ctrl Pts',(-9.67581103310551,0.197813707971872,
28.545787864934));
#17085=CARTESIAN_POINT('Ctrl Pts',(-9.68822500000001,0.0989100500920189,
28.5497623706194));
#17086=CARTESIAN_POINT('Ctrl Pts',(-9.688225,-1.09801057135428E-13,28.5537368763048));
#17087=CARTESIAN_POINT('Origin',(-8.5,0.,1.8));
#17088=CARTESIAN_POINT('',(-9.688225,1.63313806922361E-12,28.8962631236951));
#17089=CARTESIAN_POINT('',(-9.688225,-8.42104164178181E-14,28.8537368763048));
#17090=CARTESIAN_POINT('',(-9.688225,-1.45515594291686E-16,1.8));
#17091=CARTESIAN_POINT('Ctrl Pts',(-9.688225,1.63313806922361E-12,28.8962631236951));
#17092=CARTESIAN_POINT('Ctrl Pts',(-9.68822499999959,0.29871282130767,28.8842599369058));
#17093=CARTESIAN_POINT('Ctrl Pts',(-9.57054245632509,0.595858078272889,
28.8722567501165));
#17094=CARTESIAN_POINT('Ctrl Pts',(-9.36601586214835,0.813569405233787,
28.8602535633272));
#17095=CARTESIAN_POINT('Ctrl Pts',(-9.16148926797161,1.03128073219468,28.8482503765379));
#17096=CARTESIAN_POINT('Ctrl Pts',(-8.87226522412713,1.16727314847177,28.8362471897485));
#17097=CARTESIAN_POINT('Ctrl Pts',(-8.57413435701321,1.18591009260198,28.8242440029592));
#17098=CARTESIAN_POINT('Ctrl Pts',(-8.27600348989929,1.2045470367322,28.8122408161699));
#17099=CARTESIAN_POINT('Ctrl Pts',(-7.97209482031986,1.10563290540057,28.8002376293806));
#17100=CARTESIAN_POINT('Ctrl Pts',(-7.74204705371976,0.915087963995872,
28.7882344425913));
#17101=CARTESIAN_POINT('Ctrl Pts',(-7.51199928711966,0.724543022591177,
28.776231255802));
#17102=CARTESIAN_POINT('Ctrl Pts',(-7.35822688079599,0.444367128060521,
28.7642280690126));
#17103=CARTESIAN_POINT('Ctrl Pts',(-7.32102560975806,0.147979855989376,
28.7522248822233));
#17104=CARTESIAN_POINT('Ctrl Pts',(-7.28382433872012,-0.148407416081769,
28.740221695434));
#17105=CARTESIAN_POINT('Ctrl Pts',(-7.36358464744669,-0.457895344722725,
28.7282185086447));
#17106=CARTESIAN_POINT('Ctrl Pts',(-7.53940549437926,-0.699383189958306,
28.7162153218554));
#17107=CARTESIAN_POINT('Ctrl Pts',(-7.71522634131184,-0.940871035193887,
28.7042121350661));
#17108=CARTESIAN_POINT('Ctrl Pts',(-7.98526240565844,-1.11182427083109,
28.6922089482768));
#17109=CARTESIAN_POINT('Ctrl Pts',(-8.27875123560174,-1.16744491727757,
28.6802057614874));
#17110=CARTESIAN_POINT('Ctrl Pts',(-8.57224006554504,-1.22306556372406,
28.6682025746981));
#17111=CARTESIAN_POINT('Ctrl Pts',(-8.88610136059985,-1.16276985667008,
28.6561993879088));
#17112=CARTESIAN_POINT('Ctrl Pts',(-9.13808834820128,-1.00235817476327,
28.6441962011195));
#17113=CARTESIAN_POINT('Ctrl Pts',(-9.39007533580271,-0.841946492856467,
28.6321930143302));
#17114=CARTESIAN_POINT('Ctrl Pts',(-9.5775432964215,-0.583102430602644,
28.6201898275409));
#17115=CARTESIAN_POINT('Ctrl Pts',(-9.65136659729197,-0.293655596345987,
28.6081866407515));
#17116=CARTESIAN_POINT('Ctrl Pts',(-9.67581103310559,-0.197813707971787,
28.6042121350661));
#17117=CARTESIAN_POINT('Ctrl Pts',(-9.68822500000015,-0.0989100500911517,
28.6002376293806));
#17118=CARTESIAN_POINT('Ctrl Pts',(-9.688225,1.74249503714918E-12,28.5962631236951));
#17119=CARTESIAN_POINT('Ctrl Pts',(-9.688225,-1.09801057135428E-13,28.5537368763048));
#17120=CARTESIAN_POINT('Ctrl Pts',(-9.68822499999997,-0.298712821306192,
28.5657400630942));
#17121=CARTESIAN_POINT('Ctrl Pts',(-9.57054245632581,-0.595858078271605,
28.5777432498835));
#17122=CARTESIAN_POINT('Ctrl Pts',(-9.3660158621493,-0.813569405232775,
28.5897464366728));
#17123=CARTESIAN_POINT('Ctrl Pts',(-9.16148926797278,-1.03128073219394,
28.6017496234621));
#17124=CARTESIAN_POINT('Ctrl Pts',(-8.87226522412841,-1.16727314847137,
28.6137528102514));
#17125=CARTESIAN_POINT('Ctrl Pts',(-8.57413435701446,-1.1859100926019,28.6257559970408));
#17126=CARTESIAN_POINT('Ctrl Pts',(-8.27600348990051,-1.20454703673244,
28.6377591838301));
#17127=CARTESIAN_POINT('Ctrl Pts',(-7.97209482032094,-1.10563290540109,
28.6497623706194));
#17128=CARTESIAN_POINT('Ctrl Pts',(-7.74204705372062,-0.915087963996584,
28.6617655574087));
#17129=CARTESIAN_POINT('Ctrl Pts',(-7.51199928712031,-0.724543022592078,
28.673768744198));
#17130=CARTESIAN_POINT('Ctrl Pts',(-7.35822688079636,-0.44436712806151,
28.6857719309873));
#17131=CARTESIAN_POINT('Ctrl Pts',(-7.32102560975818,-0.147979855990351,
28.6977751177767));
#17132=CARTESIAN_POINT('Ctrl Pts',(-7.28382433872,0.148407416080807,28.709778304566));
#17133=CARTESIAN_POINT('Ctrl Pts',(-7.36358464744633,0.457895344721878,
28.7217814913553));
#17134=CARTESIAN_POINT('Ctrl Pts',(-7.53940549437877,0.699383189957621,
28.7337846781446));
#17135=CARTESIAN_POINT('Ctrl Pts',(-7.7152263413112,0.940871035193363,28.7457878649339));
#17136=CARTESIAN_POINT('Ctrl Pts',(-7.98526240565773,1.11182427083077,28.7577910517232));
#17137=CARTESIAN_POINT('Ctrl Pts',(-8.27875123560104,1.16744491727744,28.7697942385126));
#17138=CARTESIAN_POINT('Ctrl Pts',(-8.57224006554435,1.22306556372412,28.7817974253019));
#17139=CARTESIAN_POINT('Ctrl Pts',(-8.88610136059925,1.16276985667029,28.7938006120912));
#17140=CARTESIAN_POINT('Ctrl Pts',(-9.1380883482008,1.00235817476358,28.8058037988805));
#17141=CARTESIAN_POINT('Ctrl Pts',(-9.39007533580234,0.841946492856875,
28.8178069856698));
#17142=CARTESIAN_POINT('Ctrl Pts',(-9.57754329642127,0.583102430603088,
28.8298101724591));
#17143=CARTESIAN_POINT('Ctrl Pts',(-9.65136659729186,0.293655596346416,
28.8418133592485));
#17144=CARTESIAN_POINT('Ctrl Pts',(-9.67581103310541,0.197813707972618,
28.8457878649339));
#17145=CARTESIAN_POINT('Ctrl Pts',(-9.68822500000001,0.0989100500924047,
28.8497623706194));
#17146=CARTESIAN_POINT('Ctrl Pts',(-9.688225,-8.42104164178181E-14,28.8537368763048));
#17147=CARTESIAN_POINT('Origin',(-8.5,0.,1.8));
#17148=CARTESIAN_POINT('',(-9.688225,1.65867319878998E-12,29.1962631236951));
#17149=CARTESIAN_POINT('',(-9.688225,-5.8564264548977E-14,29.1537368763048));
#17150=CARTESIAN_POINT('',(-9.688225,-1.45515594291686E-16,1.8));
#17151=CARTESIAN_POINT('Ctrl Pts',(-9.688225,1.65867319878998E-12,29.1962631236951));
#17152=CARTESIAN_POINT('Ctrl Pts',(-9.68822499999958,0.298712821307696,
29.1842599369058));
#17153=CARTESIAN_POINT('Ctrl Pts',(-9.57054245632508,0.595858078272912,
29.1722567501165));
#17154=CARTESIAN_POINT('Ctrl Pts',(-9.36601586214833,0.813569405233805,
29.1602535633272));
#17155=CARTESIAN_POINT('Ctrl Pts',(-9.16148926797158,1.0312807321947,29.1482503765379));
#17156=CARTESIAN_POINT('Ctrl Pts',(-8.87226522412711,1.16727314847177,29.1362471897485));
#17157=CARTESIAN_POINT('Ctrl Pts',(-8.57413435701319,1.18591009260198,29.1242440029592));
#17158=CARTESIAN_POINT('Ctrl Pts',(-8.27600348989926,1.20454703673219,29.1122408161699));
#17159=CARTESIAN_POINT('Ctrl Pts',(-7.97209482031984,1.10563290540055,29.1002376293806));
#17160=CARTESIAN_POINT('Ctrl Pts',(-7.74204705371974,0.915087963995855,
29.0882344425913));
#17161=CARTESIAN_POINT('Ctrl Pts',(-7.51199928711965,0.724543022591156,
29.076231255802));
#17162=CARTESIAN_POINT('Ctrl Pts',(-7.35822688079598,0.444367128060496,
29.0642280690126));
#17163=CARTESIAN_POINT('Ctrl Pts',(-7.32102560975805,0.147979855989351,
29.0522248822233));
#17164=CARTESIAN_POINT('Ctrl Pts',(-7.28382433872013,-0.148407416081795,
29.040221695434));
#17165=CARTESIAN_POINT('Ctrl Pts',(-7.3635846474467,-0.45789534472275,29.0282185086447));
#17166=CARTESIAN_POINT('Ctrl Pts',(-7.53940549437928,-0.699383189958327,
29.0162153218554));
#17167=CARTESIAN_POINT('Ctrl Pts',(-7.71522634131186,-0.940871035193904,
29.0042121350661));
#17168=CARTESIAN_POINT('Ctrl Pts',(-7.98526240565846,-1.1118242708311,28.9922089482767));
#17169=CARTESIAN_POINT('Ctrl Pts',(-8.27875123560176,-1.16744491727758,
28.9802057614874));
#17170=CARTESIAN_POINT('Ctrl Pts',(-8.57224006554507,-1.22306556372406,
28.9682025746981));
#17171=CARTESIAN_POINT('Ctrl Pts',(-8.88610136059988,-1.16276985667007,
28.9561993879088));
#17172=CARTESIAN_POINT('Ctrl Pts',(-9.1380883482013,-1.00235817476326,28.9441962011195));
#17173=CARTESIAN_POINT('Ctrl Pts',(-9.39007533580273,-0.841946492856447,
28.9321930143302));
#17174=CARTESIAN_POINT('Ctrl Pts',(-9.57754329642151,-0.58310243060262,
28.9201898275409));
#17175=CARTESIAN_POINT('Ctrl Pts',(-9.65136659729197,-0.293655596345962,
28.9081866407515));
#17176=CARTESIAN_POINT('Ctrl Pts',(-9.67581103310558,-0.197813707971806,
28.9042121350661));
#17177=CARTESIAN_POINT('Ctrl Pts',(-9.68822500000014,-0.098910050091216,
28.9002376293806));
#17178=CARTESIAN_POINT('Ctrl Pts',(-9.688225,1.63313806922361E-12,28.8962631236951));
#17179=CARTESIAN_POINT('Ctrl Pts',(-9.688225,-8.42104164178181E-14,28.8537368763048));
#17180=CARTESIAN_POINT('Ctrl Pts',(-9.68822499999998,-0.298712821306166,
28.8657400630942));
#17181=CARTESIAN_POINT('Ctrl Pts',(-9.57054245632583,-0.595858078271582,
28.8777432498835));
#17182=CARTESIAN_POINT('Ctrl Pts',(-9.36601586214931,-0.813569405232756,
28.8897464366728));
#17183=CARTESIAN_POINT('Ctrl Pts',(-9.1614892679728,-1.03128073219393,28.9017496234621));
#17184=CARTESIAN_POINT('Ctrl Pts',(-8.87226522412844,-1.16727314847136,
28.9137528102514));
#17185=CARTESIAN_POINT('Ctrl Pts',(-8.57413435701449,-1.1859100926019,28.9257559970407));
#17186=CARTESIAN_POINT('Ctrl Pts',(-8.27600348990054,-1.20454703673244,
28.9377591838301));
#17187=CARTESIAN_POINT('Ctrl Pts',(-7.97209482032096,-1.1056329054011,28.9497623706194));
#17188=CARTESIAN_POINT('Ctrl Pts',(-7.74204705372064,-0.915087963996601,
28.9617655574087));
#17189=CARTESIAN_POINT('Ctrl Pts',(-7.51199928712033,-0.724543022592099,
28.973768744198));
#17190=CARTESIAN_POINT('Ctrl Pts',(-7.35822688079637,-0.444367128061534,
28.9857719309873));
#17191=CARTESIAN_POINT('Ctrl Pts',(-7.32102560975818,-0.147979855990377,
28.9977751177767));
#17192=CARTESIAN_POINT('Ctrl Pts',(-7.28382433871999,0.148407416080781,
29.009778304566));
#17193=CARTESIAN_POINT('Ctrl Pts',(-7.36358464744632,0.457895344721854,
29.0217814913553));
#17194=CARTESIAN_POINT('Ctrl Pts',(-7.53940549437875,0.6993831899576,29.0337846781446));
#17195=CARTESIAN_POINT('Ctrl Pts',(-7.71522634131118,0.940871035193346,
29.0457878649339));
#17196=CARTESIAN_POINT('Ctrl Pts',(-7.9852624056577,1.11182427083076,29.0577910517232));
#17197=CARTESIAN_POINT('Ctrl Pts',(-8.27875123560101,1.16744491727744,29.0697942385126));
#17198=CARTESIAN_POINT('Ctrl Pts',(-8.57224006554432,1.22306556372412,29.0817974253019));
#17199=CARTESIAN_POINT('Ctrl Pts',(-8.88610136059923,1.1627698566703,29.0938006120912));
#17200=CARTESIAN_POINT('Ctrl Pts',(-9.13808834820077,1.0023581747636,29.1058037988805));
#17201=CARTESIAN_POINT('Ctrl Pts',(-9.39007533580232,0.841946492856894,
29.1178069856698));
#17202=CARTESIAN_POINT('Ctrl Pts',(-9.57754329642125,0.583102430603112,
29.1298101724591));
#17203=CARTESIAN_POINT('Ctrl Pts',(-9.65136659729185,0.293655596346441,
29.1418133592485));
#17204=CARTESIAN_POINT('Ctrl Pts',(-9.67581103310541,0.197813707972643,
29.1457878649339));
#17205=CARTESIAN_POINT('Ctrl Pts',(-9.688225,0.0989100500924303,29.1497623706194));
#17206=CARTESIAN_POINT('Ctrl Pts',(-9.688225,-5.8564264548977E-14,29.1537368763048));
#17207=CARTESIAN_POINT('Origin',(-8.5,0.,1.8));
#17208=CARTESIAN_POINT('',(-9.688225,1.68431935065882E-12,29.4962631236951));
#17209=CARTESIAN_POINT('',(-9.68727888030919,8.85048131729375E-5,29.4537368763048));
#17210=CARTESIAN_POINT('',(-9.688225,-1.45515594291686E-16,1.8));
#17211=CARTESIAN_POINT('Ctrl Pts',(-9.688225,1.68431935065882E-12,29.4962631236951));
#17212=CARTESIAN_POINT('Ctrl Pts',(-9.68822499999958,0.298712821307722,
29.4842599369058));
#17213=CARTESIAN_POINT('Ctrl Pts',(-9.57054245632506,0.595858078272935,
29.4722567501165));
#17214=CARTESIAN_POINT('Ctrl Pts',(-9.36601586214831,0.813569405233824,
29.4602535633272));
#17215=CARTESIAN_POINT('Ctrl Pts',(-9.16148926797156,1.03128073219471,29.4482503765379));
#17216=CARTESIAN_POINT('Ctrl Pts',(-8.87226522412708,1.16727314847178,29.4362471897485));
#17217=CARTESIAN_POINT('Ctrl Pts',(-8.57413435701316,1.18591009260198,29.4242440029592));
#17218=CARTESIAN_POINT('Ctrl Pts',(-8.27600348989924,1.20454703673219,29.4122408161699));
#17219=CARTESIAN_POINT('Ctrl Pts',(-7.97209482031981,1.10563290540054,29.4002376293806));
#17220=CARTESIAN_POINT('Ctrl Pts',(-7.74204705371972,0.915087963995839,
29.3882344425913));
#17221=CARTESIAN_POINT('Ctrl Pts',(-7.51199928711963,0.724543022591135,
29.376231255802));
#17222=CARTESIAN_POINT('Ctrl Pts',(-7.35822688079597,0.444367128060472,
29.3642280690126));
#17223=CARTESIAN_POINT('Ctrl Pts',(-7.32102560975805,0.147979855989325,
29.3522248822233));
#17224=CARTESIAN_POINT('Ctrl Pts',(-7.28382433872013,-0.148407416081821,
29.340221695434));
#17225=CARTESIAN_POINT('Ctrl Pts',(-7.36358464744671,-0.457895344722775,
29.3282185086447));
#17226=CARTESIAN_POINT('Ctrl Pts',(-7.5394054943793,-0.699383189958348,
29.3162153218554));
#17227=CARTESIAN_POINT('Ctrl Pts',(-7.71522634131188,-0.940871035193921,
29.3042121350661));
#17228=CARTESIAN_POINT('Ctrl Pts',(-7.98526240565849,-1.11182427083111,
29.2922089482767));
#17229=CARTESIAN_POINT('Ctrl Pts',(-8.27875123560179,-1.16744491727758,
29.2802057614874));
#17230=CARTESIAN_POINT('Ctrl Pts',(-8.57224006554509,-1.22306556372406,
29.2682025746981));
#17231=CARTESIAN_POINT('Ctrl Pts',(-8.88610136059991,-1.16276985667006,
29.2561993879088));
#17232=CARTESIAN_POINT('Ctrl Pts',(-9.13808834820133,-1.00235817476324,
29.2441962011195));
#17233=CARTESIAN_POINT('Ctrl Pts',(-9.39007533580275,-0.841946492856428,
29.2321930143302));
#17234=CARTESIAN_POINT('Ctrl Pts',(-9.57754329642152,-0.583102430602597,
29.2201898275409));
#17235=CARTESIAN_POINT('Ctrl Pts',(-9.65136659729198,-0.293655596345938,
29.2081866407515));
#17236=CARTESIAN_POINT('Ctrl Pts',(-9.67581103310559,-0.19781370797178,
29.2042121350661));
#17237=CARTESIAN_POINT('Ctrl Pts',(-9.68822500000014,-0.0989100500911904,
29.2002376293806));
#17238=CARTESIAN_POINT('Ctrl Pts',(-9.688225,1.65867319878998E-12,29.1962631236951));
#17239=CARTESIAN_POINT('Ctrl Pts',(-9.688225,-5.8564264548977E-14,29.1537368763048));
#17240=CARTESIAN_POINT('Ctrl Pts',(-9.68822499999998,-0.298712821306141,
29.1657400630942));
#17241=CARTESIAN_POINT('Ctrl Pts',(-9.57054245632584,-0.595858078271559,
29.1777432498835));
#17242=CARTESIAN_POINT('Ctrl Pts',(-9.36601586214933,-0.813569405232737,
29.1897464366728));
#17243=CARTESIAN_POINT('Ctrl Pts',(-9.16148926797282,-1.03128073219392,
29.2017496234621));
#17244=CARTESIAN_POINT('Ctrl Pts',(-8.87226522412846,-1.16727314847135,
29.2137528102514));
#17245=CARTESIAN_POINT('Ctrl Pts',(-8.57413435701451,-1.1859100926019,29.2257559970407));
#17246=CARTESIAN_POINT('Ctrl Pts',(-8.27600348990057,-1.20454703673244,
29.2377591838301));
#17247=CARTESIAN_POINT('Ctrl Pts',(-7.97209482032099,-1.10563290540111,
29.2497623706194));
#17248=CARTESIAN_POINT('Ctrl Pts',(-7.74204705372066,-0.915087963996617,
29.2617655574087));
#17249=CARTESIAN_POINT('Ctrl Pts',(-7.51199928712034,-0.724543022592121,
29.273768744198));
#17250=CARTESIAN_POINT('Ctrl Pts',(-7.35822688079638,-0.444367128061559,
29.2857719309873));
#17251=CARTESIAN_POINT('Ctrl Pts',(-7.32102560975818,-0.147979855990402,
29.2977751177767));
#17252=CARTESIAN_POINT('Ctrl Pts',(-7.28382433871999,0.148407416080755,
29.309778304566));
#17253=CARTESIAN_POINT('Ctrl Pts',(-7.36358464744631,0.457895344721829,
29.3217814913553));
#17254=CARTESIAN_POINT('Ctrl Pts',(-7.53940549437874,0.699383189957579,
29.3337846781446));
#17255=CARTESIAN_POINT('Ctrl Pts',(-7.71522634131116,0.940871035193329,
29.3457878649339));
#17256=CARTESIAN_POINT('Ctrl Pts',(-7.98526240565768,1.11182427083075,29.3577910517232));
#17257=CARTESIAN_POINT('Ctrl Pts',(-8.27875123560099,1.16744491727743,29.3697942385126));
#17258=CARTESIAN_POINT('Ctrl Pts',(-8.5722400655443,1.22306556372412,29.3817974253019));
#17259=CARTESIAN_POINT('Ctrl Pts',(-8.8861013605992,1.16276985667031,29.3938006120912));
#17260=CARTESIAN_POINT('Ctrl Pts',(-9.13808834820075,1.00235817476361,29.4058037988805));
#17261=CARTESIAN_POINT('Ctrl Pts',(-9.3900753358023,0.841946492856913,29.4178069856698));
#17262=CARTESIAN_POINT('Ctrl Pts',(-9.57754329642124,0.583102430603135,
29.4298101724591));
#17263=CARTESIAN_POINT('Ctrl Pts',(-9.65136659729185,0.293655596346466,
29.4418133592485));
#17264=CARTESIAN_POINT('Ctrl Pts',(-9.67581103310541,0.197813707972669,
29.4457878649339));
#17265=CARTESIAN_POINT('Ctrl Pts',(-9.688225,0.0989100500924559,29.4497623706194));
#17266=CARTESIAN_POINT('Ctrl Pts',(-9.688225,-3.29736238313671E-14,29.4537368763048));
#17267=CARTESIAN_POINT('Origin',(-8.5,0.,1.8));
#17268=CARTESIAN_POINT('',(-9.688225,1.70996550252767E-12,29.7962631236951));
#17269=CARTESIAN_POINT('',(-9.68829027239597,-0.000978575593966811,29.7537368763048));
#17270=CARTESIAN_POINT('',(-9.688225,-1.45515594291686E-16,1.8));
#17271=CARTESIAN_POINT('Ctrl Pts',(-9.688225,1.70996550252767E-12,29.7962631236951));
#17272=CARTESIAN_POINT('Ctrl Pts',(-9.68822499999957,0.298712821307747,
29.7842599369058));
#17273=CARTESIAN_POINT('Ctrl Pts',(-9.57054245632505,0.595858078272958,
29.7722567501165));
#17274=CARTESIAN_POINT('Ctrl Pts',(-9.36601586214829,0.813569405233843,
29.7602535633272));
#17275=CARTESIAN_POINT('Ctrl Pts',(-9.16148926797154,1.03128073219473,29.7482503765379));
#17276=CARTESIAN_POINT('Ctrl Pts',(-8.87226522412706,1.16727314847179,29.7362471897485));
#17277=CARTESIAN_POINT('Ctrl Pts',(-8.57413435701313,1.18591009260199,29.7242440029592));
#17278=CARTESIAN_POINT('Ctrl Pts',(-8.27600348989921,1.20454703673218,29.7122408161699));
#17279=CARTESIAN_POINT('Ctrl Pts',(-7.97209482031979,1.10563290540053,29.7002376293806));
#17280=CARTESIAN_POINT('Ctrl Pts',(-7.7420470537197,0.915087963995822,29.6882344425913));
#17281=CARTESIAN_POINT('Ctrl Pts',(-7.51199928711962,0.724543022591113,
29.676231255802));
#17282=CARTESIAN_POINT('Ctrl Pts',(-7.35822688079596,0.444367128060447,
29.6642280690126));
#17283=CARTESIAN_POINT('Ctrl Pts',(-7.32102560975805,0.1479798559893,29.6522248822233));
#17284=CARTESIAN_POINT('Ctrl Pts',(-7.28382433872013,-0.148407416081847,
29.640221695434));
#17285=CARTESIAN_POINT('Ctrl Pts',(-7.36358464744672,-0.457895344722799,
29.6282185086447));
#17286=CARTESIAN_POINT('Ctrl Pts',(-7.53940549437931,-0.699383189958368,
29.6162153218554));
#17287=CARTESIAN_POINT('Ctrl Pts',(-7.7152263413119,-0.940871035193937,
29.6042121350661));
#17288=CARTESIAN_POINT('Ctrl Pts',(-7.98526240565851,-1.11182427083112,
29.5922089482767));
#17289=CARTESIAN_POINT('Ctrl Pts',(-8.27875123560181,-1.16744491727759,
29.5802057614874));
#17290=CARTESIAN_POINT('Ctrl Pts',(-8.57224006554512,-1.22306556372406,
29.5682025746981));
#17291=CARTESIAN_POINT('Ctrl Pts',(-8.88610136059993,-1.16276985667005,
29.5561993879088));
#17292=CARTESIAN_POINT('Ctrl Pts',(-9.13808834820135,-1.00235817476323,
29.5441962011195));
#17293=CARTESIAN_POINT('Ctrl Pts',(-9.39007533580277,-0.841946492856409,
29.5321930143302));
#17294=CARTESIAN_POINT('Ctrl Pts',(-9.57754329642153,-0.583102430602574,
29.5201898275409));
#17295=CARTESIAN_POINT('Ctrl Pts',(-9.65136659729199,-0.293655596345913,
29.5081866407515));
#17296=CARTESIAN_POINT('Ctrl Pts',(-9.67581103310559,-0.197813707971755,
29.5042121350661));
#17297=CARTESIAN_POINT('Ctrl Pts',(-9.68822500000014,-0.0989100500911648,
29.5002376293806));
#17298=CARTESIAN_POINT('Ctrl Pts',(-9.688225,1.68431935065882E-12,29.4962631236951));
#17299=CARTESIAN_POINT('Ctrl Pts',(-9.68630702871204,0.000179416718910312,
29.4537368763049));
#17300=CARTESIAN_POINT('Ctrl Pts',(-9.68614803161525,-0.208258635069709,
29.4620824521433));
#17301=CARTESIAN_POINT('Ctrl Pts',(-9.63399075937292,-0.416818054777034,
29.4704280279817));
#17302=CARTESIAN_POINT('Ctrl Pts',(-9.53044187393016,-0.595799011918308,
29.4787736038201));
#17303=CARTESIAN_POINT('Ctrl Pts',(-9.33306934044666,-0.936951162472383,
29.4946809449717));
#17304=CARTESIAN_POINT('Ctrl Pts',(-8.94898369186194,-1.17064050846203,
29.5105882861234));
#17305=CARTESIAN_POINT('Ctrl Pts',(-8.55559785580855,-1.18900976154421,
29.526495627275));
#17306=CARTESIAN_POINT('Ctrl Pts',(-8.16221201975512,-1.2073790146264,29.5424029684266));
#17307=CARTESIAN_POINT('Ctrl Pts',(-7.75952599623297,-1.01042817480108,
29.5583103095782));
#17308=CARTESIAN_POINT('Ctrl Pts',(-7.53039248685666,-0.689467174220619,
29.5742176507298));
#17309=CARTESIAN_POINT('Ctrl Pts',(-7.41582573216856,-0.528986673930462,
29.5821713213056));
#17310=CARTESIAN_POINT('Ctrl Pts',(-7.34464710601685,-0.33750363345153,
29.5901249918815));
#17311=CARTESIAN_POINT('Ctrl Pts',(-7.32116324979802,-0.140351109640275,
29.5980786624573));
#17312=CARTESIAN_POINT('Ctrl Pts',(-7.29767939357918,0.0568014141710692,
29.6060323330331));
#17313=CARTESIAN_POINT('Ctrl Pts',(-7.32189030729322,0.259623421314646,
29.6139860036089));
#17314=CARTESIAN_POINT('Ctrl Pts',(-7.39558129849426,0.442514540719367,
29.6219396741847));
#17315=CARTESIAN_POINT('Ctrl Pts',(-7.54296328089633,0.808296779528768,
29.6378470153363));
#17316=CARTESIAN_POINT('Ctrl Pts',(-7.88826557324638,1.09435546738231,29.6537543564879));
#17317=CARTESIAN_POINT('Ctrl Pts',(-8.27492430307999,1.16885146040352,29.6696616976396));
#17318=CARTESIAN_POINT('Ctrl Pts',(-8.66158303291351,1.2433474534247,29.6855690387912));
#17319=CARTESIAN_POINT('Ctrl Pts',(-9.08959820023061,1.10628075161366,29.7014763799428));
#17320=CARTESIAN_POINT('Ctrl Pts',(-9.36164000612452,0.821043330033523,
29.7173837210944));
#17321=CARTESIAN_POINT('Ctrl Pts',(-9.56887300417075,0.603758321816504,
29.7295014394979));
#17322=CARTESIAN_POINT('Ctrl Pts',(-9.68559592122482,0.300491042494952,
29.7416191579014));
#17323=CARTESIAN_POINT('Ctrl Pts',(-9.68829027239597,-0.000978575593966811,
29.7537368763048));
#17324=CARTESIAN_POINT('Origin',(-8.5,0.,1.24542303242842));
#17325=CARTESIAN_POINT('',(-9.516475,1.77136955610542E-12,29.8954230324284));
#17326=CARTESIAN_POINT('',(-9.516475,1.79831334285591E-12,29.9545769675714));
#17327=CARTESIAN_POINT('',(-9.516475,1.78524650477582E-12,1.24542303242842));
#17328=CARTESIAN_POINT('',(-7.90984029786094,-0.827606761449023,30.));
#17329=CARTESIAN_POINT('Ctrl Pts',(-9.516475,1.8869293844785E-12,29.8954230324284));
#17330=CARTESIAN_POINT('Ctrl Pts',(-9.51647500000049,-0.265706620582062,
29.9079039656766));
#17331=CARTESIAN_POINT('Ctrl Pts',(-9.40727465387295,-0.529786878175418,
29.9203848989248));
#17332=CARTESIAN_POINT('Ctrl Pts',(-9.21961691907893,-0.717894780173495,
29.932865832173));
#17333=CARTESIAN_POINT('Ctrl Pts',(-9.0319591842849,-0.906002682171572,
29.9453467654212));
#17334=CARTESIAN_POINT('Ctrl Pts',(-8.7681413283455,-1.01583545019863,29.9578276986694));
#17335=CARTESIAN_POINT('Ctrl Pts',(-8.50243547044677,-1.01647208230659,
29.9703086319176));
#17336=CARTESIAN_POINT('Ctrl Pts',(-8.29173620430335,-1.0169769184401,29.9802057546117));
#17337=CARTESIAN_POINT('Ctrl Pts',(-8.0813906437366,-0.94993792854409,29.9901028773059));
#17338=CARTESIAN_POINT('Ctrl Pts',(-7.90984029786094,-0.827606761449023,
30.));
#17339=CARTESIAN_POINT('',(-9.09015970213943,-0.827606761448756,30.));
#17340=CARTESIAN_POINT('Origin',(-8.5,0.,30.));
#17341=CARTESIAN_POINT('Ctrl Pts',(-9.51769523843386,0.000138611918728023,
29.9545769675714));
#17342=CARTESIAN_POINT('Ctrl Pts',(-9.51757347611664,-0.152713583871541,
29.9617643078051));
#17343=CARTESIAN_POINT('Ctrl Pts',(-9.44060368458966,-0.475706479329954,
29.9769053186147));
#17344=CARTESIAN_POINT('Ctrl Pts',(-9.22802350159151,-0.72929719873085,
29.9920463294242));
#17345=CARTESIAN_POINT('Ctrl Pts',(-9.09015970213924,-0.82760676144889,
30.));
#17346=CARTESIAN_POINT('Origin',(-8.5,0.,1.24542303242842));
#17347=CARTESIAN_POINT('',(-9.516475,1.74945312371443E-12,29.5954230324284));
#17348=CARTESIAN_POINT('',(-9.516475,1.776396937294E-12,29.6545769675714));
#17349=CARTESIAN_POINT('',(-9.516475,1.78524650477582E-12,1.24542303242842));
#17350=CARTESIAN_POINT('Ctrl Pts',(-9.516475,1.74945312371443E-12,29.5954230324284));
#17351=CARTESIAN_POINT('Ctrl Pts',(-9.51647500000046,-0.2657066205822,29.6079039656766));
#17352=CARTESIAN_POINT('Ctrl Pts',(-9.40727465387288,-0.529786878175541,
29.6203848989248));
#17353=CARTESIAN_POINT('Ctrl Pts',(-9.21961691907883,-0.717894780173593,
29.632865832173));
#17354=CARTESIAN_POINT('Ctrl Pts',(-9.03195918428478,-0.906002682171644,
29.6453467654212));
#17355=CARTESIAN_POINT('Ctrl Pts',(-8.76814132834537,-1.01583545019867,
29.6578276986694));
#17356=CARTESIAN_POINT('Ctrl Pts',(-8.50243547044663,-1.01647208230659,
29.6703086319176));
#17357=CARTESIAN_POINT('Ctrl Pts',(-8.2367296125479,-1.01710871441452,29.6827895651657));
#17358=CARTESIAN_POINT('Ctrl Pts',(-7.9723884693348,-0.908541417083597,
29.6952704984139));
#17359=CARTESIAN_POINT('Ctrl Pts',(-7.78383148002456,-0.72133492679974,
29.7077514316621));
#17360=CARTESIAN_POINT('Ctrl Pts',(-7.59527449071432,-0.534128436515884,
29.7202323649103));
#17361=CARTESIAN_POINT('Ctrl Pts',(-7.48480993131748,-0.270574496757414,
29.7327132981585));
#17362=CARTESIAN_POINT('Ctrl Pts',(-7.48353667075687,-0.00487092690994738,
29.7451942314067));
#17363=CARTESIAN_POINT('Ctrl Pts',(-7.48226341019625,0.260832642937519,
29.7576751646549));
#17364=CARTESIAN_POINT('Ctrl Pts',(-7.59019703546662,0.525433154238881,
29.7701560979031));
#17365=CARTESIAN_POINT('Ctrl Pts',(-7.77695120652395,0.71443814839203,29.7826370311513));
#17366=CARTESIAN_POINT('Ctrl Pts',(-7.96370537758128,0.903443142545179,
29.7951179643995));
#17367=CARTESIAN_POINT('Ctrl Pts',(-8.2269938881465,1.01453885915611,29.8075988976476));
#17368=CARTESIAN_POINT('Ctrl Pts',(-8.49269364458979,1.01644874085987,29.8200798308958));
#17369=CARTESIAN_POINT('Ctrl Pts',(-8.75839340103307,1.01835862256364,29.832560764144));
#17370=CARTESIAN_POINT('Ctrl Pts',(-9.02325176140223,0.911059288979924,
29.8450416973922));
#17371=CARTESIAN_POINT('Ctrl Pts',(-9.21270367535709,0.724758509268773,
29.8575226306404));
#17372=CARTESIAN_POINT('Ctrl Pts',(-9.40215558931195,0.538457729557621,
29.8700035638886));
#17373=CARTESIAN_POINT('Ctrl Pts',(-9.51388182535791,0.275436159674178,
29.8824844971368));
#17374=CARTESIAN_POINT('Ctrl Pts',(-9.51642831724056,0.00974174196610049,
29.894965430385));
#17375=CARTESIAN_POINT('Ctrl Pts',(-9.51645943884196,0.00649459406839334,
29.8951179643995));
#17376=CARTESIAN_POINT('Ctrl Pts',(-9.51647499999999,0.00324729703536851,
29.8952704984139));
#17377=CARTESIAN_POINT('Ctrl Pts',(-9.516475,1.8869293844785E-12,29.8954230324284));
#17378=CARTESIAN_POINT('Ctrl Pts',(-9.516475,1.776396937294E-12,29.6545769675714));
#17379=CARTESIAN_POINT('Ctrl Pts',(-9.51647500000046,-0.265706620582173,
29.6670579008196));
#17380=CARTESIAN_POINT('Ctrl Pts',(-9.4072746538729,-0.529786878175517,
29.6795388340678));
#17381=CARTESIAN_POINT('Ctrl Pts',(-9.21961691907885,-0.717894780173574,
29.692019767316));
#17382=CARTESIAN_POINT('Ctrl Pts',(-9.0319591842848,-0.90600268217163,29.7045007005642));
#17383=CARTESIAN_POINT('Ctrl Pts',(-8.76814132834539,-1.01583545019866,
29.7169816338124));
#17384=CARTESIAN_POINT('Ctrl Pts',(-8.50243547044666,-1.01647208230659,
29.7294625670606));
#17385=CARTESIAN_POINT('Ctrl Pts',(-8.23672961254792,-1.01710871441453,
29.7419435003088));
#17386=CARTESIAN_POINT('Ctrl Pts',(-7.97238846933483,-0.908541417083611,
29.754424433557));
#17387=CARTESIAN_POINT('Ctrl Pts',(-7.78383148002458,-0.721334926799759,
29.7669053668051));
#17388=CARTESIAN_POINT('Ctrl Pts',(-7.59527449071433,-0.534128436515908,
29.7793863000533));
#17389=CARTESIAN_POINT('Ctrl Pts',(-7.48480993131749,-0.270574496757441,
29.7918672333015));
#17390=CARTESIAN_POINT('Ctrl Pts',(-7.48353667075687,-0.00487092690997433,
29.8043481665497));
#17391=CARTESIAN_POINT('Ctrl Pts',(-7.48226341019624,0.260832642937492,
29.8168290997979));
#17392=CARTESIAN_POINT('Ctrl Pts',(-7.59019703546661,0.525433154238857,
29.8293100330461));
#17393=CARTESIAN_POINT('Ctrl Pts',(-7.77695120652393,0.714438148392011,
29.8417909662943));
#17394=CARTESIAN_POINT('Ctrl Pts',(-7.96370537758126,0.903443142545165,
29.8542718995425));
#17395=CARTESIAN_POINT('Ctrl Pts',(-8.22699388814648,1.0145388591561,29.8667528327907));
#17396=CARTESIAN_POINT('Ctrl Pts',(-8.49269364458976,1.01644874085987,29.8792337660389));
#17397=CARTESIAN_POINT('Ctrl Pts',(-8.75839340103304,1.01835862256364,29.891714699287));
#17398=CARTESIAN_POINT('Ctrl Pts',(-9.02325176140221,0.911059288979938,
29.9041956325352));
#17399=CARTESIAN_POINT('Ctrl Pts',(-9.21270367535707,0.724758509268792,
29.9166765657834));
#17400=CARTESIAN_POINT('Ctrl Pts',(-9.40215558931194,0.538457729557645,
29.9291574990316));
#17401=CARTESIAN_POINT('Ctrl Pts',(-9.5138818253579,0.275436159674205,29.9416384322798));
#17402=CARTESIAN_POINT('Ctrl Pts',(-9.51642831724056,0.00974174196612743,
29.954119365528));
#17403=CARTESIAN_POINT('Ctrl Pts',(-9.51645943884196,0.00649459406838176,
29.9542718995425));
#17404=CARTESIAN_POINT('Ctrl Pts',(-9.51647499999999,0.00324729703531833,
29.954424433557));
#17405=CARTESIAN_POINT('Ctrl Pts',(-9.516475,1.79831336968498E-12,29.9545769675714));
#17406=CARTESIAN_POINT('Origin',(-8.5,0.,1.24542303242842));
#17407=CARTESIAN_POINT('',(-9.516475,1.72753669132345E-12,29.2954230324284));
#17408=CARTESIAN_POINT('',(-9.51618362200288,2.72569712245247E-5,29.3545769675714));
#17409=CARTESIAN_POINT('',(-9.516475,1.78524650477582E-12,1.24542303242842));
#17410=CARTESIAN_POINT('Ctrl Pts',(-9.516475,1.72753669132345E-12,29.2954230324284));
#17411=CARTESIAN_POINT('Ctrl Pts',(-9.51647500000045,-0.265706620582183,
29.3079039656766));
#17412=CARTESIAN_POINT('Ctrl Pts',(-9.4072746538729,-0.529786878175485,
29.3203848989248));
#17413=CARTESIAN_POINT('Ctrl Pts',(-9.2196169190789,-0.717894780173526,
29.332865832173));
#17414=CARTESIAN_POINT('Ctrl Pts',(-9.03195918428489,-0.906002682171568,
29.3453467654212));
#17415=CARTESIAN_POINT('Ctrl Pts',(-8.76814132834554,-1.01583545019861,
29.3578276986694));
#17416=CARTESIAN_POINT('Ctrl Pts',(-8.50243547044684,-1.01647208230659,
29.3703086319175));
#17417=CARTESIAN_POINT('Ctrl Pts',(-8.23672961254815,-1.01710871441458,
29.3827895651657));
#17418=CARTESIAN_POINT('Ctrl Pts',(-7.97238846933507,-0.908541417083738,
29.3952704984139));
#17419=CARTESIAN_POINT('Ctrl Pts',(-7.78383148002479,-0.721334926799969,
29.4077514316621));
#17420=CARTESIAN_POINT('Ctrl Pts',(-7.59527449071451,-0.5341284365162,29.4202323649103));
#17421=CARTESIAN_POINT('Ctrl Pts',(-7.4848099313176,-0.270574496757815,
29.4327132981585));
#17422=CARTESIAN_POINT('Ctrl Pts',(-7.48353667075687,-0.0048709269103877,
29.4451942314067));
#17423=CARTESIAN_POINT('Ctrl Pts',(-7.48226341019614,0.26083264293704,29.4576751646549));
#17424=CARTESIAN_POINT('Ctrl Pts',(-7.59019703546636,0.525433154238411,
29.4701560979031));
#17425=CARTESIAN_POINT('Ctrl Pts',(-7.77695120652356,0.714438148391635,
29.4826370311512));
#17426=CARTESIAN_POINT('Ctrl Pts',(-7.96370537758076,0.903443142544859,
29.4951179643994));
#17427=CARTESIAN_POINT('Ctrl Pts',(-8.22699388814587,1.01453885915593,29.5075988976476));
#17428=CARTESIAN_POINT('Ctrl Pts',(-8.49269364458912,1.01644874085987,29.5200798308958));
#17429=CARTESIAN_POINT('Ctrl Pts',(-8.75839340103236,1.01835862256381,29.532560764144));
#17430=CARTESIAN_POINT('Ctrl Pts',(-9.02325176140155,0.911059288980303,
29.5450416973922));
#17431=CARTESIAN_POINT('Ctrl Pts',(-9.21270367535653,0.724758509269325,
29.5575226306404));
#17432=CARTESIAN_POINT('Ctrl Pts',(-9.40215558931151,0.538457729558346,
29.5700035638886));
#17433=CARTESIAN_POINT('Ctrl Pts',(-9.51388182535766,0.27543615967504,29.5824844971367));
#17434=CARTESIAN_POINT('Ctrl Pts',(-9.51642831724055,0.00974174196700301,
29.5949654303849));
#17435=CARTESIAN_POINT('Ctrl Pts',(-9.51645943884196,0.00649459406894922,
29.5951179643994));
#17436=CARTESIAN_POINT('Ctrl Pts',(-9.51647499999999,0.00324729703557761,
29.5952704984139));
#17437=CARTESIAN_POINT('Ctrl Pts',(-9.516475,1.74945312371443E-12,29.5954230324284));
#17438=CARTESIAN_POINT('Ctrl Pts',(-9.51483425867161,0.000153483230988238,
29.3545769675714));
#17439=CARTESIAN_POINT('Ctrl Pts',(-9.51469824354527,-0.178156238154032,
29.3629225434099));
#17440=CARTESIAN_POINT('Ctrl Pts',(-9.47007995719168,-0.356569784534552,
29.3712681192483));
#17441=CARTESIAN_POINT('Ctrl Pts',(-9.38149837261734,-0.509680237866999,
29.3796136950868));
#17442=CARTESIAN_POINT('Ctrl Pts',(-9.21265472265832,-0.801521120052119,
29.3955210362384));
#17443=CARTESIAN_POINT('Ctrl Pts',(-8.8840860932784,-1.00143222945046,29.41142837739));
#17444=CARTESIAN_POINT('Ctrl Pts',(-8.54756155650945,-1.01714632949621,
29.4273357185417));
#17445=CARTESIAN_POINT('Ctrl Pts',(-8.21103701974038,-1.03286042954196,
29.4432430596933));
#17446=CARTESIAN_POINT('Ctrl Pts',(-7.86655657558232,-0.864377520234989,
29.4591504008449));
#17447=CARTESIAN_POINT('Ctrl Pts',(-7.67054278699563,-0.589809291940723,
29.4750577419965));
#17448=CARTESIAN_POINT('Ctrl Pts',(-7.57253589270232,-0.452525177793652,
29.4830114125723));
#17449=CARTESIAN_POINT('Ctrl Pts',(-7.51164566230181,-0.288719733899682,
29.4909650831482));
#17450=CARTESIAN_POINT('Ctrl Pts',(-7.49155624089586,-0.12006429268186,
29.498918753724));
#17451=CARTESIAN_POINT('Ctrl Pts',(-7.4714668194899,0.0485911485360002,
29.5068724242998));
#17452=CARTESIAN_POINT('Ctrl Pts',(-7.49217820707847,0.222096587077811,
29.5148260948756));
#17453=CARTESIAN_POINT('Ctrl Pts',(-7.55521765691417,0.378552014793018,
29.5227797654514));
#17454=CARTESIAN_POINT('Ctrl Pts',(-7.68129655658559,0.691462870223505,
29.538687106603));
#17455=CARTESIAN_POINT('Ctrl Pts',(-7.97668770524555,0.936173682347486,
29.5545944477546));
#17456=CARTESIAN_POINT('Ctrl Pts',(-8.30745749413879,0.999901776358546,
29.5705017889063));
#17457=CARTESIAN_POINT('Ctrl Pts',(-8.63822728303192,1.06362987036958,29.5864091300579));
#17458=CARTESIAN_POINT('Ctrl Pts',(-9.00437571215826,0.94637524626783,29.6023164712095));
#17459=CARTESIAN_POINT('Ctrl Pts',(-9.23709568913741,0.702366991854193,
29.6182238123611));
#17460=CARTESIAN_POINT('Ctrl Pts',(-9.41437453926143,0.516489082597208,
29.6303415307646));
#17461=CARTESIAN_POINT('Ctrl Pts',(-9.51422593702913,0.25705706614624,29.642459249168));
#17462=CARTESIAN_POINT('Ctrl Pts',(-9.51653083770639,-0.000837129015673788,
29.6545769675714));
#17463=CARTESIAN_POINT('Origin',(-8.5,0.,1.24542303242842));
#17464=CARTESIAN_POINT('',(-9.516475,1.70562025893246E-12,28.9954230324284));
#17465=CARTESIAN_POINT('',(-9.516475,1.73256407251203E-12,29.0545769675714));
#17466=CARTESIAN_POINT('',(-9.516475,1.78524650477582E-12,1.24542303242842));
#17467=CARTESIAN_POINT('Ctrl Pts',(-9.516475,1.70562025893246E-12,28.9954230324284));
#17468=CARTESIAN_POINT('Ctrl Pts',(-9.51647500000045,-0.265706620582321,
29.0079039656766));
#17469=CARTESIAN_POINT('Ctrl Pts',(-9.40727465387279,-0.529786878175732,
29.0203848989248));
#17470=CARTESIAN_POINT('Ctrl Pts',(-9.21961691907864,-0.717894780173787,
29.032865832173));
#17471=CARTESIAN_POINT('Ctrl Pts',(-9.03195918428448,-0.906002682171843,
29.0453467654212));
#17472=CARTESIAN_POINT('Ctrl Pts',(-8.76814132834494,-1.0158354501988,29.0578276986694));
#17473=CARTESIAN_POINT('Ctrl Pts',(-8.50243547044612,-1.0164720823066,29.0703086319176));
#17474=CARTESIAN_POINT('Ctrl Pts',(-8.23672961254731,-1.01710871441439,
29.0827895651658));
#17475=CARTESIAN_POINT('Ctrl Pts',(-7.9723884693342,-0.908541417083268,
29.095270498414));
#17476=CARTESIAN_POINT('Ctrl Pts',(-7.78383148002404,-0.721334926799221,
29.1077514316622));
#17477=CARTESIAN_POINT('Ctrl Pts',(-7.59527449071387,-0.534128436515173,
29.1202323649104));
#17478=CARTESIAN_POINT('Ctrl Pts',(-7.48480993131723,-0.270574496756524,
29.1327132981585));
#17479=CARTESIAN_POINT('Ctrl Pts',(-7.48353667075686,-0.00487092690897908,
29.1451942314067));
#17480=CARTESIAN_POINT('Ctrl Pts',(-7.4822634101965,0.260832642938566,29.1576751646549));
#17481=CARTESIAN_POINT('Ctrl Pts',(-7.59019703546719,0.5254331542399,29.1701560979031));
#17482=CARTESIAN_POINT('Ctrl Pts',(-7.7769512065248,0.714438148392883,29.1826370311513));
#17483=CARTESIAN_POINT('Ctrl Pts',(-7.9637053775824,0.903443142545867,29.1951179643995));
#17484=CARTESIAN_POINT('Ctrl Pts',(-8.22699388814785,1.01453885915649,29.2075988976477));
#17485=CARTESIAN_POINT('Ctrl Pts',(-8.49269364459122,1.01644874085988,29.2200798308959));
#17486=CARTESIAN_POINT('Ctrl Pts',(-8.75839340103458,1.01835862256327,29.2325607641441));
#17487=CARTESIAN_POINT('Ctrl Pts',(-9.02325176140366,0.911059288979123,
29.2450416973923));
#17488=CARTESIAN_POINT('Ctrl Pts',(-9.21270367535828,0.724758509267608,
29.2575226306405));
#17489=CARTESIAN_POINT('Ctrl Pts',(-9.40215558931289,0.538457729556092,
29.2700035638887));
#17490=CARTESIAN_POINT('Ctrl Pts',(-9.51388182535842,0.275436159672367,
29.2824844971369));
#17491=CARTESIAN_POINT('Ctrl Pts',(-9.51642831724057,0.00974174196420779,
29.2949654303851));
#17492=CARTESIAN_POINT('Ctrl Pts',(-9.51645943884196,0.00649459406707835,
29.2951179643995));
#17493=CARTESIAN_POINT('Ctrl Pts',(-9.51647499999999,0.00324729703463126,
29.295270498414));
#17494=CARTESIAN_POINT('Ctrl Pts',(-9.516475,1.72753669132345E-12,29.2954230324284));
#17495=CARTESIAN_POINT('Ctrl Pts',(-9.516475,1.73256407251203E-12,29.0545769675714));
#17496=CARTESIAN_POINT('Ctrl Pts',(-9.51647500000045,-0.265706620582294,
29.0670579008196));
#17497=CARTESIAN_POINT('Ctrl Pts',(-9.40727465387281,-0.529786878175708,
29.0795388340678));
#17498=CARTESIAN_POINT('Ctrl Pts',(-9.21961691907866,-0.717894780173768,
29.092019767316));
#17499=CARTESIAN_POINT('Ctrl Pts',(-9.0319591842845,-0.906002682171829,
29.1045007005642));
#17500=CARTESIAN_POINT('Ctrl Pts',(-8.76814132834496,-1.01583545019879,
29.1169816338124));
#17501=CARTESIAN_POINT('Ctrl Pts',(-8.50243547044615,-1.0164720823066,29.1294625670606));
#17502=CARTESIAN_POINT('Ctrl Pts',(-8.23672961254734,-1.0171087144144,29.1419435003088));
#17503=CARTESIAN_POINT('Ctrl Pts',(-7.97238846933422,-0.908541417083282,
29.154424433557));
#17504=CARTESIAN_POINT('Ctrl Pts',(-7.78383148002406,-0.72133492679924,
29.1669053668052));
#17505=CARTESIAN_POINT('Ctrl Pts',(-7.59527449071389,-0.534128436515197,
29.1793863000534));
#17506=CARTESIAN_POINT('Ctrl Pts',(-7.48480993131723,-0.270574496756551,
29.1918672333016));
#17507=CARTESIAN_POINT('Ctrl Pts',(-7.48353667075686,-0.00487092690900603,
29.2043481665498));
#17508=CARTESIAN_POINT('Ctrl Pts',(-7.48226341019649,0.260832642938539,
29.216829099798));
#17509=CARTESIAN_POINT('Ctrl Pts',(-7.59019703546717,0.525433154239876,
29.2293100330462));
#17510=CARTESIAN_POINT('Ctrl Pts',(-7.77695120652478,0.714438148392864,
29.2417909662943));
#17511=CARTESIAN_POINT('Ctrl Pts',(-7.96370537758238,0.903443142545853,
29.2542718995425));
#17512=CARTESIAN_POINT('Ctrl Pts',(-8.22699388814783,1.01453885915649,29.2667528327907));
#17513=CARTESIAN_POINT('Ctrl Pts',(-8.49269364459119,1.01644874085988,29.2792337660389));
#17514=CARTESIAN_POINT('Ctrl Pts',(-8.75839340103456,1.01835862256328,29.2917146992871));
#17515=CARTESIAN_POINT('Ctrl Pts',(-9.02325176140364,0.911059288979137,
29.3041956325353));
#17516=CARTESIAN_POINT('Ctrl Pts',(-9.21270367535826,0.724758509267627,
29.3166765657835));
#17517=CARTESIAN_POINT('Ctrl Pts',(-9.40215558931287,0.538457729556116,
29.3291574990317));
#17518=CARTESIAN_POINT('Ctrl Pts',(-9.51388182535841,0.275436159672394,
29.3416384322799));
#17519=CARTESIAN_POINT('Ctrl Pts',(-9.51642831724057,0.00974174196423473,
29.3541193655281));
#17520=CARTESIAN_POINT('Ctrl Pts',(-9.51645943884196,0.00649459406714381,
29.3542718995425));
#17521=CARTESIAN_POINT('Ctrl Pts',(-9.51647499999999,0.00324729703473532,
29.354424433557));
#17522=CARTESIAN_POINT('Ctrl Pts',(-9.516475,1.87004033327609E-12,29.3545769675714));
#17523=CARTESIAN_POINT('Origin',(-8.5,0.,1.24542303242842));
#17524=CARTESIAN_POINT('',(-9.516475,1.68370382654148E-12,28.6954230324284));
#17525=CARTESIAN_POINT('',(-9.51677113484703,-0.000181121393472947,28.7545769675714));
#17526=CARTESIAN_POINT('',(-9.516475,1.78524650477582E-12,1.24542303242842));
#17527=CARTESIAN_POINT('Ctrl Pts',(-9.516475,1.79926365491456E-12,28.6954230324284));
#17528=CARTESIAN_POINT('Ctrl Pts',(-9.51647500000047,-0.26570662058215,
28.7079039656766));
#17529=CARTESIAN_POINT('Ctrl Pts',(-9.40727465387291,-0.529786878175496,
28.7203848989248));
#17530=CARTESIAN_POINT('Ctrl Pts',(-9.21961691907887,-0.717894780173557,
28.732865832173));
#17531=CARTESIAN_POINT('Ctrl Pts',(-9.03195918428482,-0.906002682171618,
28.7453467654212));
#17532=CARTESIAN_POINT('Ctrl Pts',(-8.76814132834541,-1.01583545019865,
28.7578276986694));
#17533=CARTESIAN_POINT('Ctrl Pts',(-8.50243547044668,-1.01647208230659,
28.7703086319176));
#17534=CARTESIAN_POINT('Ctrl Pts',(-8.23672961254795,-1.01710871441454,
28.7827895651657));
#17535=CARTESIAN_POINT('Ctrl Pts',(-7.97238846933485,-0.908541417083623,
28.7952704984139));
#17536=CARTESIAN_POINT('Ctrl Pts',(-7.78383148002459,-0.721334926799775,
28.8077514316621));
#17537=CARTESIAN_POINT('Ctrl Pts',(-7.59527449071434,-0.534128436515928,
28.8202323649103));
#17538=CARTESIAN_POINT('Ctrl Pts',(-7.4848099313175,-0.270574496757464,
28.8327132981585));
#17539=CARTESIAN_POINT('Ctrl Pts',(-7.48353667075687,-0.00487092690999719,
28.8451942314067));
#17540=CARTESIAN_POINT('Ctrl Pts',(-7.48226341019623,0.260832642937469,
28.8576751646549));
#17541=CARTESIAN_POINT('Ctrl Pts',(-7.5901970354666,0.525433154238836,28.8701560979031));
#17542=CARTESIAN_POINT('Ctrl Pts',(-7.77695120652392,0.714438148391995,
28.8826370311513));
#17543=CARTESIAN_POINT('Ctrl Pts',(-7.96370537758124,0.903443142545153,
28.8951179643995));
#17544=CARTESIAN_POINT('Ctrl Pts',(-8.22699388814645,1.0145388591561,28.9075988976476));
#17545=CARTESIAN_POINT('Ctrl Pts',(-8.49269364458974,1.01644874085987,28.9200798308958));
#17546=CARTESIAN_POINT('Ctrl Pts',(-8.75839340103302,1.01835862256365,28.932560764144));
#17547=CARTESIAN_POINT('Ctrl Pts',(-9.02325176140219,0.91105928897995,28.9450416973922));
#17548=CARTESIAN_POINT('Ctrl Pts',(-9.21270367535706,0.724758509268808,
28.9575226306404));
#17549=CARTESIAN_POINT('Ctrl Pts',(-9.40215558931192,0.538457729557665,
28.9700035638886));
#17550=CARTESIAN_POINT('Ctrl Pts',(-9.51388182535789,0.275436159674228,
28.9824844971368));
#17551=CARTESIAN_POINT('Ctrl Pts',(-9.51642831724055,0.0097417419661503,
28.994965430385));
#17552=CARTESIAN_POINT('Ctrl Pts',(-9.51645943884196,0.00649459406836611,
28.9951179643995));
#17553=CARTESIAN_POINT('Ctrl Pts',(-9.51647499999999,0.00324729703526424,
28.9952704984139));
#17554=CARTESIAN_POINT('Ctrl Pts',(-9.516475,1.70562025893246E-12,28.9954230324284));
#17555=CARTESIAN_POINT('Ctrl Pts',(-9.516475,1.71064764012104E-12,28.7545769675714));
#17556=CARTESIAN_POINT('Ctrl Pts',(-9.51647500000045,-0.265706620582239,
28.7670579008196));
#17557=CARTESIAN_POINT('Ctrl Pts',(-9.40727465387286,-0.529786878175576,
28.7795388340678));
#17558=CARTESIAN_POINT('Ctrl Pts',(-9.2196169190788,-0.71789478017362,28.792019767316));
#17559=CARTESIAN_POINT('Ctrl Pts',(-9.03195918428474,-0.906002682171665,
28.8045007005642));
#17560=CARTESIAN_POINT('Ctrl Pts',(-8.76814132834533,-1.01583545019868,
28.8169816338124));
#17561=CARTESIAN_POINT('Ctrl Pts',(-8.50243547044659,-1.01647208230659,
28.8294625670606));
#17562=CARTESIAN_POINT('Ctrl Pts',(-8.23672961254786,-1.01710871441451,
28.8419435003088));
#17563=CARTESIAN_POINT('Ctrl Pts',(-7.97238846933477,-0.908541417083576,
28.854424433557));
#17564=CARTESIAN_POINT('Ctrl Pts',(-7.78383148002453,-0.721334926799713,
28.8669053668052));
#17565=CARTESIAN_POINT('Ctrl Pts',(-7.5952744907143,-0.534128436515849,
28.8793863000533));
#17566=CARTESIAN_POINT('Ctrl Pts',(-7.48480993131747,-0.270574496757375,
28.8918672333015));
#17567=CARTESIAN_POINT('Ctrl Pts',(-7.48353667075687,-0.00487092690990858,
28.9043481665497));
#17568=CARTESIAN_POINT('Ctrl Pts',(-7.48226341019626,0.260832642937558,
28.9168290997979));
#17569=CARTESIAN_POINT('Ctrl Pts',(-7.59019703546664,0.525433154238916,
28.9293100330461));
#17570=CARTESIAN_POINT('Ctrl Pts',(-7.77695120652398,0.714438148392058,
28.9417909662943));
#17571=CARTESIAN_POINT('Ctrl Pts',(-7.96370537758132,0.9034431425452,28.9542718995425));
#17572=CARTESIAN_POINT('Ctrl Pts',(-8.22699388814654,1.01453885915612,28.9667528327907));
#17573=CARTESIAN_POINT('Ctrl Pts',(-8.49269364458983,1.01644874085987,28.9792337660389));
#17574=CARTESIAN_POINT('Ctrl Pts',(-8.75839340103311,1.01835862256363,28.991714699287));
#17575=CARTESIAN_POINT('Ctrl Pts',(-9.02325176140227,0.911059288979904,
29.0041956325352));
#17576=CARTESIAN_POINT('Ctrl Pts',(-9.21270367535712,0.724758509268745,
29.0166765657834));
#17577=CARTESIAN_POINT('Ctrl Pts',(-9.40215558931197,0.538457729557587,
29.0291574990316));
#17578=CARTESIAN_POINT('Ctrl Pts',(-9.51388182535792,0.275436159674139,
29.0416384322798));
#17579=CARTESIAN_POINT('Ctrl Pts',(-9.51642831724056,0.00974174196606169,
29.054119365528));
#17580=CARTESIAN_POINT('Ctrl Pts',(-9.51645943884196,0.00649459406831602,
29.0542718995425));
#17581=CARTESIAN_POINT('Ctrl Pts',(-9.51647499999999,0.00324729703525258,
29.054424433557));
#17582=CARTESIAN_POINT('Ctrl Pts',(-9.516475,1.73256407251203E-12,29.0545769675714));
#17583=CARTESIAN_POINT('Origin',(-8.5,0.,1.24542303242842));
#17584=CARTESIAN_POINT('',(-9.516475,1.66178739415049E-12,28.3954230324284));
#17585=CARTESIAN_POINT('',(-9.51596463663996,-0.000112154843913254,28.4545769675714));
#17586=CARTESIAN_POINT('',(-9.516475,1.78524650477582E-12,1.24542303242842));
#17587=CARTESIAN_POINT('Ctrl Pts',(-9.516475,1.77734722252357E-12,28.3954230324284));
#17588=CARTESIAN_POINT('Ctrl Pts',(-9.51647500000047,-0.265706620582211,
28.4079039656766));
#17589=CARTESIAN_POINT('Ctrl Pts',(-9.40727465387286,-0.529786878175592,
28.4203848989248));
#17590=CARTESIAN_POINT('Ctrl Pts',(-9.21961691907877,-0.717894780173655,
28.432865832173));
#17591=CARTESIAN_POINT('Ctrl Pts',(-9.03195918428468,-0.906002682171718,
28.4453467654212));
#17592=CARTESIAN_POINT('Ctrl Pts',(-8.7681413283452,-1.01583545019872,28.4578276986694));
#17593=CARTESIAN_POINT('Ctrl Pts',(-8.50243547044643,-1.01647208230659,
28.4703086319176));
#17594=CARTESIAN_POINT('Ctrl Pts',(-8.23672961254766,-1.01710871441447,
28.4827895651658));
#17595=CARTESIAN_POINT('Ctrl Pts',(-7.97238846933455,-0.908541417083458,
28.4952704984139));
#17596=CARTESIAN_POINT('Ctrl Pts',(-7.78383148002433,-0.721334926799516,
28.5077514316621));
#17597=CARTESIAN_POINT('Ctrl Pts',(-7.59527449071412,-0.534128436515573,
28.5202323649103));
#17598=CARTESIAN_POINT('Ctrl Pts',(-7.48480993131737,-0.270574496757019,
28.5327132981585));
#17599=CARTESIAN_POINT('Ctrl Pts',(-7.48353667075686,-0.00487092690951304,
28.5451942314067));
#17600=CARTESIAN_POINT('Ctrl Pts',(-7.48226341019636,0.260832642937993,
28.5576751646549));
#17601=CARTESIAN_POINT('Ctrl Pts',(-7.59019703546688,0.525433154239346,
28.5701560979031));
#17602=CARTESIAN_POINT('Ctrl Pts',(-7.77695120652434,0.714438148392421,
28.5826370311513));
#17603=CARTESIAN_POINT('Ctrl Pts',(-7.9637053775818,0.903443142545497,28.5951179643995));
#17604=CARTESIAN_POINT('Ctrl Pts',(-8.22699388814713,1.01453885915629,28.6075988976477));
#17605=CARTESIAN_POINT('Ctrl Pts',(-8.49269364459045,1.01644874085988,28.6200798308959));
#17606=CARTESIAN_POINT('Ctrl Pts',(-8.75839340103378,1.01835862256347,28.6325607641441));
#17607=CARTESIAN_POINT('Ctrl Pts',(-9.0232517614029,0.911059288979549,28.6450416973922));
#17608=CARTESIAN_POINT('Ctrl Pts',(-9.21270367535765,0.724758509268225,
28.6575226306404));
#17609=CARTESIAN_POINT('Ctrl Pts',(-9.40215558931239,0.538457729556901,
28.6700035638886));
#17610=CARTESIAN_POINT('Ctrl Pts',(-9.51388182535815,0.275436159673322,
28.6824844971368));
#17611=CARTESIAN_POINT('Ctrl Pts',(-9.51642831724056,0.00974174196520395,
28.694965430385));
#17612=CARTESIAN_POINT('Ctrl Pts',(-9.51645943884196,0.0064945940677664,
28.6951179643995));
#17613=CARTESIAN_POINT('Ctrl Pts',(-9.51647499999999,0.00324729703501113,
28.6952704984139));
#17614=CARTESIAN_POINT('Ctrl Pts',(-9.516475,1.79926365491456E-12,28.6954230324284));
#17615=CARTESIAN_POINT('Ctrl Pts',(-9.51470232196842,-0.000389554669110295,
28.4545769675714));
#17616=CARTESIAN_POINT('Ctrl Pts',(-9.51530181937862,-0.130740653459931,
28.4606830615291));
#17617=CARTESIAN_POINT('Ctrl Pts',(-9.4616334089974,-0.430481838946053,
28.4747428260626));
#17618=CARTESIAN_POINT('Ctrl Pts',(-9.17050079378615,-0.816721293551335,
28.4967562611719));
#17619=CARTESIAN_POINT('Ctrl Pts',(-8.5410371348917,-1.12070821481403,28.5285709434751));
#17620=CARTESIAN_POINT('Ctrl Pts',(-7.62806957928328,-0.828287897936413,
28.5683392963542));
#17621=CARTESIAN_POINT('Ctrl Pts',(-7.33220907315438,0.286981604349355,
28.616061319809));
#17622=CARTESIAN_POINT('Ctrl Pts',(-8.10971802963793,1.13653082253137,28.6637833432638));
#17623=CARTESIAN_POINT('Ctrl Pts',(-9.20823837075766,0.950128537031716,
28.7099552258513));
#17624=CARTESIAN_POINT('Ctrl Pts',(-9.51583879936752,0.303640361218014,
28.7402197672872));
#17625=CARTESIAN_POINT('Ctrl Pts',(-9.5178552445993,-0.000844182403807882,
28.7545769675715));
#17626=CARTESIAN_POINT('Origin',(-8.5,0.,1.24542303242842));
#17627=CARTESIAN_POINT('',(-9.5167407851321,1.32517023624598E-5,28.0954230324284));
#17628=CARTESIAN_POINT('',(-9.516475,1.66681477533907E-12,28.1545769675714));
#17629=CARTESIAN_POINT('',(-9.516475,1.78524650477582E-12,1.24542303242842));
#17630=CARTESIAN_POINT('Ctrl Pts',(-9.51800967957185,7.65171274508918E-5,
28.0954230324284));
#17631=CARTESIAN_POINT('Ctrl Pts',(-9.51765220615975,-0.332868200880708,
28.1111343373136));
#17632=CARTESIAN_POINT('Ctrl Pts',(-9.15838448307071,-1.00358273601128,
28.1427529833504));
#17633=CARTESIAN_POINT('Ctrl Pts',(-8.01331019109225,-1.09975294067858,
28.1902789705388));
#17634=CARTESIAN_POINT('Ctrl Pts',(-7.43080495083982,-0.338367989046775,
28.2300473234179));
#17635=CARTESIAN_POINT('Ctrl Pts',(-7.50531901190296,0.356671722620504,
28.2618620057211));
#17636=CARTESIAN_POINT('Ctrl Pts',(-7.88944826933002,0.940689924117418,
28.2936766880244));
#17637=CARTESIAN_POINT('Ctrl Pts',(-8.8230477467519,1.15843154909714,28.3334450409034));
#17638=CARTESIAN_POINT('Ctrl Pts',(-9.45630261489437,0.541449066543569,
28.3700117125634));
#17639=CARTESIAN_POINT('Ctrl Pts',(-9.51678407727377,0.102067591494495,
28.3906710430717));
#17640=CARTESIAN_POINT('Ctrl Pts',(-9.51592367502213,0.000791130475659388,
28.3954230324284));
#17641=CARTESIAN_POINT('Ctrl Pts',(-9.516475,1.78237460371215E-12,28.1545769675714));
#17642=CARTESIAN_POINT('Ctrl Pts',(-9.51647500000047,-0.265706620582167,
28.1670579008196));
#17643=CARTESIAN_POINT('Ctrl Pts',(-9.4072746538729,-0.529786878175512,
28.1795388340678));
#17644=CARTESIAN_POINT('Ctrl Pts',(-9.21961691907885,-0.717894780173569,
28.192019767316));
#17645=CARTESIAN_POINT('Ctrl Pts',(-9.03195918428481,-0.906002682171627,
28.2045007005642));
#17646=CARTESIAN_POINT('Ctrl Pts',(-8.7681413283454,-1.01583545019866,28.2169816338124));
#17647=CARTESIAN_POINT('Ctrl Pts',(-8.50243547044666,-1.01647208230659,
28.2294625670606));
#17648=CARTESIAN_POINT('Ctrl Pts',(-8.23672961254793,-1.01710871441453,
28.2419435003088));
#17649=CARTESIAN_POINT('Ctrl Pts',(-7.97238846933483,-0.908541417083614,
28.254424433557));
#17650=CARTESIAN_POINT('Ctrl Pts',(-7.78383148002458,-0.721334926799763,
28.2669053668051));
#17651=CARTESIAN_POINT('Ctrl Pts',(-7.59527449071433,-0.534128436515913,
28.2793863000533));
#17652=CARTESIAN_POINT('Ctrl Pts',(-7.48480993131749,-0.270574496757447,
28.2918672333015));
#17653=CARTESIAN_POINT('Ctrl Pts',(-7.48353667075687,-0.00487092690998031,
28.3043481665497));
#17654=CARTESIAN_POINT('Ctrl Pts',(-7.48226341019624,0.260832642937486,
28.3168290997979));
#17655=CARTESIAN_POINT('Ctrl Pts',(-7.5901970354666,0.525433154238852,28.3293100330461));
#17656=CARTESIAN_POINT('Ctrl Pts',(-7.77695120652393,0.714438148392007,
28.3417909662943));
#17657=CARTESIAN_POINT('Ctrl Pts',(-7.96370537758126,0.903443142545162,
28.3542718995425));
#17658=CARTESIAN_POINT('Ctrl Pts',(-8.22699388814647,1.0145388591561,28.3667528327907));
#17659=CARTESIAN_POINT('Ctrl Pts',(-8.49269364458975,1.01644874085987,28.3792337660389));
#17660=CARTESIAN_POINT('Ctrl Pts',(-8.75839340103304,1.01835862256364,28.391714699287));
#17661=CARTESIAN_POINT('Ctrl Pts',(-9.0232517614022,0.911059288979941,28.4041956325352));
#17662=CARTESIAN_POINT('Ctrl Pts',(-9.21270367535707,0.724758509268796,
28.4166765657834));
#17663=CARTESIAN_POINT('Ctrl Pts',(-9.40215558931193,0.53845772955765,28.4291574990316));
#17664=CARTESIAN_POINT('Ctrl Pts',(-9.5138818253579,0.275436159674211,28.4416384322798));
#17665=CARTESIAN_POINT('Ctrl Pts',(-9.51642831724055,0.00974174196613341,
28.454119365528));
#17666=CARTESIAN_POINT('Ctrl Pts',(-9.51645943884196,0.00649459406834922,
28.4542718995425));
#17667=CARTESIAN_POINT('Ctrl Pts',(-9.51647499999999,0.00324729703524735,
28.454424433557));
#17668=CARTESIAN_POINT('Ctrl Pts',(-9.516475,1.68873120773006E-12,28.4545769675714));
#17669=CARTESIAN_POINT('Origin',(-8.5,0.,1.24542303242842));
#17670=CARTESIAN_POINT('',(-9.516475,1.61795452936852E-12,27.7954230324284));
#17671=CARTESIAN_POINT('',(-9.51669945074544,6.82738928919885E-5,27.8545769675714));
#17672=CARTESIAN_POINT('',(-9.516475,1.78524650477582E-12,1.24542303242842));
#17673=CARTESIAN_POINT('Ctrl Pts',(-9.516475,1.7335143577416E-12,27.7954230324284));
#17674=CARTESIAN_POINT('Ctrl Pts',(-9.51647500000045,-0.265706620582254,
27.8079039656766));
#17675=CARTESIAN_POINT('Ctrl Pts',(-9.40727465387284,-0.529786878175631,
27.8203848989248));
#17676=CARTESIAN_POINT('Ctrl Pts',(-9.21961691907874,-0.717894780173686,
27.832865832173));
#17677=CARTESIAN_POINT('Ctrl Pts',(-9.03195918428464,-0.906002682171741,
27.8453467654212));
#17678=CARTESIAN_POINT('Ctrl Pts',(-8.76814132834516,-1.01583545019873,
27.8578276986694));
#17679=CARTESIAN_POINT('Ctrl Pts',(-8.50243547044638,-1.01647208230659,
27.8703086319176));
#17680=CARTESIAN_POINT('Ctrl Pts',(-8.23672961254761,-1.01710871441446,
27.8827895651658));
#17681=CARTESIAN_POINT('Ctrl Pts',(-7.97238846933451,-0.908541417083436,
27.895270498414));
#17682=CARTESIAN_POINT('Ctrl Pts',(-7.7838314800243,-0.721334926799485,
27.9077514316621));
#17683=CARTESIAN_POINT('Ctrl Pts',(-7.5952744907141,-0.534128436515534,
27.9202323649103));
#17684=CARTESIAN_POINT('Ctrl Pts',(-7.48480993131736,-0.270574496756975,
27.9327132981585));
#17685=CARTESIAN_POINT('Ctrl Pts',(-7.48353667075686,-0.00487092690946921,
27.9451942314067));
#17686=CARTESIAN_POINT('Ctrl Pts',(-7.48226341019637,0.260832642938037,
27.9576751646549));
#17687=CARTESIAN_POINT('Ctrl Pts',(-7.5901970354669,0.525433154239385,27.9701560979031));
#17688=CARTESIAN_POINT('Ctrl Pts',(-7.77695120652437,0.714438148392453,
27.9826370311513));
#17689=CARTESIAN_POINT('Ctrl Pts',(-7.96370537758184,0.90344314254552,27.9951179643995));
#17690=CARTESIAN_POINT('Ctrl Pts',(-8.22699388814717,1.0145388591563,28.0075988976477));
#17691=CARTESIAN_POINT('Ctrl Pts',(-8.4926936445905,1.01644874085988,28.0200798308959));
#17692=CARTESIAN_POINT('Ctrl Pts',(-8.75839340103382,1.01835862256346,28.0325607641441));
#17693=CARTESIAN_POINT('Ctrl Pts',(-9.02325176140294,0.911059288979527,
28.0450416973922));
#17694=CARTESIAN_POINT('Ctrl Pts',(-9.21270367535768,0.724758509268194,
28.0575226306404));
#17695=CARTESIAN_POINT('Ctrl Pts',(-9.40215558931241,0.538457729556862,
28.0700035638886));
#17696=CARTESIAN_POINT('Ctrl Pts',(-9.51388182535816,0.275436159673279,
28.0824844971368));
#17697=CARTESIAN_POINT('Ctrl Pts',(-9.51642831724056,0.00974174196516012,
28.094965430385));
#17698=CARTESIAN_POINT('Ctrl Pts',(-9.51645943884196,0.00649459406768405,
28.0951179643995));
#17699=CARTESIAN_POINT('Ctrl Pts',(-9.51647499999999,0.00324729703489034,
28.095270498414));
#17700=CARTESIAN_POINT('Ctrl Pts',(-9.516475,1.63987096175951E-12,28.0954230324284));
#17701=CARTESIAN_POINT('Ctrl Pts',(-9.51761484906871,0.000346721644969969,
27.8545769675714));
#17702=CARTESIAN_POINT('Ctrl Pts',(-9.51603164570953,-0.322453934885924,
27.8697949677096));
#17703=CARTESIAN_POINT('Ctrl Pts',(-9.17770066316481,-0.98391483713693,
27.9009203089995));
#17704=CARTESIAN_POINT('Ctrl Pts',(-8.04802974380756,-1.1143684208142,27.9479529914409));
#17705=CARTESIAN_POINT('Ctrl Pts',(-7.31915026362204,-0.222747002236805,
27.9956750148958));
#17706=CARTESIAN_POINT('Ctrl Pts',(-7.67312128813442,0.873135548270785,
28.0433970383507));
#17707=CARTESIAN_POINT('Ctrl Pts',(-8.78880236016895,1.16744023289704,28.0911190618055));
#17708=CARTESIAN_POINT('Ctrl Pts',(-9.44635199105584,0.562681634430224,
28.1281790382124));
#17709=CARTESIAN_POINT('Ctrl Pts',(-9.51666892397189,0.112429099594727,
28.1493316734677));
#17710=CARTESIAN_POINT('Ctrl Pts',(-9.5160973699535,0.000575295411255838,
28.1545769675714));
#17711=CARTESIAN_POINT('Origin',(-8.5,0.,1.24542303242842));
#17712=CARTESIAN_POINT('',(-9.516475,1.59603809697754E-12,27.4954230324284));
#17713=CARTESIAN_POINT('',(-9.516475,1.6229819105571E-12,27.5545769675714));
#17714=CARTESIAN_POINT('',(-9.516475,1.78524650477582E-12,1.24542303242842));
#17715=CARTESIAN_POINT('Ctrl Pts',(-9.516475,1.59603809697754E-12,27.4954230324284));
#17716=CARTESIAN_POINT('Ctrl Pts',(-9.51647500000042,-0.26570662058243,
27.5079039656766));
#17717=CARTESIAN_POINT('Ctrl Pts',(-9.40727465387273,-0.52978687817583,
27.5203848989248));
#17718=CARTESIAN_POINT('Ctrl Pts',(-9.21961691907856,-0.717894780173865,
27.532865832173));
#17719=CARTESIAN_POINT('Ctrl Pts',(-9.03195918428438,-0.9060026821719,27.5453467654212));
#17720=CARTESIAN_POINT('Ctrl Pts',(-8.76814132834483,-1.01583545019883,
27.5578276986694));
#17721=CARTESIAN_POINT('Ctrl Pts',(-8.50243547044602,-1.0164720823066,27.5703086319176));
#17722=CARTESIAN_POINT('Ctrl Pts',(-8.23672961254721,-1.01710871441436,
27.5827895651658));
#17723=CARTESIAN_POINT('Ctrl Pts',(-7.9723884693341,-0.908541417083211,
27.595270498414));
#17724=CARTESIAN_POINT('Ctrl Pts',(-7.78383148002396,-0.721334926799144,
27.6077514316622));
#17725=CARTESIAN_POINT('Ctrl Pts',(-7.59527449071382,-0.534128436515076,
27.6202323649104));
#17726=CARTESIAN_POINT('Ctrl Pts',(-7.4848099313172,-0.270574496756415,
27.6327132981586));
#17727=CARTESIAN_POINT('Ctrl Pts',(-7.48353667075686,-0.0048709269088695,
27.6451942314067));
#17728=CARTESIAN_POINT('Ctrl Pts',(-7.48226341019652,0.260832642938676,
27.6576751646549));
#17729=CARTESIAN_POINT('Ctrl Pts',(-7.59019703546725,0.525433154239998,
27.6701560979031));
#17730=CARTESIAN_POINT('Ctrl Pts',(-7.77695120652487,0.714438148392961,
27.6826370311513));
#17731=CARTESIAN_POINT('Ctrl Pts',(-7.9637053775825,0.903443142545925,27.6951179643995));
#17732=CARTESIAN_POINT('Ctrl Pts',(-8.22699388814796,1.01453885915652,27.7075988976477));
#17733=CARTESIAN_POINT('Ctrl Pts',(-8.49269364459133,1.01644874085988,27.7200798308959));
#17734=CARTESIAN_POINT('Ctrl Pts',(-8.75839340103469,1.01835862256324,27.7325607641441));
#17735=CARTESIAN_POINT('Ctrl Pts',(-9.02325176140376,0.911059288979067,
27.7450416973923));
#17736=CARTESIAN_POINT('Ctrl Pts',(-9.21270367535835,0.724758509267531,
27.7575226306405));
#17737=CARTESIAN_POINT('Ctrl Pts',(-9.40215558931294,0.538457729555995,
27.7700035638887));
#17738=CARTESIAN_POINT('Ctrl Pts',(-9.51388182535845,0.275436159672258,
27.7824844971369));
#17739=CARTESIAN_POINT('Ctrl Pts',(-9.51642831724057,0.00974174196409821,
27.7949654303851));
#17740=CARTESIAN_POINT('Ctrl Pts',(-9.51645943884197,0.00649459406700729,
27.7951179643995));
#17741=CARTESIAN_POINT('Ctrl Pts',(-9.51647499999999,0.0032472970345988,
27.795270498414));
#17742=CARTESIAN_POINT('Ctrl Pts',(-9.516475,1.7335143577416E-12,27.7954230324284));
#17743=CARTESIAN_POINT('Ctrl Pts',(-9.516475,1.6229819105571E-12,27.5545769675714));
#17744=CARTESIAN_POINT('Ctrl Pts',(-9.51647500000042,-0.265706620582365,
27.5670579008196));
#17745=CARTESIAN_POINT('Ctrl Pts',(-9.40727465387278,-0.52978687817573,
27.5795388340678));
#17746=CARTESIAN_POINT('Ctrl Pts',(-9.21961691907866,-0.717894780173764,
27.592019767316));
#17747=CARTESIAN_POINT('Ctrl Pts',(-9.03195918428454,-0.906002682171798,
27.6045007005642));
#17748=CARTESIAN_POINT('Ctrl Pts',(-8.76814132834505,-1.01583545019876,
27.6169816338124));
#17749=CARTESIAN_POINT('Ctrl Pts',(-8.50243547044627,-1.01647208230659,
27.6294625670606));
#17750=CARTESIAN_POINT('Ctrl Pts',(-8.2367296125475,-1.01710871441443,27.6419435003088));
#17751=CARTESIAN_POINT('Ctrl Pts',(-7.97238846933441,-0.908541417083378,
27.654424433557));
#17752=CARTESIAN_POINT('Ctrl Pts',(-7.78383148002422,-0.721334926799407,
27.6669053668052));
#17753=CARTESIAN_POINT('Ctrl Pts',(-7.59527449071404,-0.534128436515436,
27.6793863000534));
#17754=CARTESIAN_POINT('Ctrl Pts',(-7.48480993131733,-0.270574496756865,
27.6918672333016));
#17755=CARTESIAN_POINT('Ctrl Pts',(-7.48353667075686,-0.00487092690935868,
27.7043481665497));
#17756=CARTESIAN_POINT('Ctrl Pts',(-7.4822634101964,0.260832642938147,27.7168290997979));
#17757=CARTESIAN_POINT('Ctrl Pts',(-7.59019703546696,0.525433154239484,
27.7293100330461));
#17758=CARTESIAN_POINT('Ctrl Pts',(-7.77695120652445,0.714438148392531,
27.7417909662943));
#17759=CARTESIAN_POINT('Ctrl Pts',(-7.96370537758194,0.903443142545578,
27.7542718995425));
#17760=CARTESIAN_POINT('Ctrl Pts',(-8.22699388814728,1.01453885915633,27.7667528327907));
#17761=CARTESIAN_POINT('Ctrl Pts',(-8.49269364459061,1.01644874085988,27.7792337660389));
#17762=CARTESIAN_POINT('Ctrl Pts',(-8.75839340103393,1.01835862256343,27.7917146992871));
#17763=CARTESIAN_POINT('Ctrl Pts',(-9.02325176140304,0.91105928897947,27.8041956325353));
#17764=CARTESIAN_POINT('Ctrl Pts',(-9.21270367535776,0.724758509268117,
27.8166765657835));
#17765=CARTESIAN_POINT('Ctrl Pts',(-9.40215558931247,0.538457729556764,
27.8291574990317));
#17766=CARTESIAN_POINT('Ctrl Pts',(-9.51388182535819,0.275436159673168,
27.8416384322799));
#17767=CARTESIAN_POINT('Ctrl Pts',(-9.51642831724056,0.00974174196504959,
27.854119365528));
#17768=CARTESIAN_POINT('Ctrl Pts',(-9.51645943884196,0.00649459406765055,
27.8542718995425));
#17769=CARTESIAN_POINT('Ctrl Pts',(-9.51647499999999,0.00324729703493389,
27.854424433557));
#17770=CARTESIAN_POINT('Ctrl Pts',(-9.516475,1.76045817132117E-12,27.8545769675714));
#17771=CARTESIAN_POINT('Origin',(-8.5,0.,1.24542303242842));
#17772=CARTESIAN_POINT('',(-9.516475,1.57412166458655E-12,27.1954230324284));
#17773=CARTESIAN_POINT('',(-9.516475,1.60106547816612E-12,27.2545769675714));
#17774=CARTESIAN_POINT('',(-9.516475,1.78524650477582E-12,1.24542303242842));
#17775=CARTESIAN_POINT('Ctrl Pts',(-9.516475,1.57412166458655E-12,27.1954230324284));
#17776=CARTESIAN_POINT('Ctrl Pts',(-9.51647500000041,-0.265706620582452,
27.2079039656766));
#17777=CARTESIAN_POINT('Ctrl Pts',(-9.40727465387272,-0.529786878175849,
27.2203848989248));
#17778=CARTESIAN_POINT('Ctrl Pts',(-9.21961691907854,-0.71789478017388,
27.232865832173));
#17779=CARTESIAN_POINT('Ctrl Pts',(-9.03195918428436,-0.906002682171912,
27.2453467654212));
#17780=CARTESIAN_POINT('Ctrl Pts',(-8.7681413283448,-1.01583545019883,27.2578276986694));
#17781=CARTESIAN_POINT('Ctrl Pts',(-8.50243547044599,-1.0164720823066,27.2703086319176));
#17782=CARTESIAN_POINT('Ctrl Pts',(-8.23672961254718,-1.01710871441436,
27.2827895651658));
#17783=CARTESIAN_POINT('Ctrl Pts',(-7.97238846933408,-0.9085414170832,27.295270498414));
#17784=CARTESIAN_POINT('Ctrl Pts',(-7.78383148002394,-0.721334926799128,
27.3077514316622));
#17785=CARTESIAN_POINT('Ctrl Pts',(-7.59527449071381,-0.534128436515056,
27.3202323649104));
#17786=CARTESIAN_POINT('Ctrl Pts',(-7.48480993131719,-0.270574496756393,
27.3327132981586));
#17787=CARTESIAN_POINT('Ctrl Pts',(-7.48353667075686,-0.00487092690884759,
27.3451942314067));
#17788=CARTESIAN_POINT('Ctrl Pts',(-7.48226341019653,0.260832642938698,
27.3576751646549));
#17789=CARTESIAN_POINT('Ctrl Pts',(-7.59019703546726,0.525433154240017,
27.3701560979031));
#17790=CARTESIAN_POINT('Ctrl Pts',(-7.77695120652489,0.714438148392977,
27.3826370311513));
#17791=CARTESIAN_POINT('Ctrl Pts',(-7.96370537758252,0.903443142545937,
27.3951179643995));
#17792=CARTESIAN_POINT('Ctrl Pts',(-8.22699388814799,1.01453885915653,27.4075988976477));
#17793=CARTESIAN_POINT('Ctrl Pts',(-8.49269364459135,1.01644874085988,27.4200798308959));
#17794=CARTESIAN_POINT('Ctrl Pts',(-8.75839340103471,1.01835862256324,27.4325607641441));
#17795=CARTESIAN_POINT('Ctrl Pts',(-9.02325176140378,0.911059288979055,
27.4450416973923));
#17796=CARTESIAN_POINT('Ctrl Pts',(-9.21270367535837,0.724758509267516,
27.4575226306405));
#17797=CARTESIAN_POINT('Ctrl Pts',(-9.40215558931296,0.538457729555976,
27.4700035638887));
#17798=CARTESIAN_POINT('Ctrl Pts',(-9.51388182535846,0.275436159672236,
27.4824844971369));
#17799=CARTESIAN_POINT('Ctrl Pts',(-9.51642831724057,0.00974174196407629,
27.4949654303851));
#17800=CARTESIAN_POINT('Ctrl Pts',(-9.51645943884197,0.00649459406694685,
27.4951179643995));
#17801=CARTESIAN_POINT('Ctrl Pts',(-9.51647499999999,0.00324729703449976,
27.495270498414));
#17802=CARTESIAN_POINT('Ctrl Pts',(-9.516475,1.59603809697754E-12,27.4954230324284));
#17803=CARTESIAN_POINT('Ctrl Pts',(-9.516475,1.60106547816612E-12,27.2545769675714));
#17804=CARTESIAN_POINT('Ctrl Pts',(-9.51647500000042,-0.265706620582425,
27.2670579008196));
#17805=CARTESIAN_POINT('Ctrl Pts',(-9.40727465387274,-0.529786878175825,
27.2795388340678));
#17806=CARTESIAN_POINT('Ctrl Pts',(-9.21961691907856,-0.717894780173861,
27.292019767316));
#17807=CARTESIAN_POINT('Ctrl Pts',(-9.03195918428439,-0.906002682171897,
27.3045007005642));
#17808=CARTESIAN_POINT('Ctrl Pts',(-8.76814132834483,-1.01583545019883,
27.3169816338124));
#17809=CARTESIAN_POINT('Ctrl Pts',(-8.50243547044602,-1.0164720823066,27.3294625670606));
#17810=CARTESIAN_POINT('Ctrl Pts',(-8.23672961254721,-1.01710871441436,
27.3419435003088));
#17811=CARTESIAN_POINT('Ctrl Pts',(-7.97238846933411,-0.908541417083214,
27.354424433557));
#17812=CARTESIAN_POINT('Ctrl Pts',(-7.78383148002396,-0.721334926799147,
27.3669053668052));
#17813=CARTESIAN_POINT('Ctrl Pts',(-7.59527449071382,-0.53412843651508,
27.3793863000534));
#17814=CARTESIAN_POINT('Ctrl Pts',(-7.4848099313172,-0.27057449675642,27.3918672333016));
#17815=CARTESIAN_POINT('Ctrl Pts',(-7.48353667075686,-0.00487092690887453,
27.4043481665498));
#17816=CARTESIAN_POINT('Ctrl Pts',(-7.48226341019652,0.260832642938671,
27.416829099798));
#17817=CARTESIAN_POINT('Ctrl Pts',(-7.59019703546724,0.525433154239993,
27.4293100330462));
#17818=CARTESIAN_POINT('Ctrl Pts',(-7.77695120652487,0.714438148392958,
27.4417909662943));
#17819=CARTESIAN_POINT('Ctrl Pts',(-7.9637053775825,0.903443142545922,27.4542718995425));
#17820=CARTESIAN_POINT('Ctrl Pts',(-8.22699388814796,1.01453885915652,27.4667528327907));
#17821=CARTESIAN_POINT('Ctrl Pts',(-8.49269364459132,1.01644874085988,27.4792337660389));
#17822=CARTESIAN_POINT('Ctrl Pts',(-8.75839340103469,1.01835862256325,27.4917146992871));
#17823=CARTESIAN_POINT('Ctrl Pts',(-9.02325176140376,0.911059288979069,
27.5041956325353));
#17824=CARTESIAN_POINT('Ctrl Pts',(-9.21270367535835,0.724758509267534,
27.5166765657835));
#17825=CARTESIAN_POINT('Ctrl Pts',(-9.40215558931294,0.538457729555999,
27.5291574990317));
#17826=CARTESIAN_POINT('Ctrl Pts',(-9.51388182535845,0.275436159672263,
27.5416384322799));
#17827=CARTESIAN_POINT('Ctrl Pts',(-9.51642831724057,0.00974174196410324,
27.5541193655281));
#17828=CARTESIAN_POINT('Ctrl Pts',(-9.51645943884197,0.0064945940669738,
27.5542718995425));
#17829=CARTESIAN_POINT('Ctrl Pts',(-9.51647499999999,0.0032472970345267,
27.554424433557));
#17830=CARTESIAN_POINT('Ctrl Pts',(-9.516475,1.6229819105571E-12,27.5545769675714));
#17831=CARTESIAN_POINT('Origin',(-8.5,0.,1.24542303242842));
#17832=CARTESIAN_POINT('',(-9.516475,1.55220523219556E-12,26.8954230324284));
#17833=CARTESIAN_POINT('',(-9.516475,1.57914904577513E-12,26.9545769675715));
#17834=CARTESIAN_POINT('',(-9.516475,1.78524650477582E-12,1.24542303242842));
#17835=CARTESIAN_POINT('Ctrl Pts',(-9.516475,1.55220523219556E-12,26.8954230324284));
#17836=CARTESIAN_POINT('Ctrl Pts',(-9.5164750000004,-0.26570662058232,26.9079039656766));
#17837=CARTESIAN_POINT('Ctrl Pts',(-9.40727465387284,-0.529786878175565,
26.9203848989248));
#17838=CARTESIAN_POINT('Ctrl Pts',(-9.21961691907885,-0.717894780173569,
26.932865832173));
#17839=CARTESIAN_POINT('Ctrl Pts',(-9.03195918428486,-0.906002682171572,
26.9453467654212));
#17840=CARTESIAN_POINT('Ctrl Pts',(-8.76814132834555,-1.0158354501986,26.9578276986694));
#17841=CARTESIAN_POINT('Ctrl Pts',(-8.5024354704469,-1.01647208230659,26.9703086319175));
#17842=CARTESIAN_POINT('Ctrl Pts',(-8.23672961254824,-1.01710871441459,
26.9827895651657));
#17843=CARTESIAN_POINT('Ctrl Pts',(-7.97238846933519,-0.9085414170838,26.9952704984139));
#17844=CARTESIAN_POINT('Ctrl Pts',(-7.78383148002491,-0.72133492680009,
27.0077514316621));
#17845=CARTESIAN_POINT('Ctrl Pts',(-7.59527449071463,-0.53412843651638,
27.0202323649103));
#17846=CARTESIAN_POINT('Ctrl Pts',(-7.48480993131768,-0.270574496758063,
27.0327132981585));
#17847=CARTESIAN_POINT('Ctrl Pts',(-7.48353667075687,-0.00487092691067461,
27.0451942314067));
#17848=CARTESIAN_POINT('Ctrl Pts',(-7.48226341019606,0.260832642936714,
27.0576751646548));
#17849=CARTESIAN_POINT('Ctrl Pts',(-7.59019703546618,0.525433154238078,
27.070156097903));
#17850=CARTESIAN_POINT('Ctrl Pts',(-7.77695120652328,0.714438148391349,
27.0826370311512));
#17851=CARTESIAN_POINT('Ctrl Pts',(-7.96370537758038,0.903443142544619,
27.0951179643994));
#17852=CARTESIAN_POINT('Ctrl Pts',(-8.22699388814539,1.01453885915579,27.1075988976476));
#17853=CARTESIAN_POINT('Ctrl Pts',(-8.4926936445886,1.01644874085986,27.1200798308958));
#17854=CARTESIAN_POINT('Ctrl Pts',(-8.7583934010318,1.01835862256394,27.132560764144));
#17855=CARTESIAN_POINT('Ctrl Pts',(-9.02325176140101,0.911059288980602,
27.1450416973921));
#17856=CARTESIAN_POINT('Ctrl Pts',(-9.21270367535608,0.724758509269769,
27.1575226306403));
#17857=CARTESIAN_POINT('Ctrl Pts',(-9.40215558931114,0.538457729558936,
27.1700035638885));
#17858=CARTESIAN_POINT('Ctrl Pts',(-9.51388182535746,0.275436159675749,
27.1824844971367));
#17859=CARTESIAN_POINT('Ctrl Pts',(-9.51642831724054,0.00974174196775212,
27.1949654303849));
#17860=CARTESIAN_POINT('Ctrl Pts',(-9.51645943884195,0.00649459406939021,
27.1951179643994));
#17861=CARTESIAN_POINT('Ctrl Pts',(-9.51647499999999,0.00324729703571043,
27.1952704984139));
#17862=CARTESIAN_POINT('Ctrl Pts',(-9.516475,1.57412166458655E-12,27.1954230324284));
#17863=CARTESIAN_POINT('Ctrl Pts',(-9.516475,1.57914904577513E-12,26.9545769675715));
#17864=CARTESIAN_POINT('Ctrl Pts',(-9.51647500000041,-0.265706620582332,
26.9670579008196));
#17865=CARTESIAN_POINT('Ctrl Pts',(-9.40727465387283,-0.529786878175617,
26.9795388340678));
#17866=CARTESIAN_POINT('Ctrl Pts',(-9.21961691907879,-0.717894780173631,
26.992019767316));
#17867=CARTESIAN_POINT('Ctrl Pts',(-9.03195918428476,-0.906002682171646,
27.0045007005642));
#17868=CARTESIAN_POINT('Ctrl Pts',(-8.76814132834539,-1.01583545019865,
27.0169816338124));
#17869=CARTESIAN_POINT('Ctrl Pts',(-8.50243547044669,-1.01647208230659,
27.0294625670606));
#17870=CARTESIAN_POINT('Ctrl Pts',(-8.236729612548,-1.01710871441454,27.0419435003088));
#17871=CARTESIAN_POINT('Ctrl Pts',(-7.97238846933493,-0.908541417083661,
27.054424433557));
#17872=CARTESIAN_POINT('Ctrl Pts',(-7.78383148002468,-0.721334926799864,
27.0669053668051));
#17873=CARTESIAN_POINT('Ctrl Pts',(-7.59527449071444,-0.534128436516068,
27.0793863000533));
#17874=CARTESIAN_POINT('Ctrl Pts',(-7.48480993131756,-0.270574496757667,
27.0918672333015));
#17875=CARTESIAN_POINT('Ctrl Pts',(-7.48353667075687,-0.00487092691023932,
27.1043481665497));
#17876=CARTESIAN_POINT('Ctrl Pts',(-7.48226341019617,0.260832642937188,
27.1168290997979));
#17877=CARTESIAN_POINT('Ctrl Pts',(-7.59019703546644,0.525433154238544,
27.1293100330461));
#17878=CARTESIAN_POINT('Ctrl Pts',(-7.77695120652367,0.71443814839174,27.1417909662943));
#17879=CARTESIAN_POINT('Ctrl Pts',(-7.9637053775809,0.903443142544937,27.1542718995425));
#17880=CARTESIAN_POINT('Ctrl Pts',(-8.22699388814602,1.01453885915597,27.1667528327906));
#17881=CARTESIAN_POINT('Ctrl Pts',(-8.49269364458926,1.01644874085987,27.1792337660388));
#17882=CARTESIAN_POINT('Ctrl Pts',(-8.75839340103251,1.01835862256377,27.191714699287));
#17883=CARTESIAN_POINT('Ctrl Pts',(-9.02325176140169,0.911059288980226,
27.2041956325352));
#17884=CARTESIAN_POINT('Ctrl Pts',(-9.21270367535664,0.72475850926922,27.2166765657834));
#17885=CARTESIAN_POINT('Ctrl Pts',(-9.40215558931158,0.538457729558215,
27.2291574990316));
#17886=CARTESIAN_POINT('Ctrl Pts',(-9.5138818253577,0.275436159674892,27.2416384322798));
#17887=CARTESIAN_POINT('Ctrl Pts',(-9.51642831724055,0.00974174196685463,
27.254119365528));
#17888=CARTESIAN_POINT('Ctrl Pts',(-9.51645943884196,0.00649459406880084,
27.2542718995425));
#17889=CARTESIAN_POINT('Ctrl Pts',(-9.51647499999999,0.00324729703542923,
27.254424433557));
#17890=CARTESIAN_POINT('Ctrl Pts',(-9.516475,1.60106547816612E-12,27.2545769675714));
#17891=CARTESIAN_POINT('Origin',(-8.5,0.,1.24542303242842));
#17892=CARTESIAN_POINT('',(-9.516475,1.53028879980458E-12,26.5954230324284));
#17893=CARTESIAN_POINT('',(-9.51655216780646,-3.99696456298066E-5,26.6545769675714));
#17894=CARTESIAN_POINT('',(-9.516475,1.78524650477582E-12,1.24542303242842));
#17895=CARTESIAN_POINT('Ctrl Pts',(-9.516475,1.64584862817766E-12,26.5954230324284));
#17896=CARTESIAN_POINT('Ctrl Pts',(-9.51647500000043,-0.265706620582265,
26.6079039656766));
#17897=CARTESIAN_POINT('Ctrl Pts',(-9.40727465387286,-0.529786878175558,
26.6203848989248));
#17898=CARTESIAN_POINT('Ctrl Pts',(-9.21961691907884,-0.717894780173584,
26.632865832173));
#17899=CARTESIAN_POINT('Ctrl Pts',(-9.03195918428482,-0.906002682171611,
26.6453467654212));
#17900=CARTESIAN_POINT('Ctrl Pts',(-8.76814132834545,-1.01583545019863,
26.6578276986694));
#17901=CARTESIAN_POINT('Ctrl Pts',(-8.50243547044676,-1.01647208230659,
26.6703086319175));
#17902=CARTESIAN_POINT('Ctrl Pts',(-8.23672961254806,-1.01710871441456,
26.6827895651657));
#17903=CARTESIAN_POINT('Ctrl Pts',(-7.97238846933499,-0.908541417083696,
26.6952704984139));
#17904=CARTESIAN_POINT('Ctrl Pts',(-7.78383148002473,-0.721334926799912,
26.7077514316621));
#17905=CARTESIAN_POINT('Ctrl Pts',(-7.59527449071447,-0.534128436516127,
26.7202323649103));
#17906=CARTESIAN_POINT('Ctrl Pts',(-7.48480993131758,-0.270574496757734,
26.7327132981585));
#17907=CARTESIAN_POINT('Ctrl Pts',(-7.48353667075687,-0.00487092691030601,
26.7451942314067));
#17908=CARTESIAN_POINT('Ctrl Pts',(-7.48226341019616,0.260832642937122,
26.7576751646549));
#17909=CARTESIAN_POINT('Ctrl Pts',(-7.5901970354664,0.525433154238484,26.7701560979031));
#17910=CARTESIAN_POINT('Ctrl Pts',(-7.77695120652362,0.714438148391693,
26.7826370311512));
#17911=CARTESIAN_POINT('Ctrl Pts',(-7.96370537758084,0.903443142544902,
26.7951179643994));
#17912=CARTESIAN_POINT('Ctrl Pts',(-8.22699388814596,1.01453885915595,26.8075988976476));
#17913=CARTESIAN_POINT('Ctrl Pts',(-8.4926936445892,1.01644874085987,26.8200798308958));
#17914=CARTESIAN_POINT('Ctrl Pts',(-8.75839340103244,1.01835862256379,26.832560764144));
#17915=CARTESIAN_POINT('Ctrl Pts',(-9.02325176140163,0.911059288980261,
26.8450416973922));
#17916=CARTESIAN_POINT('Ctrl Pts',(-9.21270367535659,0.724758509269267,
26.8575226306404));
#17917=CARTESIAN_POINT('Ctrl Pts',(-9.40215558931155,0.538457729558274,
26.8700035638886));
#17918=CARTESIAN_POINT('Ctrl Pts',(-9.51388182535769,0.275436159674958,
26.8824844971367));
#17919=CARTESIAN_POINT('Ctrl Pts',(-9.51642831724055,0.00974174196692133,
26.8949654303849));
#17920=CARTESIAN_POINT('Ctrl Pts',(-9.51645943884196,0.00649459406882902,
26.8951179643994));
#17921=CARTESIAN_POINT('Ctrl Pts',(-9.51647499999999,0.00324729703541897,
26.8952704984139));
#17922=CARTESIAN_POINT('Ctrl Pts',(-9.516475,1.55220523219556E-12,26.8954230324284));
#17923=CARTESIAN_POINT('Ctrl Pts',(-9.516475,1.55723261338415E-12,26.6545769675715));
#17924=CARTESIAN_POINT('Ctrl Pts',(-9.51647500000041,-0.265706620582431,
26.6670579008196));
#17925=CARTESIAN_POINT('Ctrl Pts',(-9.40727465387275,-0.529786878175788,
26.6795388340678));
#17926=CARTESIAN_POINT('Ctrl Pts',(-9.21961691907861,-0.71789478017381,
26.692019767316));
#17927=CARTESIAN_POINT('Ctrl Pts',(-9.03195918428448,-0.906002682171833,
26.7045007005642));
#17928=CARTESIAN_POINT('Ctrl Pts',(-8.76814132834498,-1.01583545019878,
26.7169816338124));
#17929=CARTESIAN_POINT('Ctrl Pts',(-8.50243547044621,-1.0164720823066,26.7294625670606));
#17930=CARTESIAN_POINT('Ctrl Pts',(-8.23672961254744,-1.01710871441441,
26.7419435003088));
#17931=CARTESIAN_POINT('Ctrl Pts',(-7.97238846933435,-0.908541417083344,
26.754424433557));
#17932=CARTESIAN_POINT('Ctrl Pts',(-7.78383148002418,-0.721334926799361,
26.7669053668052));
#17933=CARTESIAN_POINT('Ctrl Pts',(-7.59527449071401,-0.534128436515377,
26.7793863000534));
#17934=CARTESIAN_POINT('Ctrl Pts',(-7.48480993131731,-0.270574496756799,
26.7918672333016));
#17935=CARTESIAN_POINT('Ctrl Pts',(-7.48353667075686,-0.00487092690929293,
26.8043481665497));
#17936=CARTESIAN_POINT('Ctrl Pts',(-7.48226341019642,0.260832642938213,
26.8168290997979));
#17937=CARTESIAN_POINT('Ctrl Pts',(-7.59019703546699,0.525433154239543,
26.8293100330461));
#17938=CARTESIAN_POINT('Ctrl Pts',(-7.77695120652449,0.714438148392578,
26.8417909662943));
#17939=CARTESIAN_POINT('Ctrl Pts',(-7.963705377582,0.903443142545613,26.8542718995425));
#17940=CARTESIAN_POINT('Ctrl Pts',(-8.22699388814735,1.01453885915635,26.8667528327907));
#17941=CARTESIAN_POINT('Ctrl Pts',(-8.49269364459067,1.01644874085988,26.8792337660389));
#17942=CARTESIAN_POINT('Ctrl Pts',(-8.758393401034,1.01835862256341,26.8917146992871));
#17943=CARTESIAN_POINT('Ctrl Pts',(-9.0232517614031,0.911059288979436,26.9041956325353));
#17944=CARTESIAN_POINT('Ctrl Pts',(-9.2127036753578,0.724758509268071,26.9166765657835));
#17945=CARTESIAN_POINT('Ctrl Pts',(-9.40215558931251,0.538457729556705,
26.9291574990317));
#17946=CARTESIAN_POINT('Ctrl Pts',(-9.51388182535821,0.275436159673103,
26.9416384322799));
#17947=CARTESIAN_POINT('Ctrl Pts',(-9.51642831724057,0.00974174196498384,
26.954119365528));
#17948=CARTESIAN_POINT('Ctrl Pts',(-9.51645943884196,0.00649459406754628,
26.9542718995425));
#17949=CARTESIAN_POINT('Ctrl Pts',(-9.51647499999999,0.00324729703479102,
26.954424433557));
#17950=CARTESIAN_POINT('Ctrl Pts',(-9.516475,1.57914904577513E-12,26.9545769675715));
#17951=CARTESIAN_POINT('Origin',(-8.5,0.,1.24542303242842));
#17952=CARTESIAN_POINT('',(-9.516475,1.50837236741359E-12,26.2954230324284));
#17953=CARTESIAN_POINT('',(-9.51621740714814,-0.000106417722281503,26.3545769675715));
#17954=CARTESIAN_POINT('',(-9.516475,1.78524650477582E-12,1.24542303242842));
#17955=CARTESIAN_POINT('Ctrl Pts',(-9.516475,1.50837236741359E-12,26.2954230324284));
#17956=CARTESIAN_POINT('Ctrl Pts',(-9.51647500000039,-0.26570662058248,
26.3079039656766));
#17957=CARTESIAN_POINT('Ctrl Pts',(-9.40727465387272,-0.529786878175832,
26.3203848989248));
#17958=CARTESIAN_POINT('Ctrl Pts',(-9.21961691907858,-0.717894780173845,
26.332865832173));
#17959=CARTESIAN_POINT('Ctrl Pts',(-9.03195918428444,-0.906002682171858,
26.3453467654212));
#17960=CARTESIAN_POINT('Ctrl Pts',(-8.76814132834493,-1.01583545019879,
26.3578276986694));
#17961=CARTESIAN_POINT('Ctrl Pts',(-8.50243547044616,-1.0164720823066,26.3703086319176));
#17962=CARTESIAN_POINT('Ctrl Pts',(-8.23672961254739,-1.0171087144144,26.3827895651658));
#17963=CARTESIAN_POINT('Ctrl Pts',(-7.9723884693343,-0.908541417083319,
26.395270498414));
#17964=CARTESIAN_POINT('Ctrl Pts',(-7.78383148002414,-0.721334926799326,
26.4077514316622));
#17965=CARTESIAN_POINT('Ctrl Pts',(-7.59527449071398,-0.534128436515333,
26.4202323649103));
#17966=CARTESIAN_POINT('Ctrl Pts',(-7.4848099313173,-0.27057449675675,26.4327132981585));
#17967=CARTESIAN_POINT('Ctrl Pts',(-7.48353667075686,-0.00487092690924407,
26.4451942314067));
#17968=CARTESIAN_POINT('Ctrl Pts',(-7.48226341019643,0.260832642938262,
26.4576751646549));
#17969=CARTESIAN_POINT('Ctrl Pts',(-7.59019703546702,0.525433154239586,
26.4701560979031));
#17970=CARTESIAN_POINT('Ctrl Pts',(-7.77695120652453,0.714438148392613,
26.4826370311513));
#17971=CARTESIAN_POINT('Ctrl Pts',(-7.96370537758204,0.903443142545639,
26.4951179643995));
#17972=CARTESIAN_POINT('Ctrl Pts',(-8.2269938881474,1.01453885915636,26.5075988976477));
#17973=CARTESIAN_POINT('Ctrl Pts',(-8.49269364459072,1.01644874085988,26.5200798308959));
#17974=CARTESIAN_POINT('Ctrl Pts',(-8.75839340103405,1.0183586225634,26.5325607641441));
#17975=CARTESIAN_POINT('Ctrl Pts',(-9.02325176140315,0.911059288979411,
26.5450416973923));
#17976=CARTESIAN_POINT('Ctrl Pts',(-9.21270367535784,0.724758509268037,
26.5575226306404));
#17977=CARTESIAN_POINT('Ctrl Pts',(-9.40215558931254,0.538457729556662,
26.5700035638886));
#17978=CARTESIAN_POINT('Ctrl Pts',(-9.51388182535822,0.275436159673054,
26.5824844971368));
#17979=CARTESIAN_POINT('Ctrl Pts',(-9.51642831724057,0.00974174196493498,
26.594965430385));
#17980=CARTESIAN_POINT('Ctrl Pts',(-9.51645943884196,0.00649459406753594,
26.5951179643995));
#17981=CARTESIAN_POINT('Ctrl Pts',(-9.51647499999999,0.00324729703481928,
26.595270498414));
#17982=CARTESIAN_POINT('Ctrl Pts',(-9.516475,1.64584862817766E-12,26.5954230324284));
#17983=CARTESIAN_POINT('Ctrl Pts',(-9.5152075092142,-0.000523630537313469,
26.3545769675714));
#17984=CARTESIAN_POINT('Ctrl Pts',(-9.51594088723012,-0.132523029843183,
26.3607600508578));
#17985=CARTESIAN_POINT('Ctrl Pts',(-9.43067022437642,-0.60331137049921,
26.3828504752957));
#17986=CARTESIAN_POINT('Ctrl Pts',(-8.71771879103822,-1.18276034286521,
26.4208482408854));
#17987=CARTESIAN_POINT('Ctrl Pts',(-7.80744356640935,-0.882063793301015,
26.4606165937644));
#17988=CARTESIAN_POINT('Ctrl Pts',(-7.47730934038002,-0.265911264380824,
26.4924312760676));
#17989=CARTESIAN_POINT('Ctrl Pts',(-7.4655089049693,0.433011689752842,26.5242459583709));
#17990=CARTESIAN_POINT('Ctrl Pts',(-8.11403107601491,1.13901338462003,26.5640143112499));
#17991=CARTESIAN_POINT('Ctrl Pts',(-9.21176260908216,0.946387668608936,
26.6101092045087));
#17992=CARTESIAN_POINT('Ctrl Pts',(-9.51556036565569,0.302366890868681,
26.6402967566159));
#17993=CARTESIAN_POINT('Ctrl Pts',(-9.51759585434001,-0.000580554954882254,
26.6545769675714));
#17994=CARTESIAN_POINT('Origin',(-8.5,0.,1.24542303242842));
#17995=CARTESIAN_POINT('',(-9.516475,1.48645593502261E-12,25.9954230324284));
#17996=CARTESIAN_POINT('',(-9.516475,1.51339974860218E-12,26.0545769675715));
#17997=CARTESIAN_POINT('',(-9.516475,1.78524650477582E-12,1.24542303242842));
#17998=CARTESIAN_POINT('Ctrl Pts',(-9.516475,1.48645593502261E-12,25.9954230324284));
#17999=CARTESIAN_POINT('Ctrl Pts',(-9.51647500000039,-0.265706620582424,
26.0079039656766));
#18000=CARTESIAN_POINT('Ctrl Pts',(-9.40727465387278,-0.5297868781757,26.0203848989248));
#18001=CARTESIAN_POINT('Ctrl Pts',(-9.21961691907873,-0.717894780173697,
26.032865832173));
#18002=CARTESIAN_POINT('Ctrl Pts',(-9.03195918428468,-0.906002682171694,
26.0453467654212));
#18003=CARTESIAN_POINT('Ctrl Pts',(-8.76814132834529,-1.01583545019867,
26.0578276986694));
#18004=CARTESIAN_POINT('Ctrl Pts',(-8.5024354704466,-1.01647208230659,26.0703086319176));
#18005=CARTESIAN_POINT('Ctrl Pts',(-8.2367296125479,-1.01710871441451,26.0827895651657));
#18006=CARTESIAN_POINT('Ctrl Pts',(-7.97238846933485,-0.908541417083613,
26.0952704984139));
#18007=CARTESIAN_POINT('Ctrl Pts',(-7.78383148002462,-0.721334926799799,
26.1077514316621));
#18008=CARTESIAN_POINT('Ctrl Pts',(-7.59527449071439,-0.534128436515985,
26.1202323649103));
#18009=CARTESIAN_POINT('Ctrl Pts',(-7.48480993131754,-0.270574496757575,
26.1327132981585));
#18010=CARTESIAN_POINT('Ctrl Pts',(-7.48353667075687,-0.00487092691014662,
26.1451942314067));
#18011=CARTESIAN_POINT('Ctrl Pts',(-7.4822634101962,0.260832642937281,26.1576751646549));
#18012=CARTESIAN_POINT('Ctrl Pts',(-7.59019703546649,0.525433154238627,
26.1701560979031));
#18013=CARTESIAN_POINT('Ctrl Pts',(-7.77695120652373,0.714438148391806,
26.1826370311512));
#18014=CARTESIAN_POINT('Ctrl Pts',(-7.96370537758098,0.903443142544986,
26.1951179643994));
#18015=CARTESIAN_POINT('Ctrl Pts',(-8.22699388814611,1.01453885915599,26.2075988976476));
#18016=CARTESIAN_POINT('Ctrl Pts',(-8.49269364458936,1.01644874085987,26.2200798308958));
#18017=CARTESIAN_POINT('Ctrl Pts',(-8.7583934010326,1.01835862256374,26.232560764144));
#18018=CARTESIAN_POINT('Ctrl Pts',(-9.02325176140177,0.911059288980179,
26.2450416973922));
#18019=CARTESIAN_POINT('Ctrl Pts',(-9.2127036753567,0.724758509269156,26.2575226306404));
#18020=CARTESIAN_POINT('Ctrl Pts',(-9.40215558931163,0.538457729558133,
26.2700035638886));
#18021=CARTESIAN_POINT('Ctrl Pts',(-9.51388182535773,0.275436159674799,
26.2824844971367));
#18022=CARTESIAN_POINT('Ctrl Pts',(-9.51642831724055,0.00974174196676194,
26.2949654303849));
#18023=CARTESIAN_POINT('Ctrl Pts',(-9.51645943884196,0.00649459406870815,
26.2951179643994));
#18024=CARTESIAN_POINT('Ctrl Pts',(-9.51647499999999,0.00324729703533653,
26.2952704984139));
#18025=CARTESIAN_POINT('Ctrl Pts',(-9.516475,1.50837236741359E-12,26.2954230324284));
#18026=CARTESIAN_POINT('Ctrl Pts',(-9.516475,1.62895957697526E-12,26.0545769675714));
#18027=CARTESIAN_POINT('Ctrl Pts',(-9.51647500000043,-0.265706620582359,
26.0670579008196));
#18028=CARTESIAN_POINT('Ctrl Pts',(-9.40727465387279,-0.529786878175724,
26.0795388340678));
#18029=CARTESIAN_POINT('Ctrl Pts',(-9.21961691907866,-0.71789478017376,
26.092019767316));
#18030=CARTESIAN_POINT('Ctrl Pts',(-9.03195918428454,-0.906002682171795,
26.1045007005642));
#18031=CARTESIAN_POINT('Ctrl Pts',(-8.76814132834505,-1.01583545019876,
26.1169816338124));
#18032=CARTESIAN_POINT('Ctrl Pts',(-8.50243547044628,-1.01647208230659,
26.1294625670606));
#18033=CARTESIAN_POINT('Ctrl Pts',(-8.23672961254751,-1.01710871441443,
26.1419435003088));
#18034=CARTESIAN_POINT('Ctrl Pts',(-7.97238846933441,-0.908541417083381,
26.154424433557));
#18035=CARTESIAN_POINT('Ctrl Pts',(-7.78383148002423,-0.721334926799411,
26.1669053668052));
#18036=CARTESIAN_POINT('Ctrl Pts',(-7.59527449071404,-0.534128436515441,
26.1793863000534));
#18037=CARTESIAN_POINT('Ctrl Pts',(-7.48480993131733,-0.270574496756871,
26.1918672333016));
#18038=CARTESIAN_POINT('Ctrl Pts',(-7.48353667075686,-0.00487092690936466,
26.2043481665497));
#18039=CARTESIAN_POINT('Ctrl Pts',(-7.4822634101964,0.260832642938141,26.2168290997979));
#18040=CARTESIAN_POINT('Ctrl Pts',(-7.59019703546696,0.525433154239479,
26.2293100330461));
#18041=CARTESIAN_POINT('Ctrl Pts',(-7.77695120652444,0.714438148392527,
26.2417909662943));
#18042=CARTESIAN_POINT('Ctrl Pts',(-7.96370537758193,0.903443142545575,
26.2542718995425));
#18043=CARTESIAN_POINT('Ctrl Pts',(-8.22699388814728,1.01453885915633,26.2667528327907));
#18044=CARTESIAN_POINT('Ctrl Pts',(-8.4926936445906,1.01644874085988,26.2792337660389));
#18045=CARTESIAN_POINT('Ctrl Pts',(-8.75839340103393,1.01835862256343,26.2917146992871));
#18046=CARTESIAN_POINT('Ctrl Pts',(-9.02325176140303,0.911059288979473,
26.3041956325353));
#18047=CARTESIAN_POINT('Ctrl Pts',(-9.21270367535775,0.724758509268121,
26.3166765657835));
#18048=CARTESIAN_POINT('Ctrl Pts',(-9.40215558931247,0.538457729556769,
26.3291574990317));
#18049=CARTESIAN_POINT('Ctrl Pts',(-9.51388182535819,0.275436159673174,
26.3416384322799));
#18050=CARTESIAN_POINT('Ctrl Pts',(-9.51642831724056,0.00974174196505557,
26.354119365528));
#18051=CARTESIAN_POINT('Ctrl Pts',(-9.51645943884196,0.00649459406757949,
26.3542718995425));
#18052=CARTESIAN_POINT('Ctrl Pts',(-9.51647499999999,0.00324729703478578,
26.354424433557));
#18053=CARTESIAN_POINT('Ctrl Pts',(-9.516475,1.53531618099316E-12,26.3545769675715));
#18054=CARTESIAN_POINT('Origin',(-8.5,0.,1.24542303242842));
#18055=CARTESIAN_POINT('',(-9.516475,1.46453950263162E-12,25.6954230324284));
#18056=CARTESIAN_POINT('',(-9.516475,1.49148331621119E-12,25.7545769675715));
#18057=CARTESIAN_POINT('',(-9.516475,1.78524650477582E-12,1.24542303242842));
#18058=CARTESIAN_POINT('Ctrl Pts',(-9.516475,1.46453950263162E-12,25.6954230324284));
#18059=CARTESIAN_POINT('Ctrl Pts',(-9.51647500000038,-0.265706620582523,
25.7079039656766));
#18060=CARTESIAN_POINT('Ctrl Pts',(-9.4072746538727,-0.529786878175871,
25.7203848989248));
#18061=CARTESIAN_POINT('Ctrl Pts',(-9.21961691907855,-0.717894780173876,
25.732865832173));
#18062=CARTESIAN_POINT('Ctrl Pts',(-9.0319591842844,-0.906002682171881,
25.7453467654212));
#18063=CARTESIAN_POINT('Ctrl Pts',(-8.76814132834489,-1.0158354501988,25.7578276986694));
#18064=CARTESIAN_POINT('Ctrl Pts',(-8.50243547044612,-1.0164720823066,25.7703086319176));
#18065=CARTESIAN_POINT('Ctrl Pts',(-8.23672961254734,-1.01710871441439,
25.7827895651658));
#18066=CARTESIAN_POINT('Ctrl Pts',(-7.97238846933427,-0.908541417083296,
25.795270498414));
#18067=CARTESIAN_POINT('Ctrl Pts',(-7.78383148002411,-0.721334926799295,
25.8077514316622));
#18068=CARTESIAN_POINT('Ctrl Pts',(-7.59527449071396,-0.534128436515294,
25.8202323649103));
#18069=CARTESIAN_POINT('Ctrl Pts',(-7.48480993131728,-0.270574496756706,
25.8327132981585));
#18070=CARTESIAN_POINT('Ctrl Pts',(-7.48353667075686,-0.00487092690920024,
25.8451942314067));
#18071=CARTESIAN_POINT('Ctrl Pts',(-7.48226341019644,0.260832642938306,
25.8576751646549));
#18072=CARTESIAN_POINT('Ctrl Pts',(-7.59019703546704,0.525433154239626,
25.8701560979031));
#18073=CARTESIAN_POINT('Ctrl Pts',(-7.77695120652456,0.714438148392644,
25.8826370311513));
#18074=CARTESIAN_POINT('Ctrl Pts',(-7.96370537758208,0.903443142545662,
25.8951179643995));
#18075=CARTESIAN_POINT('Ctrl Pts',(-8.22699388814744,1.01453885915637,25.9075988976477));
#18076=CARTESIAN_POINT('Ctrl Pts',(-8.49269364459077,1.01644874085988,25.9200798308959));
#18077=CARTESIAN_POINT('Ctrl Pts',(-8.75839340103409,1.01835862256339,25.9325607641441));
#18078=CARTESIAN_POINT('Ctrl Pts',(-9.02325176140318,0.911059288979388,
25.9450416973923));
#18079=CARTESIAN_POINT('Ctrl Pts',(-9.21270367535787,0.724758509268006,
25.9575226306405));
#18080=CARTESIAN_POINT('Ctrl Pts',(-9.40215558931256,0.538457729556623,
25.9700035638886));
#18081=CARTESIAN_POINT('Ctrl Pts',(-9.51388182535823,0.27543615967301,25.9824844971368));
#18082=CARTESIAN_POINT('Ctrl Pts',(-9.51642831724057,0.00974174196489115,
25.994965430385));
#18083=CARTESIAN_POINT('Ctrl Pts',(-9.51645943884196,0.00649459406745359,
25.9951179643995));
#18084=CARTESIAN_POINT('Ctrl Pts',(-9.51647499999999,0.00324729703469832,
25.995270498414));
#18085=CARTESIAN_POINT('Ctrl Pts',(-9.516475,1.48645593502261E-12,25.9954230324284));
#18086=CARTESIAN_POINT('Ctrl Pts',(-9.516475,1.49148331621119E-12,25.7545769675715));
#18087=CARTESIAN_POINT('Ctrl Pts',(-9.51647500000039,-0.265706620582535,
25.7670579008196));
#18088=CARTESIAN_POINT('Ctrl Pts',(-9.40727465387268,-0.529786878175923,
25.7795388340678));
#18089=CARTESIAN_POINT('Ctrl Pts',(-9.21961691907848,-0.717894780173939,
25.792019767316));
#18090=CARTESIAN_POINT('Ctrl Pts',(-9.03195918428429,-0.906002682171955,
25.8045007005642));
#18091=CARTESIAN_POINT('Ctrl Pts',(-8.76814132834472,-1.01583545019886,
25.8169816338124));
#18092=CARTESIAN_POINT('Ctrl Pts',(-8.50243547044591,-1.0164720823066,25.8294625670606));
#18093=CARTESIAN_POINT('Ctrl Pts',(-8.2367296125471,-1.01710871441434,25.8419435003088));
#18094=CARTESIAN_POINT('Ctrl Pts',(-7.97238846933401,-0.908541417083157,
25.854424433557));
#18095=CARTESIAN_POINT('Ctrl Pts',(-7.78383148002388,-0.72133492679907,
25.8669053668052));
#18096=CARTESIAN_POINT('Ctrl Pts',(-7.59527449071376,-0.534128436514983,
25.8793863000534));
#18097=CARTESIAN_POINT('Ctrl Pts',(-7.48480993131717,-0.27057449675631,
25.8918672333016));
#18098=CARTESIAN_POINT('Ctrl Pts',(-7.48353667075686,-0.00487092690876495,
25.9043481665498));
#18099=CARTESIAN_POINT('Ctrl Pts',(-7.48226341019655,0.26083264293878,25.916829099798));
#18100=CARTESIAN_POINT('Ctrl Pts',(-7.5901970354673,0.525433154240091,25.9293100330462));
#18101=CARTESIAN_POINT('Ctrl Pts',(-7.77695120652495,0.714438148393036,
25.9417909662944));
#18102=CARTESIAN_POINT('Ctrl Pts',(-7.96370537758259,0.90344314254598,25.9542718995425));
#18103=CARTESIAN_POINT('Ctrl Pts',(-8.22699388814807,1.01453885915655,25.9667528327907));
#18104=CARTESIAN_POINT('Ctrl Pts',(-8.49269364459143,1.01644874085988,25.9792337660389));
#18105=CARTESIAN_POINT('Ctrl Pts',(-8.7583934010348,1.01835862256322,25.9917146992871));
#18106=CARTESIAN_POINT('Ctrl Pts',(-9.02325176140386,0.911059288979013,
26.0041956325353));
#18107=CARTESIAN_POINT('Ctrl Pts',(-9.21270367535843,0.724758509267457,
26.0166765657835));
#18108=CARTESIAN_POINT('Ctrl Pts',(-9.402155589313,0.538457729555902,26.0291574990317));
#18109=CARTESIAN_POINT('Ctrl Pts',(-9.51388182535848,0.275436159672154,
26.0416384322799));
#18110=CARTESIAN_POINT('Ctrl Pts',(-9.51642831724057,0.00974174196399366,
26.0541193655281));
#18111=CARTESIAN_POINT('Ctrl Pts',(-9.51645943884197,0.00649459406690274,
26.0542718995425));
#18112=CARTESIAN_POINT('Ctrl Pts',(-9.51647499999999,0.00324729703449424,
26.054424433557));
#18113=CARTESIAN_POINT('Ctrl Pts',(-9.516475,1.62895957697526E-12,26.0545769675714));
#18114=CARTESIAN_POINT('Origin',(-8.5,0.,1.24542303242842));
#18115=CARTESIAN_POINT('',(-9.51609769462188,7.92988697302073E-5,25.3954230324284));
#18116=CARTESIAN_POINT('',(-9.516475,1.46956688382021E-12,25.4545769675715));
#18117=CARTESIAN_POINT('',(-9.516475,1.78524650477582E-12,1.24542303242842));
#18118=CARTESIAN_POINT('Ctrl Pts',(-9.516475,1.50040298442718E-12,25.3954230324284));
#18119=CARTESIAN_POINT('Ctrl Pts',(-9.51647500000039,-0.265706620582449,
25.4079039656766));
#18120=CARTESIAN_POINT('Ctrl Pts',(-9.40727465387275,-0.529786878175763,
25.4203848989248));
#18121=CARTESIAN_POINT('Ctrl Pts',(-9.21961691907866,-0.717894780173769,
25.432865832173));
#18122=CARTESIAN_POINT('Ctrl Pts',(-9.03195918428456,-0.906002682171775,
25.4453467654212));
#18123=CARTESIAN_POINT('Ctrl Pts',(-8.76814132834512,-1.01583545019873,
25.4578276986694));
#18124=CARTESIAN_POINT('Ctrl Pts',(-8.50243547044638,-1.01647208230659,
25.4703086319176));
#18125=CARTESIAN_POINT('Ctrl Pts',(-8.23672961254765,-1.01710871441446,
25.4827895651658));
#18126=CARTESIAN_POINT('Ctrl Pts',(-7.97238846933458,-0.908541417083467,
25.4952704984139));
#18127=CARTESIAN_POINT('Ctrl Pts',(-7.78383148002438,-0.721334926799565,
25.5077514316621));
#18128=CARTESIAN_POINT('Ctrl Pts',(-7.59527449071418,-0.534128436515662,
25.5202323649103));
#18129=CARTESIAN_POINT('Ctrl Pts',(-7.48480993131742,-0.270574496757165,
25.5327132981585));
#18130=CARTESIAN_POINT('Ctrl Pts',(-7.48353667075686,-0.00487092690969834,
25.5451942314067));
#18131=CARTESIAN_POINT('Ctrl Pts',(-7.48226341019631,0.260832642937769,
25.5576751646549));
#18132=CARTESIAN_POINT('Ctrl Pts',(-7.59019703546675,0.525433154239104,
25.5701560979031));
#18133=CARTESIAN_POINT('Ctrl Pts',(-7.77695120652413,0.714438148392207,
25.5826370311513));
#18134=CARTESIAN_POINT('Ctrl Pts',(-7.96370537758151,0.903443142545311,
25.5951179643995));
#18135=CARTESIAN_POINT('Ctrl Pts',(-8.22699388814675,1.01453885915618,25.6075988976477));
#18136=CARTESIAN_POINT('Ctrl Pts',(-8.49269364459004,1.01644874085987,25.6200798308958));
#18137=CARTESIAN_POINT('Ctrl Pts',(-8.75839340103332,1.01835862256357,25.632560764144));
#18138=CARTESIAN_POINT('Ctrl Pts',(-9.02325176140245,0.911059288979796,
25.6450416973922));
#18139=CARTESIAN_POINT('Ctrl Pts',(-9.21270367535727,0.724758509268598,
25.6575226306404));
#18140=CARTESIAN_POINT('Ctrl Pts',(-9.40215558931207,0.538457729557414,
25.6700035638886));
#18141=CARTESIAN_POINT('Ctrl Pts',(-9.51388182535796,0.275436159673968,
25.6824844971368));
#18142=CARTESIAN_POINT('Ctrl Pts',(-9.51642831724056,0.00974174196590923,
25.694965430385));
#18143=CARTESIAN_POINT('Ctrl Pts',(-9.51645943884196,0.00649459406812504,
25.6951179643995));
#18144=CARTESIAN_POINT('Ctrl Pts',(-9.51647499999999,0.00324729703502315,
25.6952704984139));
#18145=CARTESIAN_POINT('Ctrl Pts',(-9.516475,1.46453950263162E-12,25.6954230324284));
#18146=CARTESIAN_POINT('Ctrl Pts',(-9.516475,1.46956688382021E-12,25.4545769675715));
#18147=CARTESIAN_POINT('Ctrl Pts',(-9.51647500000038,-0.265706620582518,
25.4670579008196));
#18148=CARTESIAN_POINT('Ctrl Pts',(-9.4072746538727,-0.529786878175867,
25.4795388340678));
#18149=CARTESIAN_POINT('Ctrl Pts',(-9.21961691907855,-0.717894780173873,
25.492019767316));
#18150=CARTESIAN_POINT('Ctrl Pts',(-9.0319591842844,-0.906002682171879,
25.5045007005642));
#18151=CARTESIAN_POINT('Ctrl Pts',(-8.76814132834489,-1.0158354501988,25.5169816338124));
#18152=CARTESIAN_POINT('Ctrl Pts',(-8.50243547044612,-1.0164720823066,25.5294625670606));
#18153=CARTESIAN_POINT('Ctrl Pts',(-8.23672961254735,-1.01710871441439,
25.5419435003088));
#18154=CARTESIAN_POINT('Ctrl Pts',(-7.97238846933427,-0.908541417083299,
25.554424433557));
#18155=CARTESIAN_POINT('Ctrl Pts',(-7.78383148002411,-0.721334926799299,
25.5669053668052));
#18156=CARTESIAN_POINT('Ctrl Pts',(-7.59527449071396,-0.534128436515299,
25.5793863000534));
#18157=CARTESIAN_POINT('Ctrl Pts',(-7.48480993131728,-0.270574496756711,
25.5918672333016));
#18158=CARTESIAN_POINT('Ctrl Pts',(-7.48353667075686,-0.00487092690920527,
25.6043481665498));
#18159=CARTESIAN_POINT('Ctrl Pts',(-7.48226341019644,0.260832642938301,
25.6168290997979));
#18160=CARTESIAN_POINT('Ctrl Pts',(-7.59019703546704,0.525433154239621,
25.6293100330461));
#18161=CARTESIAN_POINT('Ctrl Pts',(-7.77695120652456,0.71443814839264,25.6417909662943));
#18162=CARTESIAN_POINT('Ctrl Pts',(-7.96370537758207,0.903443142545659,
25.6542718995425));
#18163=CARTESIAN_POINT('Ctrl Pts',(-8.22699388814744,1.01453885915637,25.6667528327907));
#18164=CARTESIAN_POINT('Ctrl Pts',(-8.49269364459076,1.01644874085988,25.6792337660389));
#18165=CARTESIAN_POINT('Ctrl Pts',(-8.75839340103408,1.01835862256339,25.6917146992871));
#18166=CARTESIAN_POINT('Ctrl Pts',(-9.02325176140318,0.911059288979391,
25.7041956325353));
#18167=CARTESIAN_POINT('Ctrl Pts',(-9.21270367535787,0.724758509268009,
25.7166765657835));
#18168=CARTESIAN_POINT('Ctrl Pts',(-9.40215558931255,0.538457729556628,
25.7291574990317));
#18169=CARTESIAN_POINT('Ctrl Pts',(-9.51388182535823,0.275436159673015,
25.7416384322799));
#18170=CARTESIAN_POINT('Ctrl Pts',(-9.51642831724057,0.00974174196489618,
25.754119365528));
#18171=CARTESIAN_POINT('Ctrl Pts',(-9.51645943884196,0.00649459406745862,
25.7542718995425));
#18172=CARTESIAN_POINT('Ctrl Pts',(-9.51647499999999,0.00324729703470335,
25.754424433557));
#18173=CARTESIAN_POINT('Ctrl Pts',(-9.516475,1.49148331621119E-12,25.7545769675715));
#18174=CARTESIAN_POINT('Origin',(-8.5,0.,1.24542303242842));
#18175=CARTESIAN_POINT('',(-9.51649580167683,2.1540054757358E-5,25.0954230324284));
#18176=CARTESIAN_POINT('',(-9.516475,1.44765045142922E-12,25.1545769675715));
#18177=CARTESIAN_POINT('',(-9.516475,1.78524650477582E-12,1.24542303242842));
#18178=CARTESIAN_POINT('Ctrl Pts',(-9.51721349225105,0.000764705779924109,
25.0954230324284));
#18179=CARTESIAN_POINT('Ctrl Pts',(-9.51484927656888,-0.286952017602154,
25.1089718447615));
#18180=CARTESIAN_POINT('Ctrl Pts',(-9.23722805908837,-0.916544261020621,
25.1384279982462));
#18181=CARTESIAN_POINT('Ctrl Pts',(-8.16676365035883,-1.15554187977053,
25.1837914928825));
#18182=CARTESIAN_POINT('Ctrl Pts',(-7.48649317569277,-0.480077979335733,
25.2235598457615));
#18183=CARTESIAN_POINT('Ctrl Pts',(-7.4661733610654,0.218649185746783,25.2553745280648));
#18184=CARTESIAN_POINT('Ctrl Pts',(-7.76765364280032,0.849317232991748,
25.287189210368));
#18185=CARTESIAN_POINT('Ctrl Pts',(-8.6631541573295,1.19151341644644,25.3269575632471));
#18186=CARTESIAN_POINT('Ctrl Pts',(-9.41619328487241,0.634917146514559,
25.3656867274592));
#18187=CARTESIAN_POINT('Ctrl Pts',(-9.51549925971945,0.148008510868454,
25.3885085505196));
#18188=CARTESIAN_POINT('Ctrl Pts',(-9.51497361421595,0.000315548626982715,
25.3954230324284));
#18189=CARTESIAN_POINT('Ctrl Pts',(-9.516475,1.50543036561576E-12,25.1545769675715));
#18190=CARTESIAN_POINT('Ctrl Pts',(-9.51647500000039,-0.265706620582463,
25.1670579008196));
#18191=CARTESIAN_POINT('Ctrl Pts',(-9.40727465387274,-0.529786878175797,
25.1795388340678));
#18192=CARTESIAN_POINT('Ctrl Pts',(-9.21961691907862,-0.717894780173806,
25.192019767316));
#18193=CARTESIAN_POINT('Ctrl Pts',(-9.0319591842845,-0.906002682171816,
25.2045007005642));
#18194=CARTESIAN_POINT('Ctrl Pts',(-8.76814132834503,-1.01583545019876,
25.2169816338124));
#18195=CARTESIAN_POINT('Ctrl Pts',(-8.50243547044627,-1.01647208230659,
25.2294625670606));
#18196=CARTESIAN_POINT('Ctrl Pts',(-8.23672961254752,-1.01710871441443,
25.2419435003088));
#18197=CARTESIAN_POINT('Ctrl Pts',(-7.97238846933444,-0.908541417083394,
25.254424433557));
#18198=CARTESIAN_POINT('Ctrl Pts',(-7.78383148002426,-0.721334926799446,
25.2669053668052));
#18199=CARTESIAN_POINT('Ctrl Pts',(-7.59527449071408,-0.534128436515499,
25.2793863000534));
#18200=CARTESIAN_POINT('Ctrl Pts',(-7.48480993131736,-0.270574496756959,
25.2918672333015));
#18201=CARTESIAN_POINT('Ctrl Pts',(-7.48353667075686,-0.00487092690947225,
25.3043481665497));
#18202=CARTESIAN_POINT('Ctrl Pts',(-7.48226341019637,0.260832642938014,
25.3168290997979));
#18203=CARTESIAN_POINT('Ctrl Pts',(-7.59019703546688,0.525433154239344,
25.3293100330461));
#18204=CARTESIAN_POINT('Ctrl Pts',(-7.77695120652433,0.714438148392409,
25.3417909662943));
#18205=CARTESIAN_POINT('Ctrl Pts',(-7.96370537758177,0.903443142545474,
25.3542718995425));
#18206=CARTESIAN_POINT('Ctrl Pts',(-8.22699388814707,1.01453885915627,25.3667528327907));
#18207=CARTESIAN_POINT('Ctrl Pts',(-8.49269364459038,1.01644874085988,25.3792337660389));
#18208=CARTESIAN_POINT('Ctrl Pts',(-8.75839340103368,1.01835862256349,25.3917146992871));
#18209=CARTESIAN_POINT('Ctrl Pts',(-9.0232517614028,0.911059288979604,25.4041956325353));
#18210=CARTESIAN_POINT('Ctrl Pts',(-9.21270367535755,0.724758509268318,
25.4166765657835));
#18211=CARTESIAN_POINT('Ctrl Pts',(-9.40215558931231,0.538457729557032,
25.4291574990316));
#18212=CARTESIAN_POINT('Ctrl Pts',(-9.5138818253581,0.275436159673493,25.4416384322798));
#18213=CARTESIAN_POINT('Ctrl Pts',(-9.51642831724056,0.00974174196539426,
25.454119365528));
#18214=CARTESIAN_POINT('Ctrl Pts',(-9.51645943884196,0.00649459406778338,
25.4542718995425));
#18215=CARTESIAN_POINT('Ctrl Pts',(-9.51647499999999,0.00324729703485473,
25.454424433557));
#18216=CARTESIAN_POINT('Ctrl Pts',(-9.516475,1.46956688382021E-12,25.4545769675715));
#18217=CARTESIAN_POINT('Origin',(-8.5,0.,1.24542303242842));
#18218=CARTESIAN_POINT('',(-9.516475,1.39879020545867E-12,24.7954230324284));
#18219=CARTESIAN_POINT('',(-9.516475,1.42573401903824E-12,24.8545769675715));
#18220=CARTESIAN_POINT('',(-9.516475,1.78524650477582E-12,1.24542303242842));
#18221=CARTESIAN_POINT('Ctrl Pts',(-9.516475,1.45657011964521E-12,24.7954230324284));
#18222=CARTESIAN_POINT('Ctrl Pts',(-9.51647500000038,-0.265706620582531,
24.8079039656766));
#18223=CARTESIAN_POINT('Ctrl Pts',(-9.4072746538727,-0.529786878175878,
24.8203848989248));
#18224=CARTESIAN_POINT('Ctrl Pts',(-9.21961691907854,-0.717894780173882,
24.832865832173));
#18225=CARTESIAN_POINT('Ctrl Pts',(-9.03195918428439,-0.906002682171885,
24.8453467654212));
#18226=CARTESIAN_POINT('Ctrl Pts',(-8.76814132834488,-1.0158354501988,24.8578276986694));
#18227=CARTESIAN_POINT('Ctrl Pts',(-8.50243547044611,-1.0164720823066,24.8703086319176));
#18228=CARTESIAN_POINT('Ctrl Pts',(-8.23672961254733,-1.01710871441439,
24.8827895651658));
#18229=CARTESIAN_POINT('Ctrl Pts',(-7.97238846933426,-0.908541417083292,
24.895270498414));
#18230=CARTESIAN_POINT('Ctrl Pts',(-7.78383148002411,-0.72133492679929,
24.9077514316622));
#18231=CARTESIAN_POINT('Ctrl Pts',(-7.59527449071395,-0.534128436515287,
24.9202323649103));
#18232=CARTESIAN_POINT('Ctrl Pts',(-7.48480993131728,-0.270574496756698,
24.9327132981585));
#18233=CARTESIAN_POINT('Ctrl Pts',(-7.48353667075686,-0.00487092690919227,
24.9451942314067));
#18234=CARTESIAN_POINT('Ctrl Pts',(-7.48226341019644,0.260832642938314,
24.9576751646549));
#18235=CARTESIAN_POINT('Ctrl Pts',(-7.59019703546705,0.525433154239633,
24.9701560979031));
#18236=CARTESIAN_POINT('Ctrl Pts',(-7.77695120652456,0.71443814839265,24.9826370311513));
#18237=CARTESIAN_POINT('Ctrl Pts',(-7.96370537758208,0.903443142545666,
24.9951179643995));
#18238=CARTESIAN_POINT('Ctrl Pts',(-8.22699388814745,1.01453885915637,25.0075988976477));
#18239=CARTESIAN_POINT('Ctrl Pts',(-8.49269364459077,1.01644874085988,25.0200798308959));
#18240=CARTESIAN_POINT('Ctrl Pts',(-8.7583934010341,1.01835862256338,25.0325607641441));
#18241=CARTESIAN_POINT('Ctrl Pts',(-9.02325176140319,0.911059288979384,
25.0450416973923));
#18242=CARTESIAN_POINT('Ctrl Pts',(-9.21270367535788,0.724758509268,25.0575226306405));
#18243=CARTESIAN_POINT('Ctrl Pts',(-9.40215558931256,0.538457729556616,
25.0700035638886));
#18244=CARTESIAN_POINT('Ctrl Pts',(-9.51388182535824,0.275436159673003,
25.0824844971368));
#18245=CARTESIAN_POINT('Ctrl Pts',(-9.51642831724057,0.00974174196488318,
25.094965430385));
#18246=CARTESIAN_POINT('Ctrl Pts',(-9.51645943884196,0.00649459406742636,
25.0951179643995));
#18247=CARTESIAN_POINT('Ctrl Pts',(-9.51647499999999,0.00324729703465179,
25.095270498414));
#18248=CARTESIAN_POINT('Ctrl Pts',(-9.516475,1.42070663784965E-12,25.0954230324284));
#18249=CARTESIAN_POINT('Ctrl Pts',(-9.516475,1.48351393322478E-12,24.8545769675715));
#18250=CARTESIAN_POINT('Ctrl Pts',(-9.51647500000039,-0.265706620582466,
24.8670579008196));
#18251=CARTESIAN_POINT('Ctrl Pts',(-9.40727465387274,-0.529786878175778,
24.8795388340678));
#18252=CARTESIAN_POINT('Ctrl Pts',(-9.21961691907864,-0.717894780173781,
24.892019767316));
#18253=CARTESIAN_POINT('Ctrl Pts',(-9.03195918428454,-0.906002682171783,
24.9045007005642));
#18254=CARTESIAN_POINT('Ctrl Pts',(-8.7681413283451,-1.01583545019874,24.9169816338124));
#18255=CARTESIAN_POINT('Ctrl Pts',(-8.50243547044636,-1.01647208230659,
24.9294625670606));
#18256=CARTESIAN_POINT('Ctrl Pts',(-8.23672961254763,-1.01710871441445,
24.9419435003088));
#18257=CARTESIAN_POINT('Ctrl Pts',(-7.97238846933456,-0.908541417083459,
24.954424433557));
#18258=CARTESIAN_POINT('Ctrl Pts',(-7.78383148002437,-0.721334926799553,
24.9669053668052));
#18259=CARTESIAN_POINT('Ctrl Pts',(-7.59527449071418,-0.534128436515647,
24.9793863000533));
#18260=CARTESIAN_POINT('Ctrl Pts',(-7.48480993131741,-0.270574496757148,
24.9918672333015));
#18261=CARTESIAN_POINT('Ctrl Pts',(-7.48353667075686,-0.00487092690968145,
25.0043481665497));
#18262=CARTESIAN_POINT('Ctrl Pts',(-7.48226341019632,0.260832642937786,
25.0168290997979));
#18263=CARTESIAN_POINT('Ctrl Pts',(-7.59019703546676,0.525433154239119,
25.0293100330461));
#18264=CARTESIAN_POINT('Ctrl Pts',(-7.77695120652414,0.714438148392219,
25.0417909662943));
#18265=CARTESIAN_POINT('Ctrl Pts',(-7.96370537758152,0.90344314254532,25.0542718995425));
#18266=CARTESIAN_POINT('Ctrl Pts',(-8.22699388814677,1.01453885915618,25.0667528327907));
#18267=CARTESIAN_POINT('Ctrl Pts',(-8.49269364459005,1.01644874085987,25.0792337660389));
#18268=CARTESIAN_POINT('Ctrl Pts',(-8.75839340103334,1.01835862256357,25.0917146992871));
#18269=CARTESIAN_POINT('Ctrl Pts',(-9.02325176140247,0.911059288979787,
25.1041956325352));
#18270=CARTESIAN_POINT('Ctrl Pts',(-9.21270367535728,0.724758509268586,
25.1166765657834));
#18271=CARTESIAN_POINT('Ctrl Pts',(-9.40215558931209,0.538457729557385,
25.1291574990316));
#18272=CARTESIAN_POINT('Ctrl Pts',(-9.51388182535798,0.275436159673913,
25.1416384322798));
#18273=CARTESIAN_POINT('Ctrl Pts',(-9.51642831724056,0.00974174196583456,
25.154119365528));
#18274=CARTESIAN_POINT('Ctrl Pts',(-9.51645943884196,0.00649459406808889,
25.1542718995425));
#18275=CARTESIAN_POINT('Ctrl Pts',(-9.51647499999999,0.00324729703502544,
25.154424433557));
#18276=CARTESIAN_POINT('Ctrl Pts',(-9.516475,1.50543036561576E-12,25.1545769675715));
#18277=CARTESIAN_POINT('Origin',(-8.5,0.,1.24542303242842));
#18278=CARTESIAN_POINT('',(-9.516475,1.37687377306768E-12,24.4954230324284));
#18279=CARTESIAN_POINT('',(-9.516475,1.40381758664725E-12,24.5545769675715));
#18280=CARTESIAN_POINT('',(-9.516475,1.78524650477582E-12,1.24542303242842));
#18281=CARTESIAN_POINT('Ctrl Pts',(-9.516475,1.31909385888114E-12,24.4954230324284));
#18282=CARTESIAN_POINT('Ctrl Pts',(-9.51647500000034,-0.26570662058263,
24.5079039656766));
#18283=CARTESIAN_POINT('Ctrl Pts',(-9.40727465387266,-0.529786878175925,
24.5203848989248));
#18284=CARTESIAN_POINT('Ctrl Pts',(-9.21961691907853,-0.717894780173897,
24.532865832173));
#18285=CARTESIAN_POINT('Ctrl Pts',(-9.0319591842844,-0.90600268217187,24.5453467654212));
#18286=CARTESIAN_POINT('Ctrl Pts',(-8.76814132834494,-1.01583545019878,
24.5578276986694));
#18287=CARTESIAN_POINT('Ctrl Pts',(-8.5024354704462,-1.0164720823066,24.5703086319176));
#18288=CARTESIAN_POINT('Ctrl Pts',(-8.23672961254747,-1.01710871441441,
24.5827895651658));
#18289=CARTESIAN_POINT('Ctrl Pts',(-7.97238846933442,-0.908541417083373,
24.595270498414));
#18290=CARTESIAN_POINT('Ctrl Pts',(-7.78383148002425,-0.721334926799437,
24.6077514316621));
#18291=CARTESIAN_POINT('Ctrl Pts',(-7.59527449071409,-0.534128436515501,
24.6202323649103));
#18292=CARTESIAN_POINT('Ctrl Pts',(-7.48480993131737,-0.270574496756984,
24.6327132981585));
#18293=CARTESIAN_POINT('Ctrl Pts',(-7.48353667075686,-0.00487092690951703,
24.6451942314067));
#18294=CARTESIAN_POINT('Ctrl Pts',(-7.48226341019636,0.26083264293795,24.6576751646549));
#18295=CARTESIAN_POINT('Ctrl Pts',(-7.59019703546684,0.525433154239266,
24.6701560979031));
#18296=CARTESIAN_POINT('Ctrl Pts',(-7.77695120652426,0.714438148392336,
24.6826370311513));
#18297=CARTESIAN_POINT('Ctrl Pts',(-7.96370537758167,0.903443142545406,
24.6951179643995));
#18298=CARTESIAN_POINT('Ctrl Pts',(-8.22699388814693,1.01453885915622,24.7075988976477));
#18299=CARTESIAN_POINT('Ctrl Pts',(-8.49269364459022,1.01644874085988,24.7200798308959));
#18300=CARTESIAN_POINT('Ctrl Pts',(-8.7583934010335,1.01835862256353,24.732560764144));
#18301=CARTESIAN_POINT('Ctrl Pts',(-9.02325176140262,0.911059288979703,
24.7450416973922));
#18302=CARTESIAN_POINT('Ctrl Pts',(-9.2127036753574,0.724758509268471,24.7575226306404));
#18303=CARTESIAN_POINT('Ctrl Pts',(-9.40215558931218,0.538457729557239,
24.7700035638886));
#18304=CARTESIAN_POINT('Ctrl Pts',(-9.51388182535803,0.275436159673749,
24.7824844971368));
#18305=CARTESIAN_POINT('Ctrl Pts',(-9.51642831724056,0.00974174196567015,
24.794965430385));
#18306=CARTESIAN_POINT('Ctrl Pts',(-9.51645943884196,0.00649459406796299,
24.7951179643995));
#18307=CARTESIAN_POINT('Ctrl Pts',(-9.51647499999999,0.00324729703493815,
24.7952704984139));
#18308=CARTESIAN_POINT('Ctrl Pts',(-9.516475,1.45657011964521E-12,24.7954230324284));
#18309=CARTESIAN_POINT('Ctrl Pts',(-9.516475,1.40381758664725E-12,24.5545769675715));
#18310=CARTESIAN_POINT('Ctrl Pts',(-9.51647500000037,-0.265706620582546,
24.5670579008196));
#18311=CARTESIAN_POINT('Ctrl Pts',(-9.4072746538727,-0.529786878175849,
24.5795388340678));
#18312=CARTESIAN_POINT('Ctrl Pts',(-9.21961691907859,-0.717894780173837,
24.592019767316));
#18313=CARTESIAN_POINT('Ctrl Pts',(-9.03195918428447,-0.906002682171825,
24.6045007005642));
#18314=CARTESIAN_POINT('Ctrl Pts',(-8.76814132834502,-1.01583545019876,
24.6169816338124));
#18315=CARTESIAN_POINT('Ctrl Pts',(-8.50243547044629,-1.01647208230659,
24.6294625670606));
#18316=CARTESIAN_POINT('Ctrl Pts',(-8.23672961254755,-1.01710871441443,
24.6419435003088));
#18317=CARTESIAN_POINT('Ctrl Pts',(-7.97238846933449,-0.908541417083417,
24.654424433557));
#18318=CARTESIAN_POINT('Ctrl Pts',(-7.78383148002431,-0.721334926799497,
24.6669053668052));
#18319=CARTESIAN_POINT('Ctrl Pts',(-7.59527449071413,-0.534128436515576,
24.6793863000534));
#18320=CARTESIAN_POINT('Ctrl Pts',(-7.48480993131739,-0.270574496757069,
24.6918672333015));
#18321=CARTESIAN_POINT('Ctrl Pts',(-7.48353667075686,-0.00487092690960175,
24.7043481665497));
#18322=CARTESIAN_POINT('Ctrl Pts',(-7.48226341019634,0.260832642937865,
24.7168290997979));
#18323=CARTESIAN_POINT('Ctrl Pts',(-7.5901970354668,0.52543315423919,24.7293100330461));
#18324=CARTESIAN_POINT('Ctrl Pts',(-7.7769512065242,0.714438148392276,24.7417909662943));
#18325=CARTESIAN_POINT('Ctrl Pts',(-7.96370537758159,0.903443142545362,
24.7542718995425));
#18326=CARTESIAN_POINT('Ctrl Pts',(-8.22699388814685,1.0145388591562,24.7667528327907));
#18327=CARTESIAN_POINT('Ctrl Pts',(-8.49269364459013,1.01644874085987,24.7792337660389));
#18328=CARTESIAN_POINT('Ctrl Pts',(-8.75839340103342,1.01835862256355,24.7917146992871));
#18329=CARTESIAN_POINT('Ctrl Pts',(-9.02325176140254,0.911059288979746,
24.8041956325353));
#18330=CARTESIAN_POINT('Ctrl Pts',(-9.21270367535734,0.72475850926853,24.8166765657834));
#18331=CARTESIAN_POINT('Ctrl Pts',(-9.40215558931213,0.538457729557314,
24.8291574990316));
#18332=CARTESIAN_POINT('Ctrl Pts',(-9.513881825358,0.275436159673833,24.8416384322798));
#18333=CARTESIAN_POINT('Ctrl Pts',(-9.51642831724056,0.00974174196575487,
24.854119365528));
#18334=CARTESIAN_POINT('Ctrl Pts',(-9.51645943884196,0.00649459406802845,
24.8542718995425));
#18335=CARTESIAN_POINT('Ctrl Pts',(-9.51647499999999,0.00324729703498431,
24.854424433557));
#18336=CARTESIAN_POINT('Ctrl Pts',(-9.516475,1.48351393322478E-12,24.8545769675715));
#18337=CARTESIAN_POINT('Origin',(-8.5,0.,1.24542303242842));
#18338=CARTESIAN_POINT('',(-9.516475,1.3549573406767E-12,24.1954230324284));
#18339=CARTESIAN_POINT('',(-9.516475,1.38190115425627E-12,24.2545769675715));
#18340=CARTESIAN_POINT('',(-9.516475,1.78524650477582E-12,1.24542303242842));
#18341=CARTESIAN_POINT('Ctrl Pts',(-9.516475,1.3549573406767E-12,24.1954230324284));
#18342=CARTESIAN_POINT('Ctrl Pts',(-9.51647500000035,-0.265706620582594,
24.2079039656766));
#18343=CARTESIAN_POINT('Ctrl Pts',(-9.40727465387268,-0.529786878175893,
24.2203848989248));
#18344=CARTESIAN_POINT('Ctrl Pts',(-9.21961691907855,-0.717894780173872,
24.232865832173));
#18345=CARTESIAN_POINT('Ctrl Pts',(-9.03195918428443,-0.906002682171851,
24.2453467654212));
#18346=CARTESIAN_POINT('Ctrl Pts',(-8.76814132834497,-1.01583545019877,
24.2578276986694));
#18347=CARTESIAN_POINT('Ctrl Pts',(-8.50243547044624,-1.0164720823066,24.2703086319176));
#18348=CARTESIAN_POINT('Ctrl Pts',(-8.2367296125475,-1.01710871441442,24.2827895651658));
#18349=CARTESIAN_POINT('Ctrl Pts',(-7.97238846933445,-0.908541417083392,
24.295270498414));
#18350=CARTESIAN_POINT('Ctrl Pts',(-7.78383148002428,-0.721334926799462,
24.3077514316621));
#18351=CARTESIAN_POINT('Ctrl Pts',(-7.59527449071411,-0.534128436515533,
24.3202323649103));
#18352=CARTESIAN_POINT('Ctrl Pts',(-7.48480993131738,-0.27057449675702,
24.3327132981585));
#18353=CARTESIAN_POINT('Ctrl Pts',(-7.48353667075686,-0.00487092690955289,
24.3451942314067));
#18354=CARTESIAN_POINT('Ctrl Pts',(-7.48226341019635,0.260832642937914,
24.3576751646549));
#18355=CARTESIAN_POINT('Ctrl Pts',(-7.59019703546683,0.525433154239234,
24.3701560979031));
#18356=CARTESIAN_POINT('Ctrl Pts',(-7.77695120652423,0.714438148392311,
24.3826370311513));
#18357=CARTESIAN_POINT('Ctrl Pts',(-7.96370537758163,0.903443142545388,
24.3951179643995));
#18358=CARTESIAN_POINT('Ctrl Pts',(-8.2269938881469,1.01453885915621,24.4075988976477));
#18359=CARTESIAN_POINT('Ctrl Pts',(-8.49269364459018,1.01644874085987,24.4200798308958));
#18360=CARTESIAN_POINT('Ctrl Pts',(-8.75839340103347,1.01835862256353,24.432560764144));
#18361=CARTESIAN_POINT('Ctrl Pts',(-9.02325176140259,0.911059288979721,
24.4450416973922));
#18362=CARTESIAN_POINT('Ctrl Pts',(-9.21270367535737,0.724758509268496,
24.4575226306404));
#18363=CARTESIAN_POINT('Ctrl Pts',(-9.40215558931216,0.538457729557271,
24.4700035638886));
#18364=CARTESIAN_POINT('Ctrl Pts',(-9.51388182535801,0.275436159673785,
24.4824844971368));
#18365=CARTESIAN_POINT('Ctrl Pts',(-9.51642831724056,0.00974174196570601,
24.494965430385));
#18366=CARTESIAN_POINT('Ctrl Pts',(-9.51645943884196,0.00649459406794107,
24.4951179643995));
#18367=CARTESIAN_POINT('Ctrl Pts',(-9.516475,0.00324729703485833,24.495270498414));
#18368=CARTESIAN_POINT('Ctrl Pts',(-9.516475,1.31909385888114E-12,24.4954230324284));
#18369=CARTESIAN_POINT('Ctrl Pts',(-9.516475,1.43968106844281E-12,24.2545769675715));
#18370=CARTESIAN_POINT('Ctrl Pts',(-9.51647500000038,-0.265706620582529,
24.2670579008196));
#18371=CARTESIAN_POINT('Ctrl Pts',(-9.4072746538727,-0.529786878175855,
24.2795388340678));
#18372=CARTESIAN_POINT('Ctrl Pts',(-9.21961691907857,-0.717894780173853,
24.292019767316));
#18373=CARTESIAN_POINT('Ctrl Pts',(-9.03195918428444,-0.90600268217185,
24.3045007005642));
#18374=CARTESIAN_POINT('Ctrl Pts',(-8.76814132834496,-1.01583545019878,
24.3169816338124));
#18375=CARTESIAN_POINT('Ctrl Pts',(-8.50243547044621,-1.0164720823066,24.3294625670606));
#18376=CARTESIAN_POINT('Ctrl Pts',(-8.23672961254745,-1.01710871441441,
24.3419435003088));
#18377=CARTESIAN_POINT('Ctrl Pts',(-7.97238846933439,-0.908541417083359,
24.354424433557));
#18378=CARTESIAN_POINT('Ctrl Pts',(-7.78383148002422,-0.7213349267994,24.3669053668052));
#18379=CARTESIAN_POINT('Ctrl Pts',(-7.59527449071405,-0.53412843651544,
24.3793863000534));
#18380=CARTESIAN_POINT('Ctrl Pts',(-7.48480993131734,-0.270574496756893,
24.3918672333016));
#18381=CARTESIAN_POINT('Ctrl Pts',(-7.48353667075686,-0.0048709269094065,
24.4043481665497));
#18382=CARTESIAN_POINT('Ctrl Pts',(-7.48226341019639,0.26083264293808,24.4168290997979));
#18383=CARTESIAN_POINT('Ctrl Pts',(-7.59019703546692,0.525433154239403,
24.4293100330461));
#18384=CARTESIAN_POINT('Ctrl Pts',(-7.77695120652437,0.714438148392456,
24.4417909662943));
#18385=CARTESIAN_POINT('Ctrl Pts',(-7.96370537758183,0.903443142545509,
24.4542718995425));
#18386=CARTESIAN_POINT('Ctrl Pts',(-8.22699388814714,1.01453885915628,24.4667528327907));
#18387=CARTESIAN_POINT('Ctrl Pts',(-8.49269364459044,1.01644874085988,24.4792337660389));
#18388=CARTESIAN_POINT('Ctrl Pts',(-8.75839340103375,1.01835862256347,24.4917146992871));
#18389=CARTESIAN_POINT('Ctrl Pts',(-9.02325176140286,0.91105928897957,24.5041956325353));
#18390=CARTESIAN_POINT('Ctrl Pts',(-9.2127036753576,0.724758509268272,24.5166765657835));
#18391=CARTESIAN_POINT('Ctrl Pts',(-9.40215558931234,0.538457729556974,
24.5291574990316));
#18392=CARTESIAN_POINT('Ctrl Pts',(-9.51388182535812,0.275436159673427,
24.5416384322798));
#18393=CARTESIAN_POINT('Ctrl Pts',(-9.51642831724056,0.00974174196532851,
24.554119365528));
#18394=CARTESIAN_POINT('Ctrl Pts',(-9.51645943884196,0.00649459406771764,
24.5542718995425));
#18395=CARTESIAN_POINT('Ctrl Pts',(-9.51647499999999,0.00324729703478898,
24.554424433557));
#18396=CARTESIAN_POINT('Ctrl Pts',(-9.516475,1.40381758664725E-12,24.5545769675715));
#18397=CARTESIAN_POINT('Origin',(-8.5,0.,1.24542303242842));
#18398=CARTESIAN_POINT('',(-9.516475,1.33304090828571E-12,23.8954230324284));
#18399=CARTESIAN_POINT('',(-9.51638018545619,9.50640762730683E-5,23.9545769675715));
#18400=CARTESIAN_POINT('',(-9.516475,1.78524650477582E-12,1.24542303242842));
#18401=CARTESIAN_POINT('Ctrl Pts',(-9.516475,1.33304090828571E-12,23.8954230324284));
#18402=CARTESIAN_POINT('Ctrl Pts',(-9.51647500000035,-0.265706620582636,
23.9079039656766));
#18403=CARTESIAN_POINT('Ctrl Pts',(-9.40727465387265,-0.52978687817595,
23.9203848989248));
#18404=CARTESIAN_POINT('Ctrl Pts',(-9.2196169190785,-0.717894780173928,
23.932865832173));
#18405=CARTESIAN_POINT('Ctrl Pts',(-9.03195918428434,-0.906002682171906,
23.9453467654212));
#18406=CARTESIAN_POINT('Ctrl Pts',(-8.76814132834485,-1.01583545019881,
23.9578276986694));
#18407=CARTESIAN_POINT('Ctrl Pts',(-8.5024354704461,-1.0164720823066,23.9703086319176));
#18408=CARTESIAN_POINT('Ctrl Pts',(-8.23672961254735,-1.01710871441438,
23.9827895651658));
#18409=CARTESIAN_POINT('Ctrl Pts',(-7.97238846933429,-0.908541417083304,
23.995270498414));
#18410=CARTESIAN_POINT('Ctrl Pts',(-7.78383148002414,-0.721334926799325,
24.0077514316622));
#18411=CARTESIAN_POINT('Ctrl Pts',(-7.59527449071399,-0.534128436515345,
24.0202323649103));
#18412=CARTESIAN_POINT('Ctrl Pts',(-7.48480993131731,-0.270574496756787,
24.0327132981585));
#18413=CARTESIAN_POINT('Ctrl Pts',(-7.48353667075686,-0.00487092690929986,
24.0451942314067));
#18414=CARTESIAN_POINT('Ctrl Pts',(-7.48226341019641,0.260832642938187,
24.0576751646549));
#18415=CARTESIAN_POINT('Ctrl Pts',(-7.59019703546697,0.525433154239499,
24.0701560979031));
#18416=CARTESIAN_POINT('Ctrl Pts',(-7.77695120652445,0.714438148392532,
24.0826370311513));
#18417=CARTESIAN_POINT('Ctrl Pts',(-7.96370537758192,0.903443142545565,
24.0951179643995));
#18418=CARTESIAN_POINT('Ctrl Pts',(-8.22699388814725,1.01453885915631,24.1075988976477));
#18419=CARTESIAN_POINT('Ctrl Pts',(-8.49269364459055,1.01644874085988,24.1200798308959));
#18420=CARTESIAN_POINT('Ctrl Pts',(-8.75839340103385,1.01835862256344,24.1325607641441));
#18421=CARTESIAN_POINT('Ctrl Pts',(-9.02325176140295,0.911059288979515,
24.1450416973922));
#18422=CARTESIAN_POINT('Ctrl Pts',(-9.21270367535768,0.724758509268197,
24.1575226306404));
#18423=CARTESIAN_POINT('Ctrl Pts',(-9.4021555893124,0.538457729556879,24.1700035638886));
#18424=CARTESIAN_POINT('Ctrl Pts',(-9.51388182535815,0.275436159673321,
24.1824844971368));
#18425=CARTESIAN_POINT('Ctrl Pts',(-9.51642831724056,0.00974174196522188,
24.194965430385));
#18426=CARTESIAN_POINT('Ctrl Pts',(-9.51645943884196,0.00649459406763026,
24.1951179643995));
#18427=CARTESIAN_POINT('Ctrl Pts',(-9.516475,0.0032472970347209,24.195270498414));
#18428=CARTESIAN_POINT('Ctrl Pts',(-9.516475,1.3549573406767E-12,24.1954230324284));
#18429=CARTESIAN_POINT('Ctrl Pts',(-9.516475,1.30220480767874E-12,23.9545769675715));
#18430=CARTESIAN_POINT('Ctrl Pts',(-9.51647500000034,-0.265706620582667,
23.9670579008197));
#18431=CARTESIAN_POINT('Ctrl Pts',(-9.40727465387263,-0.529786878175978,
23.9795388340678));
#18432=CARTESIAN_POINT('Ctrl Pts',(-9.21961691907847,-0.71789478017395,
23.992019767316));
#18433=CARTESIAN_POINT('Ctrl Pts',(-9.03195918428432,-0.906002682171922,
24.0045007005642));
#18434=CARTESIAN_POINT('Ctrl Pts',(-8.76814132834482,-1.01583545019881,
24.0169816338124));
#18435=CARTESIAN_POINT('Ctrl Pts',(-8.50243547044607,-1.0164720823066,24.0294625670606));
#18436=CARTESIAN_POINT('Ctrl Pts',(-8.23672961254731,-1.01710871441438,
24.0419435003088));
#18437=CARTESIAN_POINT('Ctrl Pts',(-7.97238846933426,-0.908541417083288,
24.054424433557));
#18438=CARTESIAN_POINT('Ctrl Pts',(-7.78383148002412,-0.721334926799303,
24.0669053668052));
#18439=CARTESIAN_POINT('Ctrl Pts',(-7.59527449071398,-0.534128436515318,
24.0793863000534));
#18440=CARTESIAN_POINT('Ctrl Pts',(-7.4848099313173,-0.270574496756756,
24.0918672333016));
#18441=CARTESIAN_POINT('Ctrl Pts',(-7.48353667075686,-0.00487092690926902,
24.1043481665497));
#18442=CARTESIAN_POINT('Ctrl Pts',(-7.48226341019642,0.260832642938218,
24.1168290997979));
#18443=CARTESIAN_POINT('Ctrl Pts',(-7.59019703546699,0.525433154239526,
24.1293100330461));
#18444=CARTESIAN_POINT('Ctrl Pts',(-7.77695120652447,0.714438148392554,
24.1417909662943));
#18445=CARTESIAN_POINT('Ctrl Pts',(-7.96370537758195,0.903443142545582,
24.1542718995425));
#18446=CARTESIAN_POINT('Ctrl Pts',(-8.22699388814728,1.01453885915632,24.1667528327907));
#18447=CARTESIAN_POINT('Ctrl Pts',(-8.49269364459058,1.01644874085988,24.1792337660389));
#18448=CARTESIAN_POINT('Ctrl Pts',(-8.75839340103389,1.01835862256343,24.1917146992871));
#18449=CARTESIAN_POINT('Ctrl Pts',(-9.02325176140298,0.9110592889795,24.2041956325353));
#18450=CARTESIAN_POINT('Ctrl Pts',(-9.2127036753577,0.724758509268176,24.2166765657835));
#18451=CARTESIAN_POINT('Ctrl Pts',(-9.40215558931242,0.538457729556852,
24.2291574990317));
#18452=CARTESIAN_POINT('Ctrl Pts',(-9.51388182535815,0.27543615967329,24.2416384322798));
#18453=CARTESIAN_POINT('Ctrl Pts',(-9.51642831724056,0.00974174196519104,
24.254119365528));
#18454=CARTESIAN_POINT('Ctrl Pts',(-9.51645943884196,0.00649459406763794,
24.2542718995425));
#18455=CARTESIAN_POINT('Ctrl Pts',(-9.51647499999999,0.00324729703476719,
24.254424433557));
#18456=CARTESIAN_POINT('Ctrl Pts',(-9.516475,1.43968106844281E-12,24.2545769675715));
#18457=CARTESIAN_POINT('Origin',(-8.5,0.,1.24542303242842));
#18458=CARTESIAN_POINT('',(-9.516475,1.31112447589473E-12,23.5954230324284));
#18459=CARTESIAN_POINT('',(-9.51682532410723,4.86896733354835E-5,23.6545769675715));
#18460=CARTESIAN_POINT('',(-9.516475,1.78524650477582E-12,1.24542303242842));
#18461=CARTESIAN_POINT('Ctrl Pts',(-9.516475,1.36890439008127E-12,23.5954230324284));
#18462=CARTESIAN_POINT('Ctrl Pts',(-9.51647500000036,-0.265706620582619,
23.6079039656766));
#18463=CARTESIAN_POINT('Ctrl Pts',(-9.40727465387265,-0.529786878175956,
23.6203848989248));
#18464=CARTESIAN_POINT('Ctrl Pts',(-9.21961691907848,-0.717894780173944,
23.632865832173));
#18465=CARTESIAN_POINT('Ctrl Pts',(-9.03195918428431,-0.906002682171931,
23.6453467654212));
#18466=CARTESIAN_POINT('Ctrl Pts',(-8.76814132834479,-1.01583545019883,
23.6578276986694));
#18467=CARTESIAN_POINT('Ctrl Pts',(-8.50243547044602,-1.0164720823066,23.6703086319176));
#18468=CARTESIAN_POINT('Ctrl Pts',(-8.23672961254725,-1.01710871441436,
23.6827895651658));
#18469=CARTESIAN_POINT('Ctrl Pts',(-7.97238846933418,-0.908541417083246,
23.695270498414));
#18470=CARTESIAN_POINT('Ctrl Pts',(-7.78383148002404,-0.721334926799228,
23.7077514316622));
#18471=CARTESIAN_POINT('Ctrl Pts',(-7.59527449071391,-0.534128436515209,
23.7202323649103));
#18472=CARTESIAN_POINT('Ctrl Pts',(-7.48480993131726,-0.270574496756611,
23.7327132981585));
#18473=CARTESIAN_POINT('Ctrl Pts',(-7.48353667075686,-0.00487092690910461,
23.7451942314067));
#18474=CARTESIAN_POINT('Ctrl Pts',(-7.48226341019646,0.260832642938402,
23.7576751646549));
#18475=CARTESIAN_POINT('Ctrl Pts',(-7.59019703546709,0.525433154239711,
23.7701560979031));
#18476=CARTESIAN_POINT('Ctrl Pts',(-7.77695120652463,0.714438148392712,
23.7826370311513));
#18477=CARTESIAN_POINT('Ctrl Pts',(-7.96370537758216,0.903443142545713,
23.7951179643995));
#18478=CARTESIAN_POINT('Ctrl Pts',(-8.22699388814754,1.0145388591564,23.8075988976477));
#18479=CARTESIAN_POINT('Ctrl Pts',(-8.49269364459086,1.01644874085988,23.8200798308959));
#18480=CARTESIAN_POINT('Ctrl Pts',(-8.75839340103419,1.01835862256336,23.8325607641441));
#18481=CARTESIAN_POINT('Ctrl Pts',(-9.02325176140327,0.911059288979339,
23.8450416973923));
#18482=CARTESIAN_POINT('Ctrl Pts',(-9.21270367535794,0.724758509267939,
23.8575226306405));
#18483=CARTESIAN_POINT('Ctrl Pts',(-9.40215558931261,0.538457729556538,
23.8700035638886));
#18484=CARTESIAN_POINT('Ctrl Pts',(-9.51388182535826,0.275436159672915,
23.8824844971368));
#18485=CARTESIAN_POINT('Ctrl Pts',(-9.51642831724057,0.00974174196479552,
23.894965430385));
#18486=CARTESIAN_POINT('Ctrl Pts',(-9.51645943884196,0.0064945940673387,
23.8951179643995));
#18487=CARTESIAN_POINT('Ctrl Pts',(-9.516475,0.00324729703456413,23.895270498414));
#18488=CARTESIAN_POINT('Ctrl Pts',(-9.516475,1.33304090828571E-12,23.8954230324284));
#18489=CARTESIAN_POINT('Ctrl Pts',(-9.51796493798108,0.000207078507120715,
23.6545769675715));
#18490=CARTESIAN_POINT('Ctrl Pts',(-9.51706691021463,-0.325585595105403,
23.669948946367));
#18491=CARTESIAN_POINT('Ctrl Pts',(-9.17147099560746,-0.99017940908471,
23.7012282663142));
#18492=CARTESIAN_POINT('Ctrl Pts',(-8.03686629447588,-1.10987867419518,
23.7484149274131));
#18493=CARTESIAN_POINT('Ctrl Pts',(-7.43826157375447,-0.361085119319684,
23.7881832802921));
#18494=CARTESIAN_POINT('Ctrl Pts',(-7.49794123728335,0.335385184319912,
23.8199979625954));
#18495=CARTESIAN_POINT('Ctrl Pts',(-7.86953258335037,0.927459856653405,
23.8518126448985));
#18496=CARTESIAN_POINT('Ctrl Pts',(-8.79827787305733,1.16505528240947,23.8915809977777));
#18497=CARTESIAN_POINT('Ctrl Pts',(-9.45053929968385,0.556114497354683,
23.9284869955272));
#18498=CARTESIAN_POINT('Ctrl Pts',(-9.51659141321842,0.1093069840508,23.9494856521251));
#18499=CARTESIAN_POINT('Ctrl Pts',(-9.51572863211466,0.000748332163859972,
23.9545769675715));
#18500=CARTESIAN_POINT('Origin',(-8.5,0.,1.24542303242842));
#18501=CARTESIAN_POINT('',(-9.516475,1.28920804350374E-12,23.2954230324284));
#18502=CARTESIAN_POINT('',(-9.516475,1.31615185708331E-12,23.3545769675715));
#18503=CARTESIAN_POINT('',(-9.516475,1.78524650477582E-12,1.24542303242842));
#18504=CARTESIAN_POINT('Ctrl Pts',(-9.516475,1.34698795769028E-12,23.2954230324284));
#18505=CARTESIAN_POINT('Ctrl Pts',(-9.51647500000035,-0.265706620582641,
23.3079039656766));
#18506=CARTESIAN_POINT('Ctrl Pts',(-9.40727465387264,-0.529786878175976,
23.3203848989248));
#18507=CARTESIAN_POINT('Ctrl Pts',(-9.21961691907847,-0.717894780173959,
23.332865832173));
#18508=CARTESIAN_POINT('Ctrl Pts',(-9.03195918428429,-0.906002682171943,
23.3453467654212));
#18509=CARTESIAN_POINT('Ctrl Pts',(-8.76814132834477,-1.01583545019883,
23.3578276986694));
#18510=CARTESIAN_POINT('Ctrl Pts',(-8.502435470446,-1.0164720823066,23.3703086319176));
#18511=CARTESIAN_POINT('Ctrl Pts',(-8.23672961254722,-1.01710871441436,
23.3827895651658));
#18512=CARTESIAN_POINT('Ctrl Pts',(-7.97238846933416,-0.908541417083235,
23.395270498414));
#18513=CARTESIAN_POINT('Ctrl Pts',(-7.78383148002403,-0.721334926799212,
23.4077514316622));
#18514=CARTESIAN_POINT('Ctrl Pts',(-7.5952744907139,-0.53412843651519,23.4202323649104));
#18515=CARTESIAN_POINT('Ctrl Pts',(-7.48480993131725,-0.270574496756589,
23.4327132981585));
#18516=CARTESIAN_POINT('Ctrl Pts',(-7.48353667075686,-0.00487092690908269,
23.4451942314067));
#18517=CARTESIAN_POINT('Ctrl Pts',(-7.48226341019647,0.260832642938424,
23.4576751646549));
#18518=CARTESIAN_POINT('Ctrl Pts',(-7.5901970354671,0.525433154239731,23.4701560979031));
#18519=CARTESIAN_POINT('Ctrl Pts',(-7.77695120652464,0.714438148392727,
23.4826370311513));
#18520=CARTESIAN_POINT('Ctrl Pts',(-7.96370537758218,0.903443142545724,
23.4951179643995));
#18521=CARTESIAN_POINT('Ctrl Pts',(-8.22699388814756,1.0145388591564,23.5075988976477));
#18522=CARTESIAN_POINT('Ctrl Pts',(-8.49269364459088,1.01644874085988,23.5200798308959));
#18523=CARTESIAN_POINT('Ctrl Pts',(-8.75839340103421,1.01835862256336,23.5325607641441));
#18524=CARTESIAN_POINT('Ctrl Pts',(-9.02325176140329,0.911059288979328,
23.5450416973923));
#18525=CARTESIAN_POINT('Ctrl Pts',(-9.21270367535795,0.724758509267924,
23.5575226306405));
#18526=CARTESIAN_POINT('Ctrl Pts',(-9.40215558931262,0.538457729556519,
23.5700035638886));
#18527=CARTESIAN_POINT('Ctrl Pts',(-9.51388182535827,0.275436159672893,
23.5824844971368));
#18528=CARTESIAN_POINT('Ctrl Pts',(-9.51642831724057,0.00974174196477361,
23.594965430385));
#18529=CARTESIAN_POINT('Ctrl Pts',(-9.51645943884196,0.00649459406733604,
23.5951179643995));
#18530=CARTESIAN_POINT('Ctrl Pts',(-9.516475,0.00324729703458077,23.595270498414));
#18531=CARTESIAN_POINT('Ctrl Pts',(-9.516475,1.36890439008127E-12,23.5954230324284));
#18532=CARTESIAN_POINT('Ctrl Pts',(-9.516475,1.43171168545639E-12,23.3545769675715));
#18533=CARTESIAN_POINT('Ctrl Pts',(-9.51647500000037,-0.265706620582537,
23.3670579008196));
#18534=CARTESIAN_POINT('Ctrl Pts',(-9.4072746538727,-0.529786878175862,
23.3795388340678));
#18535=CARTESIAN_POINT('Ctrl Pts',(-9.21961691907857,-0.717894780173858,
23.392019767316));
#18536=CARTESIAN_POINT('Ctrl Pts',(-9.03195918428443,-0.906002682171854,
23.4045007005642));
#18537=CARTESIAN_POINT('Ctrl Pts',(-8.76814132834495,-1.01583545019878,
23.4169816338124));
#18538=CARTESIAN_POINT('Ctrl Pts',(-8.5024354704462,-1.0164720823066,23.4294625670606));
#18539=CARTESIAN_POINT('Ctrl Pts',(-8.23672961254744,-1.01710871441441,
23.4419435003088));
#18540=CARTESIAN_POINT('Ctrl Pts',(-7.97238846933438,-0.908541417083355,
23.454424433557));
#18541=CARTESIAN_POINT('Ctrl Pts',(-7.78383148002421,-0.721334926799394,
23.4669053668052));
#18542=CARTESIAN_POINT('Ctrl Pts',(-7.59527449071404,-0.534128436515433,
23.4793863000534));
#18543=CARTESIAN_POINT('Ctrl Pts',(-7.48480993131734,-0.270574496756885,
23.4918672333016));
#18544=CARTESIAN_POINT('Ctrl Pts',(-7.48353667075686,-0.00487092690939853,
23.5043481665497));
#18545=CARTESIAN_POINT('Ctrl Pts',(-7.48226341019639,0.260832642938088,
23.5168290997979));
#18546=CARTESIAN_POINT('Ctrl Pts',(-7.59019703546692,0.52543315423941,23.5293100330461));
#18547=CARTESIAN_POINT('Ctrl Pts',(-7.77695120652438,0.714438148392462,
23.5417909662943));
#18548=CARTESIAN_POINT('Ctrl Pts',(-7.96370537758184,0.903443142545513,
23.5542718995425));
#18549=CARTESIAN_POINT('Ctrl Pts',(-8.22699388814715,1.01453885915629,23.5667528327907));
#18550=CARTESIAN_POINT('Ctrl Pts',(-8.49269364459045,1.01644874085988,23.5792337660389));
#18551=CARTESIAN_POINT('Ctrl Pts',(-8.75839340103376,1.01835862256347,23.5917146992871));
#18552=CARTESIAN_POINT('Ctrl Pts',(-9.02325176140286,0.911059288979566,
23.6041956325353));
#18553=CARTESIAN_POINT('Ctrl Pts',(-9.21270367535761,0.724758509268266,
23.6166765657835));
#18554=CARTESIAN_POINT('Ctrl Pts',(-9.40215558931235,0.538457729556966,
23.6291574990316));
#18555=CARTESIAN_POINT('Ctrl Pts',(-9.51388182535812,0.275436159673419,
23.6416384322798));
#18556=CARTESIAN_POINT('Ctrl Pts',(-9.51642831724056,0.00974174196532054,
23.654119365528));
#18557=CARTESIAN_POINT('Ctrl Pts',(-9.51645943884196,0.00649459406769041,
23.6542718995425));
#18558=CARTESIAN_POINT('Ctrl Pts',(-9.516475,0.00324729703474261,23.654424433557));
#18559=CARTESIAN_POINT('Ctrl Pts',(-9.516475,1.3380682894743E-12,23.6545769675715));
#18560=CARTESIAN_POINT('Origin',(-8.5,0.,1.24542303242842));
#18561=CARTESIAN_POINT('',(-9.516475,1.26729161111276E-12,22.9954230324284));
#18562=CARTESIAN_POINT('',(-9.516475,1.29423542469233E-12,23.0545769675715));
#18563=CARTESIAN_POINT('',(-9.516475,1.78524650477582E-12,1.24542303242842));
#18564=CARTESIAN_POINT('Ctrl Pts',(-9.516475,1.26729161111276E-12,22.9954230324284));
#18565=CARTESIAN_POINT('Ctrl Pts',(-9.51647500000033,-0.265706620582721,
23.0079039656766));
#18566=CARTESIAN_POINT('Ctrl Pts',(-9.4072746538726,-0.529786878176047,
23.0203848989248));
#18567=CARTESIAN_POINT('Ctrl Pts',(-9.21961691907841,-0.717894780174016,
23.032865832173));
#18568=CARTESIAN_POINT('Ctrl Pts',(-9.03195918428422,-0.906002682171985,
23.0453467654212));
#18569=CARTESIAN_POINT('Ctrl Pts',(-8.76814132834469,-1.01583545019885,
23.0578276986694));
#18570=CARTESIAN_POINT('Ctrl Pts',(-8.50243547044592,-1.0164720823066,23.0703086319176));
#18571=CARTESIAN_POINT('Ctrl Pts',(-8.23672961254715,-1.01710871441434,
23.0827895651658));
#18572=CARTESIAN_POINT('Ctrl Pts',(-7.97238846933409,-0.908541417083194,
23.095270498414));
#18573=CARTESIAN_POINT('Ctrl Pts',(-7.78383148002397,-0.721334926799156,
23.1077514316622));
#18574=CARTESIAN_POINT('Ctrl Pts',(-7.59527449071385,-0.534128436515119,
23.1202323649104));
#18575=CARTESIAN_POINT('Ctrl Pts',(-7.48480993131723,-0.270574496756509,
23.1327132981585));
#18576=CARTESIAN_POINT('Ctrl Pts',(-7.48353667075686,-0.00487092690900299,
23.1451942314067));
#18577=CARTESIAN_POINT('Ctrl Pts',(-7.48226341019649,0.260832642938503,
23.1576751646549));
#18578=CARTESIAN_POINT('Ctrl Pts',(-7.59019703546714,0.525433154239802,
23.1701560979031));
#18579=CARTESIAN_POINT('Ctrl Pts',(-7.7769512065247,0.714438148392784,23.1826370311513));
#18580=CARTESIAN_POINT('Ctrl Pts',(-7.96370537758225,0.903443142545766,
23.1951179643995));
#18581=CARTESIAN_POINT('Ctrl Pts',(-8.22699388814764,1.01453885915642,23.2075988976477));
#18582=CARTESIAN_POINT('Ctrl Pts',(-8.49269364459096,1.01644874085988,23.2200798308959));
#18583=CARTESIAN_POINT('Ctrl Pts',(-8.75839340103429,1.01835862256334,23.2325607641441));
#18584=CARTESIAN_POINT('Ctrl Pts',(-9.02325176140336,0.911059288979287,
23.2450416973923));
#18585=CARTESIAN_POINT('Ctrl Pts',(-9.21270367535801,0.724758509267868,
23.2575226306405));
#18586=CARTESIAN_POINT('Ctrl Pts',(-9.40215558931266,0.538457729556448,
23.2700035638887));
#18587=CARTESIAN_POINT('Ctrl Pts',(-9.51388182535829,0.275436159672814,
23.2824844971368));
#18588=CARTESIAN_POINT('Ctrl Pts',(-9.51642831724057,0.00974174196469391,
23.294965430385));
#18589=CARTESIAN_POINT('Ctrl Pts',(-9.51645943884196,0.00649459406727561,
23.2951179643995));
#18590=CARTESIAN_POINT('Ctrl Pts',(-9.516475,0.00324729703453964,23.295270498414));
#18591=CARTESIAN_POINT('Ctrl Pts',(-9.516475,1.34698795769028E-12,23.2954230324284));
#18592=CARTESIAN_POINT('Ctrl Pts',(-9.516475,1.35201533887887E-12,23.0545769675715));
#18593=CARTESIAN_POINT('Ctrl Pts',(-9.51647500000035,-0.265706620582617,
23.0670579008197));
#18594=CARTESIAN_POINT('Ctrl Pts',(-9.40727465387266,-0.529786878175934,
23.0795388340678));
#18595=CARTESIAN_POINT('Ctrl Pts',(-9.21961691907851,-0.717894780173915,
23.092019767316));
#18596=CARTESIAN_POINT('Ctrl Pts',(-9.03195918428436,-0.906002682171896,
23.1045007005642));
#18597=CARTESIAN_POINT('Ctrl Pts',(-8.76814132834487,-1.0158354501988,23.1169816338124));
#18598=CARTESIAN_POINT('Ctrl Pts',(-8.50243547044612,-1.0164720823066,23.1294625670606));
#18599=CARTESIAN_POINT('Ctrl Pts',(-8.23672961254736,-1.01710871441439,
23.1419435003088));
#18600=CARTESIAN_POINT('Ctrl Pts',(-7.97238846933431,-0.908541417083314,
23.154424433557));
#18601=CARTESIAN_POINT('Ctrl Pts',(-7.78383148002415,-0.721334926799338,
23.1669053668052));
#18602=CARTESIAN_POINT('Ctrl Pts',(-7.595274490714,-0.534128436515362,23.1793863000534));
#18603=CARTESIAN_POINT('Ctrl Pts',(-7.48480993131732,-0.270574496756806,
23.1918672333016));
#18604=CARTESIAN_POINT('Ctrl Pts',(-7.48353667075686,-0.00487092690931883,
23.2043481665497));
#18605=CARTESIAN_POINT('Ctrl Pts',(-7.48226341019641,0.260832642938168,
23.2168290997979));
#18606=CARTESIAN_POINT('Ctrl Pts',(-7.59019703546696,0.525433154239481,
23.2293100330461));
#18607=CARTESIAN_POINT('Ctrl Pts',(-7.77695120652444,0.714438148392518,
23.2417909662943));
#18608=CARTESIAN_POINT('Ctrl Pts',(-7.96370537758191,0.903443142545555,
23.2542718995425));
#18609=CARTESIAN_POINT('Ctrl Pts',(-8.22699388814723,1.01453885915631,23.2667528327907));
#18610=CARTESIAN_POINT('Ctrl Pts',(-8.49269364459053,1.01644874085988,23.2792337660389));
#18611=CARTESIAN_POINT('Ctrl Pts',(-8.75839340103384,1.01835862256345,23.2917146992871));
#18612=CARTESIAN_POINT('Ctrl Pts',(-9.02325176140294,0.911059288979525,
23.3041956325353));
#18613=CARTESIAN_POINT('Ctrl Pts',(-9.21270367535766,0.72475850926821,23.3166765657835));
#18614=CARTESIAN_POINT('Ctrl Pts',(-9.40215558931239,0.538457729556896,
23.3291574990317));
#18615=CARTESIAN_POINT('Ctrl Pts',(-9.51388182535814,0.27543615967334,23.3416384322798));
#18616=CARTESIAN_POINT('Ctrl Pts',(-9.51642831724056,0.00974174196524085,
23.354119365528));
#18617=CARTESIAN_POINT('Ctrl Pts',(-9.51645943884196,0.00649459406766849,
23.3542718995425));
#18618=CARTESIAN_POINT('Ctrl Pts',(-9.51647499999999,0.00324729703477843,
23.354424433557));
#18619=CARTESIAN_POINT('Ctrl Pts',(-9.516475,1.43171168545639E-12,23.3545769675715));
#18620=CARTESIAN_POINT('Origin',(-8.5,0.,1.24542303242842));
#18621=CARTESIAN_POINT('',(-9.516475,1.24537517872177E-12,22.6954230324284));
#18622=CARTESIAN_POINT('',(-9.516475,1.27231899230134E-12,22.7545769675715));
#18623=CARTESIAN_POINT('',(-9.516475,1.78524650477582E-12,1.24542303242842));
#18624=CARTESIAN_POINT('Ctrl Pts',(-9.516475,1.30315509290831E-12,22.6954230324284));
#18625=CARTESIAN_POINT('Ctrl Pts',(-9.51647500000034,-0.265706620582666,
22.7079039656766));
#18626=CARTESIAN_POINT('Ctrl Pts',(-9.40727465387263,-0.529786878175977,
22.7203848989248));
#18627=CARTESIAN_POINT('Ctrl Pts',(-9.21961691907848,-0.717894780173949,
22.732865832173));
#18628=CARTESIAN_POINT('Ctrl Pts',(-9.03195918428432,-0.906002682171922,
22.7453467654212));
#18629=CARTESIAN_POINT('Ctrl Pts',(-8.76814132834482,-1.01583545019881,
22.7578276986694));
#18630=CARTESIAN_POINT('Ctrl Pts',(-8.50243547044607,-1.0164720823066,22.7703086319176));
#18631=CARTESIAN_POINT('Ctrl Pts',(-8.23672961254732,-1.01710871441438,
22.7827895651658));
#18632=CARTESIAN_POINT('Ctrl Pts',(-7.97238846933426,-0.908541417083289,
22.795270498414));
#18633=CARTESIAN_POINT('Ctrl Pts',(-7.78383148002412,-0.721334926799304,
22.8077514316622));
#18634=CARTESIAN_POINT('Ctrl Pts',(-7.59527449071398,-0.534128436515318,
22.8202323649103));
#18635=CARTESIAN_POINT('Ctrl Pts',(-7.4848099313173,-0.270574496756757,
22.8327132981585));
#18636=CARTESIAN_POINT('Ctrl Pts',(-7.48353667075686,-0.00487092690926997,
22.8451942314067));
#18637=CARTESIAN_POINT('Ctrl Pts',(-7.48226341019642,0.260832642938217,
22.8576751646549));
#18638=CARTESIAN_POINT('Ctrl Pts',(-7.59019703546699,0.525433154239525,
22.8701560979031));
#18639=CARTESIAN_POINT('Ctrl Pts',(-7.77695120652447,0.714438148392553,
22.8826370311513));
#18640=CARTESIAN_POINT('Ctrl Pts',(-7.96370537758195,0.903443142545581,
22.8951179643995));
#18641=CARTESIAN_POINT('Ctrl Pts',(-8.22699388814728,1.01453885915632,22.9075988976477));
#18642=CARTESIAN_POINT('Ctrl Pts',(-8.49269364459058,1.01644874085988,22.9200798308959));
#18643=CARTESIAN_POINT('Ctrl Pts',(-8.75839340103389,1.01835862256343,22.9325607641441));
#18644=CARTESIAN_POINT('Ctrl Pts',(-9.02325176140298,0.9110592889795,22.9450416973922));
#18645=CARTESIAN_POINT('Ctrl Pts',(-9.2127036753577,0.724758509268176,22.9575226306404));
#18646=CARTESIAN_POINT('Ctrl Pts',(-9.40215558931242,0.538457729556853,
22.9700035638886));
#18647=CARTESIAN_POINT('Ctrl Pts',(-9.51388182535815,0.275436159673291,
22.9824844971368));
#18648=CARTESIAN_POINT('Ctrl Pts',(-9.51642831724056,0.00974174196519199,
22.994965430385));
#18649=CARTESIAN_POINT('Ctrl Pts',(-9.51645943884196,0.00649459406758111,
22.9951179643995));
#18650=CARTESIAN_POINT('Ctrl Pts',(-9.516475,0.00324729703465245,22.995270498414));
#18651=CARTESIAN_POINT('Ctrl Pts',(-9.516475,1.26729161111276E-12,22.9954230324284));
#18652=CARTESIAN_POINT('Ctrl Pts',(-9.516475,1.33009890648788E-12,22.7545769675715));
#18653=CARTESIAN_POINT('Ctrl Pts',(-9.51647500000035,-0.265706620582639,
22.7670579008197));
#18654=CARTESIAN_POINT('Ctrl Pts',(-9.40727465387265,-0.529786878175953,
22.7795388340678));
#18655=CARTESIAN_POINT('Ctrl Pts',(-9.21961691907849,-0.71789478017393,
22.792019767316));
#18656=CARTESIAN_POINT('Ctrl Pts',(-9.03195918428434,-0.906002682171908,
22.8045007005642));
#18657=CARTESIAN_POINT('Ctrl Pts',(-8.76814132834485,-1.01583545019881,
22.8169816338124));
#18658=CARTESIAN_POINT('Ctrl Pts',(-8.5024354704461,-1.0164720823066,22.8294625670606));
#18659=CARTESIAN_POINT('Ctrl Pts',(-8.23672961254734,-1.01710871441438,
22.8419435003088));
#18660=CARTESIAN_POINT('Ctrl Pts',(-7.97238846933429,-0.908541417083303,
22.854424433557));
#18661=CARTESIAN_POINT('Ctrl Pts',(-7.78383148002414,-0.721334926799323,
22.8669053668052));
#18662=CARTESIAN_POINT('Ctrl Pts',(-7.59527449071399,-0.534128436515342,
22.8793863000534));
#18663=CARTESIAN_POINT('Ctrl Pts',(-7.48480993131731,-0.270574496756784,
22.8918672333016));
#18664=CARTESIAN_POINT('Ctrl Pts',(-7.48353667075686,-0.00487092690929692,
22.9043481665497));
#18665=CARTESIAN_POINT('Ctrl Pts',(-7.48226341019642,0.26083264293819,22.9168290997979));
#18666=CARTESIAN_POINT('Ctrl Pts',(-7.59019703546697,0.525433154239501,
22.9293100330461));
#18667=CARTESIAN_POINT('Ctrl Pts',(-7.77695120652445,0.714438148392534,
22.9417909662943));
#18668=CARTESIAN_POINT('Ctrl Pts',(-7.96370537758193,0.903443142545567,
22.9542718995425));
#18669=CARTESIAN_POINT('Ctrl Pts',(-8.22699388814725,1.01453885915631,22.9667528327907));
#18670=CARTESIAN_POINT('Ctrl Pts',(-8.49269364459055,1.01644874085988,22.9792337660389));
#18671=CARTESIAN_POINT('Ctrl Pts',(-8.75839340103386,1.01835862256344,22.9917146992871));
#18672=CARTESIAN_POINT('Ctrl Pts',(-9.02325176140296,0.911059288979514,
23.0041956325353));
#18673=CARTESIAN_POINT('Ctrl Pts',(-9.21270367535768,0.724758509268195,
23.0166765657835));
#18674=CARTESIAN_POINT('Ctrl Pts',(-9.4021555893124,0.538457729556876,23.0291574990317));
#18675=CARTESIAN_POINT('Ctrl Pts',(-9.51388182535815,0.275436159673318,
23.0416384322798));
#18676=CARTESIAN_POINT('Ctrl Pts',(-9.51642831724056,0.00974174196521894,
23.054119365528));
#18677=CARTESIAN_POINT('Ctrl Pts',(-9.51645943884196,0.00649459406762731,
23.0542718995425));
#18678=CARTESIAN_POINT('Ctrl Pts',(-9.516475,0.00324729703471796,23.054424433557));
#18679=CARTESIAN_POINT('Ctrl Pts',(-9.516475,1.35201533887887E-12,23.0545769675715));
#18680=CARTESIAN_POINT('Origin',(-8.5,0.,1.24542303242842));
#18681=CARTESIAN_POINT('',(-9.5160605096938,-0.00010514095004287,22.3954230324284));
#18682=CARTESIAN_POINT('',(-9.516475,1.25040255991036E-12,22.4545769675715));
#18683=CARTESIAN_POINT('',(-9.516475,1.78524650477582E-12,1.24542303242842));
#18684=CARTESIAN_POINT('Ctrl Pts',(-9.516475,1.28123866051733E-12,22.3954230324284));
#18685=CARTESIAN_POINT('Ctrl Pts',(-9.51647500000034,-0.265706620582688,
22.4079039656766));
#18686=CARTESIAN_POINT('Ctrl Pts',(-9.40727465387262,-0.529786878175997,
22.4203848989248));
#18687=CARTESIAN_POINT('Ctrl Pts',(-9.21961691907846,-0.717894780173965,
22.432865832173));
#18688=CARTESIAN_POINT('Ctrl Pts',(-9.0319591842843,-0.906002682171933,
22.4453467654212));
#18689=CARTESIAN_POINT('Ctrl Pts',(-8.7681413283448,-1.01583545019882,22.4578276986694));
#18690=CARTESIAN_POINT('Ctrl Pts',(-8.50243547044605,-1.0164720823066,22.4703086319176));
#18691=CARTESIAN_POINT('Ctrl Pts',(-8.23672961254729,-1.01710871441437,
22.4827895651658));
#18692=CARTESIAN_POINT('Ctrl Pts',(-7.97238846933424,-0.908541417083277,
22.495270498414));
#18693=CARTESIAN_POINT('Ctrl Pts',(-7.7838314800241,-0.721334926799288,
22.5077514316622));
#18694=CARTESIAN_POINT('Ctrl Pts',(-7.59527449071397,-0.534128436515299,
22.5202323649103));
#18695=CARTESIAN_POINT('Ctrl Pts',(-7.4848099313173,-0.270574496756735,
22.5327132981585));
#18696=CARTESIAN_POINT('Ctrl Pts',(-7.48353667075686,-0.00487092690924806,
22.5451942314067));
#18697=CARTESIAN_POINT('Ctrl Pts',(-7.48226341019643,0.260832642938239,
22.5576751646549));
#18698=CARTESIAN_POINT('Ctrl Pts',(-7.590197035467,0.525433154239545,22.5701560979031));
#18699=CARTESIAN_POINT('Ctrl Pts',(-7.77695120652449,0.714438148392569,
22.5826370311513));
#18700=CARTESIAN_POINT('Ctrl Pts',(-7.96370537758197,0.903443142545593,
22.5951179643995));
#18701=CARTESIAN_POINT('Ctrl Pts',(-8.2269938881473,1.01453885915633,22.6075988976477));
#18702=CARTESIAN_POINT('Ctrl Pts',(-8.4926936445906,1.01644874085988,22.6200798308959));
#18703=CARTESIAN_POINT('Ctrl Pts',(-8.75839340103391,1.01835862256343,22.6325607641441));
#18704=CARTESIAN_POINT('Ctrl Pts',(-9.023251761403,0.911059288979489,22.6450416973922));
#18705=CARTESIAN_POINT('Ctrl Pts',(-9.21270367535771,0.724758509268161,
22.6575226306404));
#18706=CARTESIAN_POINT('Ctrl Pts',(-9.40215558931243,0.538457729556833,
22.6700035638886));
#18707=CARTESIAN_POINT('Ctrl Pts',(-9.51388182535816,0.275436159673269,
22.6824844971368));
#18708=CARTESIAN_POINT('Ctrl Pts',(-9.51642831724056,0.00974174196517008,
22.694965430385));
#18709=CARTESIAN_POINT('Ctrl Pts',(-9.51645943884196,0.00649459406757845,
22.6951179643995));
#18710=CARTESIAN_POINT('Ctrl Pts',(-9.516475,0.0032472970346691,22.695270498414));
#18711=CARTESIAN_POINT('Ctrl Pts',(-9.516475,1.30315509290831E-12,22.6954230324284));
#18712=CARTESIAN_POINT('Ctrl Pts',(-9.516475,1.25040255991036E-12,22.4545769675715));
#18713=CARTESIAN_POINT('Ctrl Pts',(-9.51647500000033,-0.265706620582718,
22.4670579008197));
#18714=CARTESIAN_POINT('Ctrl Pts',(-9.4072746538726,-0.529786878176024,
22.4795388340678));
#18715=CARTESIAN_POINT('Ctrl Pts',(-9.21961691907844,-0.717894780173987,
22.492019767316));
#18716=CARTESIAN_POINT('Ctrl Pts',(-9.03195918428427,-0.906002682171949,
22.5045007005642));
#18717=CARTESIAN_POINT('Ctrl Pts',(-8.76814132834477,-1.01583545019883,
22.5169816338124));
#18718=CARTESIAN_POINT('Ctrl Pts',(-8.50243547044602,-1.0164720823066,22.5294625670606));
#18719=CARTESIAN_POINT('Ctrl Pts',(-8.23672961254726,-1.01710871441436,
22.5419435003088));
#18720=CARTESIAN_POINT('Ctrl Pts',(-7.97238846933422,-0.908541417083261,
22.554424433557));
#18721=CARTESIAN_POINT('Ctrl Pts',(-7.78383148002408,-0.721334926799266,
22.5669053668052));
#18722=CARTESIAN_POINT('Ctrl Pts',(-7.59527449071395,-0.534128436515272,
22.5793863000534));
#18723=CARTESIAN_POINT('Ctrl Pts',(-7.48480993131729,-0.270574496756704,
22.5918672333016));
#18724=CARTESIAN_POINT('Ctrl Pts',(-7.48353667075686,-0.00487092690921722,
22.6043481665498));
#18725=CARTESIAN_POINT('Ctrl Pts',(-7.48226341019643,0.26083264293827,22.6168290997979));
#18726=CARTESIAN_POINT('Ctrl Pts',(-7.59019703546702,0.525433154239572,
22.6293100330461));
#18727=CARTESIAN_POINT('Ctrl Pts',(-7.77695120652451,0.714438148392591,
22.6417909662943));
#18728=CARTESIAN_POINT('Ctrl Pts',(-7.963705377582,0.903443142545609,22.6542718995425));
#18729=CARTESIAN_POINT('Ctrl Pts',(-8.22699388814733,1.01453885915634,22.6667528327907));
#18730=CARTESIAN_POINT('Ctrl Pts',(-8.49269364459063,1.01644874085988,22.6792337660389));
#18731=CARTESIAN_POINT('Ctrl Pts',(-8.75839340103394,1.01835862256342,22.6917146992871));
#18732=CARTESIAN_POINT('Ctrl Pts',(-9.02325176140303,0.911059288979473,
22.7041956325353));
#18733=CARTESIAN_POINT('Ctrl Pts',(-9.21270367535774,0.724758509268139,
22.7166765657835));
#18734=CARTESIAN_POINT('Ctrl Pts',(-9.40215558931244,0.538457729556806,
22.7291574990317));
#18735=CARTESIAN_POINT('Ctrl Pts',(-9.51388182535817,0.275436159673239,
22.7416384322798));
#18736=CARTESIAN_POINT('Ctrl Pts',(-9.51642831724056,0.00974174196513924,
22.754119365528));
#18737=CARTESIAN_POINT('Ctrl Pts',(-9.51645943884196,0.00649459406756688,
22.7542718995425));
#18738=CARTESIAN_POINT('Ctrl Pts',(-9.516475,0.00324729703467682,22.754424433557));
#18739=CARTESIAN_POINT('Ctrl Pts',(-9.516475,1.33009890648788E-12,22.7545769675715));
#18740=CARTESIAN_POINT('Origin',(-8.5,0.,1.24542303242842));
#18741=CARTESIAN_POINT('',(-9.51589627264183,0.00088909351918253,22.0954230324284));
#18742=CARTESIAN_POINT('',(-9.51647200958291,-1.63787847398016E-6,22.1545769675715));
#18743=CARTESIAN_POINT('',(-9.516475,1.78524650477582E-12,1.24542303242842));
#18744=CARTESIAN_POINT('Ctrl Pts',(-9.51589627264183,0.000889093519182621,
22.0954230324284));
#18745=CARTESIAN_POINT('Ctrl Pts',(-9.51392442065431,-0.241722873625218,
22.1068093522094));
#18746=CARTESIAN_POINT('Ctrl Pts',(-9.30556868281626,-0.826435388003987,
22.134103013142));
#18747=CARTESIAN_POINT('Ctrl Pts',(-8.3263597217982,-1.1900304846565,22.1773040152262));
#18748=CARTESIAN_POINT('Ctrl Pts',(-7.56086357421315,-0.61293859637056,
22.2170723681052));
#18749=CARTESIAN_POINT('Ctrl Pts',(-7.44608444309555,0.076596244772818,
22.2488870504085));
#18750=CARTESIAN_POINT('Ctrl Pts',(-7.65935850290658,0.742288907720554,
22.2807017327117));
#18751=CARTESIAN_POINT('Ctrl Pts',(-8.50025311474624,1.20263187907136,22.3204700855908));
#18752=CARTESIAN_POINT('Ctrl Pts',(-9.36761503946097,0.728072660225888,
22.3613617423549));
#18753=CARTESIAN_POINT('Ctrl Pts',(-9.51436567791787,0.193492055931185,
22.3863460579675));
#18754=CARTESIAN_POINT('Ctrl Pts',(-9.51493538331909,-0.000390544144346583,
22.3954230324284));
#18755=CARTESIAN_POINT('Ctrl Pts',(-9.51576916465609,-0.000386592347592606,
22.1545769675715));
#18756=CARTESIAN_POINT('Ctrl Pts',(-9.51620747696863,-0.135644650959571,
22.1609140295152));
#18757=CARTESIAN_POINT('Ctrl Pts',(-9.42610449104091,-0.60977881496797,
22.1831584326104));
#18758=CARTESIAN_POINT('Ctrl Pts',(-8.7081020895998,-1.18449019452673,22.2213101768575));
#18759=CARTESIAN_POINT('Ctrl Pts',(-7.61521781807871,-0.814404432911052,
22.2690322003123));
#18760=CARTESIAN_POINT('Ctrl Pts',(-7.33719548426661,0.30316329774476,22.3167542237672));
#18761=CARTESIAN_POINT('Ctrl Pts',(-8.12547601519426,1.14272738419793,22.364476247222));
#18762=CARTESIAN_POINT('Ctrl Pts',(-9.21759447524406,0.939966962847629,
22.4104171618235));
#18763=CARTESIAN_POINT('Ctrl Pts',(-9.51469503156432,0.299302442536928,
22.4404507352733));
#18764=CARTESIAN_POINT('Ctrl Pts',(-9.51711756914169,-0.000632200503468537,
22.4545769675715));
#18765=CARTESIAN_POINT('Origin',(-8.5,0.,1.24542303242842));
#18766=CARTESIAN_POINT('',(-9.51691317747902,3.08906250382967E-5,21.7954230324284));
#18767=CARTESIAN_POINT('',(-9.516475,1.20656969512839E-12,21.8545769675715));
#18768=CARTESIAN_POINT('',(-9.516475,1.78524650477582E-12,1.24542303242842));
#18769=CARTESIAN_POINT('Ctrl Pts',(-9.51824203506389,0.000124572390490018,
21.7954230324284));
#18770=CARTESIAN_POINT('Ctrl Pts',(-9.51824208893095,-0.000615822241855329,
21.7954579641481));
#18771=CARTESIAN_POINT('Ctrl Pts',(-9.5178614904951,-0.338520706650099,
21.8114002370193));
#18772=CARTESIAN_POINT('Ctrl Pts',(-9.14729583240704,-1.01357368058483,
21.8432498510421));
#18773=CARTESIAN_POINT('Ctrl Pts',(-8.19080776710961,-1.07799402237706,
21.8830182039212));
#18774=CARTESIAN_POINT('Ctrl Pts',(-7.65285755162984,-0.63162857595897,
21.9148328862244));
#18775=CARTESIAN_POINT('Ctrl Pts',(-7.37859808588644,0.0113444340040694,
21.9466475685277));
#18776=CARTESIAN_POINT('Ctrl Pts',(-7.71333472266603,0.909659959579857,
21.9864159214067));
#18777=CARTESIAN_POINT('Ctrl Pts',(-8.84120404649836,1.15311486350827,22.0341379448616));
#18778=CARTESIAN_POINT('Ctrl Pts',(-9.45970169651922,0.531555192179094,
22.0704736485355));
#18779=CARTESIAN_POINT('Ctrl Pts',(-9.5166792108648,0.0972199457469021,
22.0909020110578));
#18780=CARTESIAN_POINT('Ctrl Pts',(-9.51589627264183,0.000889093519182621,
22.0954230324284));
#18781=CARTESIAN_POINT('Ctrl Pts',(-9.516475,1.20656969512839E-12,21.8545769675715));
#18782=CARTESIAN_POINT('Ctrl Pts',(-9.51647500000032,-0.265706620582781,
21.8670579008197));
#18783=CARTESIAN_POINT('Ctrl Pts',(-9.40727465387257,-0.529786878176101,
21.8795388340679));
#18784=CARTESIAN_POINT('Ctrl Pts',(-9.21961691907837,-0.717894780174059,
21.892019767316));
#18785=CARTESIAN_POINT('Ctrl Pts',(-9.03195918428417,-0.906002682172016,
21.9045007005642));
#18786=CARTESIAN_POINT('Ctrl Pts',(-8.76814132834463,-1.01583545019887,
21.9169816338124));
#18787=CARTESIAN_POINT('Ctrl Pts',(-8.50243547044586,-1.0164720823066,21.9294625670606));
#18788=CARTESIAN_POINT('Ctrl Pts',(-8.23672961254708,-1.01710871441432,
21.9419435003088));
#18789=CARTESIAN_POINT('Ctrl Pts',(-7.97238846933404,-0.908541417083162,
21.954424433557));
#18790=CARTESIAN_POINT('Ctrl Pts',(-7.78383148002393,-0.721334926799113,
21.9669053668052));
#18791=CARTESIAN_POINT('Ctrl Pts',(-7.59527449071382,-0.534128436515065,
21.9793863000534));
#18792=CARTESIAN_POINT('Ctrl Pts',(-7.48480993131722,-0.270574496756449,
21.9918672333016));
#18793=CARTESIAN_POINT('Ctrl Pts',(-7.48353667075686,-0.00487092690894227,
22.0043481665498));
#18794=CARTESIAN_POINT('Ctrl Pts',(-7.48226341019651,0.260832642938564,
22.016829099798));
#18795=CARTESIAN_POINT('Ctrl Pts',(-7.59019703546717,0.525433154239857,
22.0293100330461));
#18796=CARTESIAN_POINT('Ctrl Pts',(-7.77695120652474,0.714438148392827,
22.0417909662943));
#18797=CARTESIAN_POINT('Ctrl Pts',(-7.96370537758231,0.903443142545798,
22.0542718995425));
#18798=CARTESIAN_POINT('Ctrl Pts',(-8.2269938881477,1.01453885915644,22.0667528327907));
#18799=CARTESIAN_POINT('Ctrl Pts',(-8.49269364459102,1.01644874085988,22.0792337660389));
#18800=CARTESIAN_POINT('Ctrl Pts',(-8.75839340103435,1.01835862256332,22.0917146992871));
#18801=CARTESIAN_POINT('Ctrl Pts',(-9.02325176140342,0.911059288979255,
22.1041956325353));
#18802=CARTESIAN_POINT('Ctrl Pts',(-9.21270367535806,0.724758509267825,
22.1166765657835));
#18803=CARTESIAN_POINT('Ctrl Pts',(-9.4021555893127,0.538457729556394,22.1291574990317));
#18804=CARTESIAN_POINT('Ctrl Pts',(-9.51388182535831,0.275436159672753,
22.1416384322799));
#18805=CARTESIAN_POINT('Ctrl Pts',(-9.51642831724057,0.00974174196463319,
22.1541193655281));
#18806=CARTESIAN_POINT('Ctrl Pts',(-9.51645943884197,0.00649459406721488,
22.1542718995425));
#18807=CARTESIAN_POINT('Ctrl Pts',(-9.516475,0.00324729703447892,22.154424433557));
#18808=CARTESIAN_POINT('Ctrl Pts',(-9.516475,1.28626604170591E-12,22.1545769675715));
#18809=CARTESIAN_POINT('Origin',(-8.5,0.,1.24542303242842));
#18810=CARTESIAN_POINT('',(-9.516475,1.15770944915783E-12,21.4954230324284));
#18811=CARTESIAN_POINT('',(-9.516475,1.1846532627374E-12,21.5545769675715));
#18812=CARTESIAN_POINT('',(-9.516475,1.78524650477582E-12,1.24542303242842));
#18813=CARTESIAN_POINT('Ctrl Pts',(-9.516475,1.21548936334437E-12,21.4954230324284));
#18814=CARTESIAN_POINT('Ctrl Pts',(-9.51647500000032,-0.265706620582753,
21.5079039656766));
#18815=CARTESIAN_POINT('Ctrl Pts',(-9.40727465387259,-0.529786878176055,
21.5203848989248));
#18816=CARTESIAN_POINT('Ctrl Pts',(-9.21961691907841,-0.717894780174012,
21.532865832173));
#18817=CARTESIAN_POINT('Ctrl Pts',(-9.03195918428424,-0.906002682171968,
21.5453467654212));
#18818=CARTESIAN_POINT('Ctrl Pts',(-8.76814132834473,-1.01583545019884,
21.5578276986694));
#18819=CARTESIAN_POINT('Ctrl Pts',(-8.50243547044598,-1.0164720823066,21.5703086319176));
#18820=CARTESIAN_POINT('Ctrl Pts',(-8.23672961254723,-1.01710871441435,
21.5827895651658));
#18821=CARTESIAN_POINT('Ctrl Pts',(-7.97238846933418,-0.908541417083243,
21.595270498414));
#18822=CARTESIAN_POINT('Ctrl Pts',(-7.78383148002406,-0.721334926799242,
21.6077514316622));
#18823=CARTESIAN_POINT('Ctrl Pts',(-7.59527449071393,-0.534128436515241,
21.6202323649103));
#18824=CARTESIAN_POINT('Ctrl Pts',(-7.48480993131728,-0.270574496756669,
21.6327132981585));
#18825=CARTESIAN_POINT('Ctrl Pts',(-7.48353667075686,-0.00487092690918231,
21.6451942314067));
#18826=CARTESIAN_POINT('Ctrl Pts',(-7.48226341019644,0.260832642938305,
21.6576751646549));
#18827=CARTESIAN_POINT('Ctrl Pts',(-7.59019703546703,0.525433154239604,
21.6701560979031));
#18828=CARTESIAN_POINT('Ctrl Pts',(-7.77695120652453,0.714438148392616,
21.6826370311513));
#18829=CARTESIAN_POINT('Ctrl Pts',(-7.96370537758203,0.903443142545627,
21.6951179643995));
#18830=CARTESIAN_POINT('Ctrl Pts',(-8.22699388814736,1.01453885915635,21.7075988976477));
#18831=CARTESIAN_POINT('Ctrl Pts',(-8.49269364459067,1.01644874085988,21.7200798308959));
#18832=CARTESIAN_POINT('Ctrl Pts',(-8.75839340103397,1.01835862256341,21.7325607641441));
#18833=CARTESIAN_POINT('Ctrl Pts',(-9.02325176140306,0.911059288979455,
21.7450416973922));
#18834=CARTESIAN_POINT('Ctrl Pts',(-9.21270367535776,0.724758509268115,
21.7575226306404));
#18835=CARTESIAN_POINT('Ctrl Pts',(-9.40215558931246,0.538457729556775,
21.7700035638886));
#18836=CARTESIAN_POINT('Ctrl Pts',(-9.51388182535818,0.275436159673204,
21.7824844971368));
#18837=CARTESIAN_POINT('Ctrl Pts',(-9.51642831724056,0.00974174196510433,
21.794965430385));
#18838=CARTESIAN_POINT('Ctrl Pts',(-9.51645943884196,0.00649459406749345,
21.7951179643995));
#18839=CARTESIAN_POINT('Ctrl Pts',(-9.516475,0.00324729703456478,21.795270498414));
#18840=CARTESIAN_POINT('Ctrl Pts',(-9.516475,1.17962588154882E-12,21.7954230324284));
#18841=CARTESIAN_POINT('Ctrl Pts',(-9.516475,1.24243317692394E-12,21.5545769675715));
#18842=CARTESIAN_POINT('Ctrl Pts',(-9.51647500000032,-0.265706620582746,
21.5670579008197));
#18843=CARTESIAN_POINT('Ctrl Pts',(-9.40727465387258,-0.529786878176069,
21.5795388340678));
#18844=CARTESIAN_POINT('Ctrl Pts',(-9.21961691907839,-0.717894780174033,
21.592019767316));
#18845=CARTESIAN_POINT('Ctrl Pts',(-9.0319591842842,-0.906002682171997,
21.6045007005642));
#18846=CARTESIAN_POINT('Ctrl Pts',(-8.76814132834467,-1.01583545019886,
21.6169816338124));
#18847=CARTESIAN_POINT('Ctrl Pts',(-8.50243547044589,-1.0164720823066,21.6294625670606));
#18848=CARTESIAN_POINT('Ctrl Pts',(-8.23672961254712,-1.01710871441433,
21.6419435003088));
#18849=CARTESIAN_POINT('Ctrl Pts',(-7.97238846933407,-0.908541417083181,
21.654424433557));
#18850=CARTESIAN_POINT('Ctrl Pts',(-7.78383148002395,-0.721334926799139,
21.6669053668052));
#18851=CARTESIAN_POINT('Ctrl Pts',(-7.59527449071384,-0.534128436515097,
21.6793863000534));
#18852=CARTESIAN_POINT('Ctrl Pts',(-7.48480993131722,-0.270574496756485,
21.6918672333016));
#18853=CARTESIAN_POINT('Ctrl Pts',(-7.48353667075686,-0.00487092690897814,
21.7043481665498));
#18854=CARTESIAN_POINT('Ctrl Pts',(-7.4822634101965,0.260832642938528,21.716829099798));
#18855=CARTESIAN_POINT('Ctrl Pts',(-7.59019703546716,0.525433154239825,
21.7293100330461));
#18856=CARTESIAN_POINT('Ctrl Pts',(-7.77695120652472,0.714438148392802,
21.7417909662943));
#18857=CARTESIAN_POINT('Ctrl Pts',(-7.96370537758228,0.903443142545779,
21.7542718995425));
#18858=CARTESIAN_POINT('Ctrl Pts',(-8.22699388814766,1.01453885915643,21.7667528327907));
#18859=CARTESIAN_POINT('Ctrl Pts',(-8.49269364459099,1.01644874085988,21.7792337660389));
#18860=CARTESIAN_POINT('Ctrl Pts',(-8.75839340103431,1.01835862256333,21.7917146992871));
#18861=CARTESIAN_POINT('Ctrl Pts',(-9.02325176140338,0.911059288979274,
21.8041956325353));
#18862=CARTESIAN_POINT('Ctrl Pts',(-9.21270367535803,0.72475850926785,21.8166765657835));
#18863=CARTESIAN_POINT('Ctrl Pts',(-9.40215558931268,0.538457729556426,
21.8291574990317));
#18864=CARTESIAN_POINT('Ctrl Pts',(-9.5138818253583,0.275436159672789,21.8416384322799));
#18865=CARTESIAN_POINT('Ctrl Pts',(-9.51642831724057,0.00974174196466906,
21.8541193655281));
#18866=CARTESIAN_POINT('Ctrl Pts',(-9.51645943884196,0.00649459406721223,
21.8542718995425));
#18867=CARTESIAN_POINT('Ctrl Pts',(-9.516475,0.00324729703443765,21.854424433557));
#18868=CARTESIAN_POINT('Ctrl Pts',(-9.516475,1.20656969512839E-12,21.8545769675715));
#18869=CARTESIAN_POINT('Origin',(-8.5,0.,1.24542303242842));
#18870=CARTESIAN_POINT('',(-9.51616151751664,0.000104592831971277,21.1954230324285));
#18871=CARTESIAN_POINT('',(-9.516475,1.16273683034641E-12,21.2545769675715));
#18872=CARTESIAN_POINT('',(-9.516475,1.78524650477582E-12,1.24542303242842));
#18873=CARTESIAN_POINT('Ctrl Pts',(-9.516475,1.13579301676685E-12,21.1954230324284));
#18874=CARTESIAN_POINT('Ctrl Pts',(-9.5164750000003,-0.265706620582814,
21.2079039656766));
#18875=CARTESIAN_POINT('Ctrl Pts',(-9.40727465387256,-0.529786878176089,
21.2203848989248));
#18876=CARTESIAN_POINT('Ctrl Pts',(-9.2196169190784,-0.717894780174027,
21.232865832173));
#18877=CARTESIAN_POINT('Ctrl Pts',(-9.03195918428423,-0.906002682171965,
21.2453467654212));
#18878=CARTESIAN_POINT('Ctrl Pts',(-8.76814132834475,-1.01583545019883,
21.2578276986694));
#18879=CARTESIAN_POINT('Ctrl Pts',(-8.50243547044602,-1.0164720823066,21.2703086319176));
#18880=CARTESIAN_POINT('Ctrl Pts',(-8.23672961254728,-1.01710871441436,
21.2827895651658));
#18881=CARTESIAN_POINT('Ctrl Pts',(-7.97238846933425,-0.908541417083278,
21.295270498414));
#18882=CARTESIAN_POINT('Ctrl Pts',(-7.78383148002412,-0.721334926799308,
21.3077514316622));
#18883=CARTESIAN_POINT('Ctrl Pts',(-7.59527449071399,-0.534128436515337,
21.3202323649103));
#18884=CARTESIAN_POINT('Ctrl Pts',(-7.48480993131732,-0.270574496756801,
21.3327132981585));
#18885=CARTESIAN_POINT('Ctrl Pts',(-7.48353667075686,-0.00487092690933373,
21.3451942314067));
#18886=CARTESIAN_POINT('Ctrl Pts',(-7.48226341019641,0.260832642938134,
21.3576751646549));
#18887=CARTESIAN_POINT('Ctrl Pts',(-7.59019703546694,0.52543315423943,21.3701560979031));
#18888=CARTESIAN_POINT('Ctrl Pts',(-7.77695120652438,0.714438148392467,
21.3826370311513));
#18889=CARTESIAN_POINT('Ctrl Pts',(-7.96370537758183,0.903443142545503,
21.3951179643995));
#18890=CARTESIAN_POINT('Ctrl Pts',(-8.22699388814712,1.01453885915627,21.4075988976477));
#18891=CARTESIAN_POINT('Ctrl Pts',(-8.4926936445904,1.01644874085988,21.4200798308959));
#18892=CARTESIAN_POINT('Ctrl Pts',(-8.75839340103369,1.01835862256348,21.432560764144));
#18893=CARTESIAN_POINT('Ctrl Pts',(-9.02325176140278,0.911059288979609,
21.4450416973922));
#18894=CARTESIAN_POINT('Ctrl Pts',(-9.21270367535753,0.724758509268343,
21.4575226306404));
#18895=CARTESIAN_POINT('Ctrl Pts',(-9.40215558931228,0.538457729557076,
21.4700035638886));
#18896=CARTESIAN_POINT('Ctrl Pts',(-9.51388182535807,0.275436159673566,
21.4824844971368));
#18897=CARTESIAN_POINT('Ctrl Pts',(-9.51642831724056,0.00974174196548686,
21.494965430385));
#18898=CARTESIAN_POINT('Ctrl Pts',(-9.51645943884196,0.00649459406776043,
21.4951179643995));
#18899=CARTESIAN_POINT('Ctrl Pts',(-9.516475,0.00324729703471629,21.495270498414));
#18900=CARTESIAN_POINT('Ctrl Pts',(-9.516475,1.21548936334437E-12,21.4954230324284));
#18901=CARTESIAN_POINT('Ctrl Pts',(-9.516475,1.16273683034641E-12,21.2545769675715));
#18902=CARTESIAN_POINT('Ctrl Pts',(-9.5164750000003,-0.265706620582787,
21.2670579008197));
#18903=CARTESIAN_POINT('Ctrl Pts',(-9.40727465387258,-0.529786878176065,
21.2795388340678));
#18904=CARTESIAN_POINT('Ctrl Pts',(-9.21961691907842,-0.717894780174008,
21.292019767316));
#18905=CARTESIAN_POINT('Ctrl Pts',(-9.03195918428426,-0.906002682171951,
21.3045007005642));
#18906=CARTESIAN_POINT('Ctrl Pts',(-8.76814132834478,-1.01583545019882,
21.3169816338124));
#18907=CARTESIAN_POINT('Ctrl Pts',(-8.50243547044604,-1.0164720823066,21.3294625670606));
#18908=CARTESIAN_POINT('Ctrl Pts',(-8.23672961254731,-1.01710871441437,
21.3419435003088));
#18909=CARTESIAN_POINT('Ctrl Pts',(-7.97238846933428,-0.908541417083292,
21.354424433557));
#18910=CARTESIAN_POINT('Ctrl Pts',(-7.78383148002414,-0.721334926799327,
21.3669053668052));
#18911=CARTESIAN_POINT('Ctrl Pts',(-7.59527449071401,-0.534128436515362,
21.3793863000534));
#18912=CARTESIAN_POINT('Ctrl Pts',(-7.48480993131733,-0.270574496756828,
21.3918672333016));
#18913=CARTESIAN_POINT('Ctrl Pts',(-7.48353667075686,-0.00487092690936068,
21.4043481665497));
#18914=CARTESIAN_POINT('Ctrl Pts',(-7.4822634101964,0.260832642938107,21.4168290997979));
#18915=CARTESIAN_POINT('Ctrl Pts',(-7.59019703546693,0.525433154239406,
21.4293100330461));
#18916=CARTESIAN_POINT('Ctrl Pts',(-7.77695120652437,0.714438148392448,
21.4417909662943));
#18917=CARTESIAN_POINT('Ctrl Pts',(-7.96370537758181,0.903443142545489,
21.4542718995425));
#18918=CARTESIAN_POINT('Ctrl Pts',(-8.22699388814709,1.01453885915627,21.4667528327907));
#18919=CARTESIAN_POINT('Ctrl Pts',(-8.49269364459037,1.01644874085988,21.4792337660389));
#18920=CARTESIAN_POINT('Ctrl Pts',(-8.75839340103366,1.01835862256349,21.4917146992871));
#18921=CARTESIAN_POINT('Ctrl Pts',(-9.02325176140276,0.911059288979622,
21.5041956325353));
#18922=CARTESIAN_POINT('Ctrl Pts',(-9.21270367535751,0.724758509268361,
21.5166765657834));
#18923=CARTESIAN_POINT('Ctrl Pts',(-9.40215558931226,0.5384577295571,21.5291574990316));
#18924=CARTESIAN_POINT('Ctrl Pts',(-9.51388182535807,0.275436159673593,
21.5416384322798));
#18925=CARTESIAN_POINT('Ctrl Pts',(-9.51642831724056,0.0097417419655138,
21.554119365528));
#18926=CARTESIAN_POINT('Ctrl Pts',(-9.51645943884196,0.00649459406778737,
21.5542718995425));
#18927=CARTESIAN_POINT('Ctrl Pts',(-9.516475,0.00324729703474323,21.554424433557));
#18928=CARTESIAN_POINT('Ctrl Pts',(-9.516475,1.24243317692394E-12,21.5545769675715));
#18929=CARTESIAN_POINT('Origin',(-8.5,0.,1.24542303242842));
#18930=CARTESIAN_POINT('',(-9.51651008988031,1.86612749551999E-5,20.8954230324284));
#18931=CARTESIAN_POINT('',(-9.51611841008406,4.72824068350965E-5,20.9545769675715));
#18932=CARTESIAN_POINT('',(-9.516475,1.78524650477582E-12,1.24542303242842));
#18933=CARTESIAN_POINT('Ctrl Pts',(-9.51739547620554,0.00048952171884608,
20.8954230324284));
#18934=CARTESIAN_POINT('Ctrl Pts',(-9.51672440796061,-0.121639760734766,
20.9011721528431));
#18935=CARTESIAN_POINT('Ctrl Pts',(-9.46120098978118,-0.413472798869971,
20.9148749438335));
#18936=CARTESIAN_POINT('Ctrl Pts',(-9.0945383169396,-0.950891759797607,
20.9444850759755));
#18937=CARTESIAN_POINT('Ctrl Pts',(-8.1573862740094,-1.15279631131811,20.9842534288547));
#18938=CARTESIAN_POINT('Ctrl Pts',(-7.34469566859739,-0.333715435113531,
21.0319754523094));
#18939=CARTESIAN_POINT('Ctrl Pts',(-7.59486638697568,0.790414745233752,
21.0796974757644));
#18940=CARTESIAN_POINT('Ctrl Pts',(-8.67505328733558,1.18972704280586,21.1274194992192));
#18941=CARTESIAN_POINT('Ctrl Pts',(-9.41959580507824,0.627975166168469,
21.1659946847739));
#18942=CARTESIAN_POINT('Ctrl Pts',(-9.51539910100029,0.144896470838527,
21.188662529177));
#18943=CARTESIAN_POINT('Ctrl Pts',(-9.51472347206447,0.000584393945904427,
21.1954230324284));
#18944=CARTESIAN_POINT('Ctrl Pts',(-9.516475,1.19860031214197E-12,20.9545769675715));
#18945=CARTESIAN_POINT('Ctrl Pts',(-9.51647500000031,-0.26570662058277,
20.9670579008197));
#18946=CARTESIAN_POINT('Ctrl Pts',(-9.40727465387258,-0.529786878176071,
20.9795388340678));
#18947=CARTESIAN_POINT('Ctrl Pts',(-9.2196169190784,-0.717894780174024,
20.992019767316));
#18948=CARTESIAN_POINT('Ctrl Pts',(-9.03195918428422,-0.906002682171976,
21.0045007005642));
#18949=CARTESIAN_POINT('Ctrl Pts',(-8.76814132834472,-1.01583545019884,
21.0169816338124));
#18950=CARTESIAN_POINT('Ctrl Pts',(-8.50243547044597,-1.0164720823066,21.0294625670606));
#18951=CARTESIAN_POINT('Ctrl Pts',(-8.23672961254721,-1.01710871441435,
21.0419435003088));
#18952=CARTESIAN_POINT('Ctrl Pts',(-7.97238846933417,-0.908541417083234,
21.054424433557));
#18953=CARTESIAN_POINT('Ctrl Pts',(-7.78383148002405,-0.72133492679923,
21.0669053668052));
#18954=CARTESIAN_POINT('Ctrl Pts',(-7.59527449071392,-0.534128436515226,
21.0793863000534));
#18955=CARTESIAN_POINT('Ctrl Pts',(-7.48480993131727,-0.270574496756652,
21.0918672333016));
#18956=CARTESIAN_POINT('Ctrl Pts',(-7.48353667075686,-0.00487092690916542,
21.1043481665498));
#18957=CARTESIAN_POINT('Ctrl Pts',(-7.48226341019645,0.260832642938322,
21.1168290997979));
#18958=CARTESIAN_POINT('Ctrl Pts',(-7.59019703546704,0.525433154239619,
21.1293100330461));
#18959=CARTESIAN_POINT('Ctrl Pts',(-7.77695120652454,0.714438148392628,
21.1417909662943));
#18960=CARTESIAN_POINT('Ctrl Pts',(-7.96370537758204,0.903443142545636,
21.1542718995425));
#18961=CARTESIAN_POINT('Ctrl Pts',(-8.22699388814738,1.01453885915635,21.1667528327907));
#18962=CARTESIAN_POINT('Ctrl Pts',(-8.49269364459069,1.01644874085988,21.1792337660389));
#18963=CARTESIAN_POINT('Ctrl Pts',(-8.75839340103399,1.01835862256341,21.1917146992871));
#18964=CARTESIAN_POINT('Ctrl Pts',(-9.02325176140307,0.911059288979446,
21.2041956325353));
#18965=CARTESIAN_POINT('Ctrl Pts',(-9.21270367535777,0.724758509268103,
21.2166765657835));
#18966=CARTESIAN_POINT('Ctrl Pts',(-9.40215558931247,0.53845772955676,21.2291574990317));
#18967=CARTESIAN_POINT('Ctrl Pts',(-9.51388182535818,0.275436159673187,
21.2416384322798));
#18968=CARTESIAN_POINT('Ctrl Pts',(-9.51642831724056,0.00974174196508744,
21.254119365528));
#18969=CARTESIAN_POINT('Ctrl Pts',(-9.51645943884196,0.00649459406747656,
21.2542718995425));
#18970=CARTESIAN_POINT('Ctrl Pts',(-9.516475,0.0032472970345479,21.254424433557));
#18971=CARTESIAN_POINT('Ctrl Pts',(-9.516475,1.16273683034641E-12,21.2545769675715));
#18972=CARTESIAN_POINT('Origin',(-8.5,0.,1.24542303242842));
#18973=CARTESIAN_POINT('',(-9.51649357373598,-1.11249508487427E-5,20.5954230324284));
#18974=CARTESIAN_POINT('',(-9.51648479396161,1.50281475572388E-5,20.6545769675715));
#18975=CARTESIAN_POINT('',(-9.516475,1.78524650477582E-12,1.24542303242842));
#18976=CARTESIAN_POINT('Ctrl Pts',(-9.516475,1.09196015198488E-12,20.5954230324284));
#18977=CARTESIAN_POINT('Ctrl Pts',(-9.51647500000029,-0.265706620582857,
20.6079039656766));
#18978=CARTESIAN_POINT('Ctrl Pts',(-9.40727465387254,-0.529786878176128,
20.6203848989248));
#18979=CARTESIAN_POINT('Ctrl Pts',(-9.21961691907837,-0.717894780174058,
20.632865832173));
#18980=CARTESIAN_POINT('Ctrl Pts',(-9.0319591842842,-0.906002682171989,
20.6453467654212));
#18981=CARTESIAN_POINT('Ctrl Pts',(-8.76814132834471,-1.01583545019884,
20.6578276986694));
#18982=CARTESIAN_POINT('Ctrl Pts',(-8.50243547044597,-1.0164720823066,20.6703086319176));
#18983=CARTESIAN_POINT('Ctrl Pts',(-8.23672961254724,-1.01710871441435,
20.6827895651658));
#18984=CARTESIAN_POINT('Ctrl Pts',(-7.97238846933421,-0.908541417083255,
20.695270498414));
#18985=CARTESIAN_POINT('Ctrl Pts',(-7.78383148002409,-0.721334926799277,
20.7077514316622));
#18986=CARTESIAN_POINT('Ctrl Pts',(-7.59527449071397,-0.534128436515299,
20.7202323649103));
#18987=CARTESIAN_POINT('Ctrl Pts',(-7.48480993131731,-0.270574496756757,
20.7327132981585));
#18988=CARTESIAN_POINT('Ctrl Pts',(-7.48353667075686,-0.0048709269092899,
20.7451942314067));
#18989=CARTESIAN_POINT('Ctrl Pts',(-7.48226341019642,0.260832642938178,
20.7576751646549));
#18990=CARTESIAN_POINT('Ctrl Pts',(-7.59019703546696,0.525433154239469,
20.7701560979031));
#18991=CARTESIAN_POINT('Ctrl Pts',(-7.77695120652442,0.714438148392498,
20.7826370311513));
#18992=CARTESIAN_POINT('Ctrl Pts',(-7.96370537758187,0.903443142545526,
20.7951179643995));
#18993=CARTESIAN_POINT('Ctrl Pts',(-8.22699388814716,1.01453885915629,20.8075988976477));
#18994=CARTESIAN_POINT('Ctrl Pts',(-8.49269364459045,1.01644874085988,20.8200798308959));
#18995=CARTESIAN_POINT('Ctrl Pts',(-8.75839340103373,1.01835862256347,20.832560764144));
#18996=CARTESIAN_POINT('Ctrl Pts',(-9.02325176140282,0.911059288979586,
20.8450416973922));
#18997=CARTESIAN_POINT('Ctrl Pts',(-9.21270367535756,0.724758509268312,
20.8575226306404));
#18998=CARTESIAN_POINT('Ctrl Pts',(-9.4021555893123,0.538457729557038,20.8700035638886));
#18999=CARTESIAN_POINT('Ctrl Pts',(-9.51388182535809,0.275436159673522,
20.8824844971368));
#19000=CARTESIAN_POINT('Ctrl Pts',(-9.51642831724056,0.00974174196544303,
20.894965430385));
#19001=CARTESIAN_POINT('Ctrl Pts',(-9.51645943884196,0.0064945940677166,
20.8951179643995));
#19002=CARTESIAN_POINT('Ctrl Pts',(-9.516475,0.00324729703467245,20.895270498414));
#19003=CARTESIAN_POINT('Ctrl Pts',(-9.516475,1.1716564985624E-12,20.8954230324284));
#19004=CARTESIAN_POINT('Ctrl Pts',(-9.51701410602559,0.000827220438096611,
20.6545769675715));
#19005=CARTESIAN_POINT('Ctrl Pts',(-9.51459385883776,-0.279828092863163,
20.6677864538149));
#19006=CARTESIAN_POINT('Ctrl Pts',(-9.24863288659975,-0.902577123736639,
20.6969032812101));
#19007=CARTESIAN_POINT('Ctrl Pts',(-8.19147423515819,-1.16238347934517,
20.7419274497567));
#19008=CARTESIAN_POINT('Ctrl Pts',(-7.49695823929343,-0.501575692631794,
20.7816958026358));
#19009=CARTESIAN_POINT('Ctrl Pts',(-7.46174696796193,0.196559475127261,
20.813510484939));
#19010=CARTESIAN_POINT('Ctrl Pts',(-7.74971360013524,0.833511408043322,
20.8453251672423));
#19011=CARTESIAN_POINT('Ctrl Pts',(-8.63771535503727,1.19472088021124,20.8850935201213));
#19012=CARTESIAN_POINT('Ctrl Pts',(-9.40914956869547,0.649570193703102,
20.924162010423));
#19013=CARTESIAN_POINT('Ctrl Pts',(-9.5152987801174,0.155174474396472,20.947323159573));
#19014=CARTESIAN_POINT('Ctrl Pts',(-9.51490137801837,0.000208656021816286,
20.9545769675715));
#19015=CARTESIAN_POINT('Origin',(-8.5,0.,1.24542303242842));
#19016=CARTESIAN_POINT('',(-9.5159845430734,-0.000147844677967088,20.2954230324284));
#19017=CARTESIAN_POINT('',(-9.516475,1.09698753317346E-12,20.3545769675715));
#19018=CARTESIAN_POINT('',(-9.516475,1.78524650477582E-12,1.24542303242842));
#19019=CARTESIAN_POINT('Ctrl Pts',(-9.51467624341893,-0.000542222108652152,
20.2954230324284));
#19020=CARTESIAN_POINT('Ctrl Pts',(-9.51530366581787,-0.14800524278466,
20.3023303884478));
#19021=CARTESIAN_POINT('Ctrl Pts',(-9.4166164222524,-0.634321150812596,
20.3251450856188));
#19022=CARTESIAN_POINT('Ctrl Pts',(-8.66406834236317,-1.1912915968917,20.3638671239414));
#19023=CARTESIAN_POINT('Ctrl Pts',(-7.58761183909353,-0.782029520380867,
20.4115891473963));
#19024=CARTESIAN_POINT('Ctrl Pts',(-7.34782400761312,0.344361107498901,
20.4593111708512));
#19025=CARTESIAN_POINT('Ctrl Pts',(-8.16803759563199,1.15590850101208,20.507033194306));
#19026=CARTESIAN_POINT('Ctrl Pts',(-9.10328679193923,0.945365535563934,
20.546801547185));
#19027=CARTESIAN_POINT('Ctrl Pts',(-9.46318133559031,0.407268310575454,
20.5762648265592));
#19028=CARTESIAN_POINT('Ctrl Pts',(-9.51665800623787,0.118514397257793,
20.5898207647817));
#19029=CARTESIAN_POINT('Ctrl Pts',(-9.51733834450537,-0.00051711008067569,
20.5954230324284));
#19030=CARTESIAN_POINT('Ctrl Pts',(-9.516475,1.15476744736E-12,20.3545769675715));
#19031=CARTESIAN_POINT('Ctrl Pts',(-9.5164750000003,-0.265706620582833,
20.3670579008197));
#19032=CARTESIAN_POINT('Ctrl Pts',(-9.40727465387254,-0.529786878176147,
20.3795388340679));
#19033=CARTESIAN_POINT('Ctrl Pts',(-9.21961691907833,-0.717894780174095,
20.392019767316));
#19034=CARTESIAN_POINT('Ctrl Pts',(-9.03195918428412,-0.906002682172043,
20.4045007005642));
#19035=CARTESIAN_POINT('Ctrl Pts',(-8.76814132834458,-1.01583545019888,
20.4169816338124));
#19036=CARTESIAN_POINT('Ctrl Pts',(-8.50243547044581,-1.0164720823066,20.4294625670606));
#19037=CARTESIAN_POINT('Ctrl Pts',(-8.23672961254703,-1.01710871441431,
20.4419435003088));
#19038=CARTESIAN_POINT('Ctrl Pts',(-7.97238846933399,-0.908541417083135,
20.454424433557));
#19039=CARTESIAN_POINT('Ctrl Pts',(-7.78383148002389,-0.721334926799077,
20.4669053668052));
#19040=CARTESIAN_POINT('Ctrl Pts',(-7.59527449071379,-0.534128436515019,
20.4793863000534));
#19041=CARTESIAN_POINT('Ctrl Pts',(-7.4848099313172,-0.270574496756397,
20.4918672333016));
#19042=CARTESIAN_POINT('Ctrl Pts',(-7.48353667075686,-0.00487092690889047,
20.5043481665498));
#19043=CARTESIAN_POINT('Ctrl Pts',(-7.48226341019652,0.260832642938616,
20.516829099798));
#19044=CARTESIAN_POINT('Ctrl Pts',(-7.5901970354672,0.525433154239903,20.5293100330461));
#19045=CARTESIAN_POINT('Ctrl Pts',(-7.77695120652478,0.714438148392864,
20.5417909662943));
#19046=CARTESIAN_POINT('Ctrl Pts',(-7.96370537758235,0.903443142545826,
20.5542718995425));
#19047=CARTESIAN_POINT('Ctrl Pts',(-8.22699388814775,1.01453885915645,20.5667528327907));
#19048=CARTESIAN_POINT('Ctrl Pts',(-8.49269364459108,1.01644874085988,20.5792337660389));
#19049=CARTESIAN_POINT('Ctrl Pts',(-8.7583934010344,1.01835862256331,20.5917146992871));
#19050=CARTESIAN_POINT('Ctrl Pts',(-9.02325176140346,0.911059288979229,
20.6041956325353));
#19051=CARTESIAN_POINT('Ctrl Pts',(-9.21270367535809,0.724758509267789,
20.6166765657835));
#19052=CARTESIAN_POINT('Ctrl Pts',(-9.40215558931272,0.538457729556348,
20.6291574990317));
#19053=CARTESIAN_POINT('Ctrl Pts',(-9.51388182535832,0.275436159672701,
20.6416384322799));
#19054=CARTESIAN_POINT('Ctrl Pts',(-9.51642831724057,0.0097417419645814,
20.6541193655281));
#19055=CARTESIAN_POINT('Ctrl Pts',(-9.51645943884197,0.00649459406712457,
20.6542718995425));
#19056=CARTESIAN_POINT('Ctrl Pts',(-9.516475,0.00324729703434999,20.654424433557));
#19057=CARTESIAN_POINT('Ctrl Pts',(-9.516475,1.11890396556444E-12,20.6545769675715));
#19058=CARTESIAN_POINT('Origin',(-8.5,0.,1.24542303242842));
#19059=CARTESIAN_POINT('',(-9.516475,1.04812728720291E-12,19.9954230324285));
#19060=CARTESIAN_POINT('',(-9.516475,1.07507110078247E-12,20.0545769675715));
#19061=CARTESIAN_POINT('',(-9.516475,1.78524650477582E-12,1.24542303242842));
#19062=CARTESIAN_POINT('Ctrl Pts',(-9.516475,1.04812728720291E-12,19.9954230324285));
#19063=CARTESIAN_POINT('Ctrl Pts',(-9.51647500000027,-0.26570662058294,
20.0079039656766));
#19064=CARTESIAN_POINT('Ctrl Pts',(-9.40727465387248,-0.529786878176243,
20.0203848989248));
#19065=CARTESIAN_POINT('Ctrl Pts',(-9.21961691907825,-0.717894780174171,
20.032865832173));
#19066=CARTESIAN_POINT('Ctrl Pts',(-9.03195918428402,-0.906002682172099,
20.0453467654212));
#19067=CARTESIAN_POINT('Ctrl Pts',(-8.76814132834447,-1.01583545019891,
20.0578276986694));
#19068=CARTESIAN_POINT('Ctrl Pts',(-8.5024354704457,-1.0164720823066,20.0703086319176));
#19069=CARTESIAN_POINT('Ctrl Pts',(-8.23672961254693,-1.01710871441428,
20.0827895651658));
#19070=CARTESIAN_POINT('Ctrl Pts',(-7.97238846933389,-0.90854141708308,
20.095270498414));
#19071=CARTESIAN_POINT('Ctrl Pts',(-7.78383148002382,-0.721334926799002,
20.1077514316622));
#19072=CARTESIAN_POINT('Ctrl Pts',(-7.59527449071374,-0.534128436514924,
20.1202323649104));
#19073=CARTESIAN_POINT('Ctrl Pts',(-7.48480993131717,-0.270574496756291,
20.1327132981586));
#19074=CARTESIAN_POINT('Ctrl Pts',(-7.48353667075686,-0.00487092690878383,
20.1451942314067));
#19075=CARTESIAN_POINT('Ctrl Pts',(-7.48226341019655,0.260832642938723,
20.1576751646549));
#19076=CARTESIAN_POINT('Ctrl Pts',(-7.59019703546726,0.525433154239998,
20.1701560979031));
#19077=CARTESIAN_POINT('Ctrl Pts',(-7.77695120652485,0.71443814839294,20.1826370311513));
#19078=CARTESIAN_POINT('Ctrl Pts',(-7.96370537758245,0.903443142545882,
20.1951179643995));
#19079=CARTESIAN_POINT('Ctrl Pts',(-8.22699388814786,1.01453885915648,20.2075988976477));
#19080=CARTESIAN_POINT('Ctrl Pts',(-8.49269364459118,1.01644874085988,20.2200798308959));
#19081=CARTESIAN_POINT('Ctrl Pts',(-8.75839340103451,1.01835862256328,20.2325607641441));
#19082=CARTESIAN_POINT('Ctrl Pts',(-9.02325176140356,0.911059288979174,
20.2450416973923));
#19083=CARTESIAN_POINT('Ctrl Pts',(-9.21270367535817,0.724758509267714,
20.2575226306405));
#19084=CARTESIAN_POINT('Ctrl Pts',(-9.40215558931278,0.538457729556254,
20.2700035638887));
#19085=CARTESIAN_POINT('Ctrl Pts',(-9.51388182535835,0.275436159672595,
20.2824844971369));
#19086=CARTESIAN_POINT('Ctrl Pts',(-9.51642831724057,0.00974174196447476,
20.294965430385));
#19087=CARTESIAN_POINT('Ctrl Pts',(-9.51645943884197,0.00649459406705645,
20.2951179643995));
#19088=CARTESIAN_POINT('Ctrl Pts',(-9.516475,0.00324729703432047,20.295270498414));
#19089=CARTESIAN_POINT('Ctrl Pts',(-9.516475,1.12782363378043E-12,20.2954230324284));
#19090=CARTESIAN_POINT('Ctrl Pts',(-9.516475,1.07507110078247E-12,20.0545769675715));
#19091=CARTESIAN_POINT('Ctrl Pts',(-9.51647500000028,-0.265706620582874,
20.0670579008197));
#19092=CARTESIAN_POINT('Ctrl Pts',(-9.40727465387253,-0.529786878176143,
20.0795388340679));
#19093=CARTESIAN_POINT('Ctrl Pts',(-9.21961691907836,-0.71789478017407,
20.092019767316));
#19094=CARTESIAN_POINT('Ctrl Pts',(-9.03195918428418,-0.906002682171997,
20.1045007005642));
#19095=CARTESIAN_POINT('Ctrl Pts',(-8.76814132834469,-1.01583545019884,
20.1169816338124));
#19096=CARTESIAN_POINT('Ctrl Pts',(-8.50243547044596,-1.0164720823066,20.1294625670606));
#19097=CARTESIAN_POINT('Ctrl Pts',(-8.23672961254722,-1.01710871441435,
20.1419435003088));
#19098=CARTESIAN_POINT('Ctrl Pts',(-7.9723884693342,-0.908541417083247,
20.154424433557));
#19099=CARTESIAN_POINT('Ctrl Pts',(-7.78383148002408,-0.721334926799265,
20.1669053668052));
#19100=CARTESIAN_POINT('Ctrl Pts',(-7.59527449071396,-0.534128436515283,
20.1793863000534));
#19101=CARTESIAN_POINT('Ctrl Pts',(-7.4848099313173,-0.270574496756741,
20.1918672333016));
#19102=CARTESIAN_POINT('Ctrl Pts',(-7.48353667075686,-0.00487092690927301,
20.2043481665497));
#19103=CARTESIAN_POINT('Ctrl Pts',(-7.48226341019642,0.260832642938195,
20.2168290997979));
#19104=CARTESIAN_POINT('Ctrl Pts',(-7.59019703546697,0.525433154239485,
20.2293100330461));
#19105=CARTESIAN_POINT('Ctrl Pts',(-7.77695120652443,0.71443814839251,20.2417909662943));
#19106=CARTESIAN_POINT('Ctrl Pts',(-7.96370537758188,0.903443142545535,
20.2542718995425));
#19107=CARTESIAN_POINT('Ctrl Pts',(-8.22699388814718,1.01453885915629,20.2667528327907));
#19108=CARTESIAN_POINT('Ctrl Pts',(-8.49269364459046,1.01644874085988,20.2792337660389));
#19109=CARTESIAN_POINT('Ctrl Pts',(-8.75839340103375,1.01835862256346,20.2917146992871));
#19110=CARTESIAN_POINT('Ctrl Pts',(-9.02325176140284,0.911059288979577,
20.3041956325353));
#19111=CARTESIAN_POINT('Ctrl Pts',(-9.21270367535757,0.7247585092683,20.3166765657835));
#19112=CARTESIAN_POINT('Ctrl Pts',(-9.40215558931231,0.538457729557023,
20.3291574990316));
#19113=CARTESIAN_POINT('Ctrl Pts',(-9.51388182535809,0.275436159673506,
20.3416384322798));
#19114=CARTESIAN_POINT('Ctrl Pts',(-9.51642831724056,0.00974174196542614,
20.354119365528));
#19115=CARTESIAN_POINT('Ctrl Pts',(-9.51645943884196,0.00649459406769971,
20.3542718995425));
#19116=CARTESIAN_POINT('Ctrl Pts',(-9.516475,0.00324729703465556,20.354424433557));
#19117=CARTESIAN_POINT('Ctrl Pts',(-9.516475,1.15476744736E-12,20.3545769675715));
#19118=CARTESIAN_POINT('Origin',(-8.5,0.,1.24542303242842));
#19119=CARTESIAN_POINT('',(-9.51688744271748,-4.25820637274689E-5,19.6954230324284));
#19120=CARTESIAN_POINT('',(-9.516475,1.05315466839149E-12,19.7545769675715));
#19121=CARTESIAN_POINT('',(-9.516475,1.78524650477582E-12,1.24542303242842));
#19122=CARTESIAN_POINT('Ctrl Pts',(-9.516475,1.02621085481192E-12,19.6954230324285));
#19123=CARTESIAN_POINT('Ctrl Pts',(-9.51647500000027,-0.265706620582943,
19.7079039656766));
#19124=CARTESIAN_POINT('Ctrl Pts',(-9.40727465387249,-0.529786878176224,
19.7203848989248));
#19125=CARTESIAN_POINT('Ctrl Pts',(-9.21961691907828,-0.717894780174146,
19.732865832173));
#19126=CARTESIAN_POINT('Ctrl Pts',(-9.03195918428407,-0.906002682172067,
19.7453467654212));
#19127=CARTESIAN_POINT('Ctrl Pts',(-8.76814132834455,-1.01583545019889,
19.7578276986694));
#19128=CARTESIAN_POINT('Ctrl Pts',(-8.50243547044579,-1.0164720823066,19.7703086319176));
#19129=CARTESIAN_POINT('Ctrl Pts',(-8.23672961254704,-1.01710871441431,
19.7827895651658));
#19130=CARTESIAN_POINT('Ctrl Pts',(-7.97238846933401,-0.908541417083145,
19.795270498414));
#19131=CARTESIAN_POINT('Ctrl Pts',(-7.78383148002392,-0.721334926799108,
19.8077514316622));
#19132=CARTESIAN_POINT('Ctrl Pts',(-7.59527449071383,-0.534128436515072,
19.8202323649104));
#19133=CARTESIAN_POINT('Ctrl Pts',(-7.48480993131723,-0.27057449675648,
19.8327132981585));
#19134=CARTESIAN_POINT('Ctrl Pts',(-7.48353667075686,-0.00487092690899303,
19.8451942314067));
#19135=CARTESIAN_POINT('Ctrl Pts',(-7.48226341019649,0.260832642938494,
19.8576751646549));
#19136=CARTESIAN_POINT('Ctrl Pts',(-7.59019703546713,0.525433154239773,
19.8701560979031));
#19137=CARTESIAN_POINT('Ctrl Pts',(-7.77695120652466,0.71443814839275,19.8826370311513));
#19138=CARTESIAN_POINT('Ctrl Pts',(-7.9637053775822,0.903443142545727,19.8951179643995));
#19139=CARTESIAN_POINT('Ctrl Pts',(-8.22699388814755,1.0145388591564,19.9075988976477));
#19140=CARTESIAN_POINT('Ctrl Pts',(-8.49269364459086,1.01644874085988,19.9200798308959));
#19141=CARTESIAN_POINT('Ctrl Pts',(-8.75839340103416,1.01835862256336,19.9325607641441));
#19142=CARTESIAN_POINT('Ctrl Pts',(-9.02325176140323,0.911059288979357,
19.9450416973923));
#19143=CARTESIAN_POINT('Ctrl Pts',(-9.2127036753579,0.724758509267982,19.9575226306405));
#19144=CARTESIAN_POINT('Ctrl Pts',(-9.40215558931256,0.538457729556607,
19.9700035638886));
#19145=CARTESIAN_POINT('Ctrl Pts',(-9.51388182535823,0.275436159673015,
19.9824844971368));
#19146=CARTESIAN_POINT('Ctrl Pts',(-9.51642831724057,0.00974174196491506,
19.994965430385));
#19147=CARTESIAN_POINT('Ctrl Pts',(-9.51645943884196,0.00649459406732343,
19.9951179643995));
#19148=CARTESIAN_POINT('Ctrl Pts',(-9.516475,0.00324729703441407,19.995270498414));
#19149=CARTESIAN_POINT('Ctrl Pts',(-9.516475,1.04812728720291E-12,19.9954230324285));
#19150=CARTESIAN_POINT('Ctrl Pts',(-9.516475,1.11093458257803E-12,19.7545769675715));
#19151=CARTESIAN_POINT('Ctrl Pts',(-9.51647500000029,-0.265706620582858,
19.7670579008197));
#19152=CARTESIAN_POINT('Ctrl Pts',(-9.40727465387253,-0.529786878176149,
19.7795388340678));
#19153=CARTESIAN_POINT('Ctrl Pts',(-9.21961691907834,-0.717894780174086,
19.792019767316));
#19154=CARTESIAN_POINT('Ctrl Pts',(-9.03195918428415,-0.906002682172022,
19.8045007005642));
#19155=CARTESIAN_POINT('Ctrl Pts',(-8.76814132834463,-1.01583545019886,
19.8169816338124));
#19156=CARTESIAN_POINT('Ctrl Pts',(-8.50243547044588,-1.0164720823066,19.8294625670606));
#19157=CARTESIAN_POINT('Ctrl Pts',(-8.23672961254712,-1.01710871441433,
19.8419435003088));
#19158=CARTESIAN_POINT('Ctrl Pts',(-7.97238846933409,-0.908541417083189,
19.854424433557));
#19159=CARTESIAN_POINT('Ctrl Pts',(-7.78383148002398,-0.721334926799168,
19.8669053668052));
#19160=CARTESIAN_POINT('Ctrl Pts',(-7.59527449071388,-0.534128436515148,
19.8793863000534));
#19161=CARTESIAN_POINT('Ctrl Pts',(-7.48480993131725,-0.270574496756565,
19.8918672333016));
#19162=CARTESIAN_POINT('Ctrl Pts',(-7.48353667075686,-0.00487092690907776,
19.9043481665498));
#19163=CARTESIAN_POINT('Ctrl Pts',(-7.48226341019647,0.260832642938409,
19.9168290997979));
#19164=CARTESIAN_POINT('Ctrl Pts',(-7.59019703546709,0.525433154239697,
19.9293100330461));
#19165=CARTESIAN_POINT('Ctrl Pts',(-7.7769512065246,0.71443814839269,19.9417909662943));
#19166=CARTESIAN_POINT('Ctrl Pts',(-7.96370537758212,0.903443142545683,
19.9542718995425));
#19167=CARTESIAN_POINT('Ctrl Pts',(-8.22699388814747,1.01453885915637,19.9667528327907));
#19168=CARTESIAN_POINT('Ctrl Pts',(-8.49269364459077,1.01644874085988,19.9792337660389));
#19169=CARTESIAN_POINT('Ctrl Pts',(-8.75839340103408,1.01835862256338,19.9917146992871));
#19170=CARTESIAN_POINT('Ctrl Pts',(-9.02325176140315,0.911059288979401,
20.0041956325353));
#19171=CARTESIAN_POINT('Ctrl Pts',(-9.21270367535783,0.724758509268041,
20.0166765657835));
#19172=CARTESIAN_POINT('Ctrl Pts',(-9.40215558931252,0.538457729556682,
20.0291574990317));
#19173=CARTESIAN_POINT('Ctrl Pts',(-9.51388182535821,0.2754361596731,20.0416384322798));
#19174=CARTESIAN_POINT('Ctrl Pts',(-9.51642831724057,0.00974174196499978,
20.054119365528));
#19175=CARTESIAN_POINT('Ctrl Pts',(-9.51645943884196,0.00649459406738889,
20.0542718995425));
#19176=CARTESIAN_POINT('Ctrl Pts',(-9.516475,0.00324729703446023,20.054424433557));
#19177=CARTESIAN_POINT('Ctrl Pts',(-9.516475,1.07507110078247E-12,20.0545769675715));
#19178=CARTESIAN_POINT('Origin',(-8.5,0.,1.24542303242842));
#19179=CARTESIAN_POINT('',(-9.51581279021529,-0.000874295316650707,19.3954230324285));
#19180=CARTESIAN_POINT('',(-9.516475,1.0312382360005E-12,19.4545769675715));
#19181=CARTESIAN_POINT('',(-9.516475,1.78524650477582E-12,1.24542303242842));
#19182=CARTESIAN_POINT('Ctrl Pts',(-9.51581279021529,-0.000874295316650814,
19.3954230324285));
#19183=CARTESIAN_POINT('Ctrl Pts',(-9.51660067785675,-0.100355318467702,
19.400090906567));
#19184=CARTESIAN_POINT('Ctrl Pts',(-9.45727900114472,-0.537898740061842,
19.4206661218572));
#19185=CARTESIAN_POINT('Ctrl Pts',(-8.83054984563462,-1.15621403266934,
19.457148678299));
#19186=CARTESIAN_POINT('Ctrl Pts',(-7.704974867994,-0.902362754165209,19.5048707017539));
#19187=CARTESIAN_POINT('Ctrl Pts',(-7.37854114860306,-0.000996887084833204,
19.5446390546329));
#19188=CARTESIAN_POINT('Ctrl Pts',(-7.65872158751808,0.639418187488004,
19.5764537369362));
#19189=CARTESIAN_POINT('Ctrl Pts',(-8.20076747273577,1.0808010195163,19.6082684192394));
#19190=CARTESIAN_POINT('Ctrl Pts',(-9.15393034110275,1.00776412933077,19.6479248510702));
#19191=CARTESIAN_POINT('Ctrl Pts',(-9.51797663774671,0.334619188771371,
19.6796276123251));
#19192=CARTESIAN_POINT('Ctrl Pts',(-9.51823730103989,-0.000181946276152444,
19.6954230324284));
#19193=CARTESIAN_POINT('Ctrl Pts',(-9.516475,1.0312382360005E-12,19.4545769675715));
#19194=CARTESIAN_POINT('Ctrl Pts',(-9.51647500000027,-0.265706620582918,
19.4670579008197));
#19195=CARTESIAN_POINT('Ctrl Pts',(-9.40727465387251,-0.529786878176182,
19.4795388340679));
#19196=CARTESIAN_POINT('Ctrl Pts',(-9.21961691907832,-0.717894780174101,
19.492019767316));
#19197=CARTESIAN_POINT('Ctrl Pts',(-9.03195918428414,-0.90600268217202,
19.5045007005642));
#19198=CARTESIAN_POINT('Ctrl Pts',(-8.76814132834465,-1.01583545019886,
19.5169816338124));
#19199=CARTESIAN_POINT('Ctrl Pts',(-8.50243547044591,-1.0164720823066,19.5294625670606));
#19200=CARTESIAN_POINT('Ctrl Pts',(-8.23672961254718,-1.01710871441434,
19.5419435003088));
#19201=CARTESIAN_POINT('Ctrl Pts',(-7.97238846933416,-0.908541417083224,
19.554424433557));
#19202=CARTESIAN_POINT('Ctrl Pts',(-7.78383148002405,-0.721334926799234,
19.5669053668052));
#19203=CARTESIAN_POINT('Ctrl Pts',(-7.59527449071394,-0.534128436515244,
19.5793863000534));
#19204=CARTESIAN_POINT('Ctrl Pts',(-7.48480993131729,-0.270574496756697,
19.5918672333016));
#19205=CARTESIAN_POINT('Ctrl Pts',(-7.48353667075686,-0.00487092690922918,
19.6043481665498));
#19206=CARTESIAN_POINT('Ctrl Pts',(-7.48226341019643,0.260832642938238,
19.6168290997979));
#19207=CARTESIAN_POINT('Ctrl Pts',(-7.59019703546699,0.525433154239524,
19.6293100330461));
#19208=CARTESIAN_POINT('Ctrl Pts',(-7.77695120652446,0.714438148392541,
19.6417909662943));
#19209=CARTESIAN_POINT('Ctrl Pts',(-7.96370537758192,0.903443142545558,
19.6542718995425));
#19210=CARTESIAN_POINT('Ctrl Pts',(-8.22699388814722,1.0145388591563,19.6667528327907));
#19211=CARTESIAN_POINT('Ctrl Pts',(-8.49269364459051,1.01644874085988,19.6792337660389));
#19212=CARTESIAN_POINT('Ctrl Pts',(-8.75839340103379,1.01835862256345,19.6917146992871));
#19213=CARTESIAN_POINT('Ctrl Pts',(-9.02325176140288,0.911059288979555,
19.7041956325353));
#19214=CARTESIAN_POINT('Ctrl Pts',(-9.2127036753576,0.724758509268269,19.7166765657835));
#19215=CARTESIAN_POINT('Ctrl Pts',(-9.40215558931233,0.538457729556984,
19.7291574990316));
#19216=CARTESIAN_POINT('Ctrl Pts',(-9.5138818253581,0.275436159673462,19.7416384322798));
#19217=CARTESIAN_POINT('Ctrl Pts',(-9.51642831724056,0.00974174196538231,
19.754119365528));
#19218=CARTESIAN_POINT('Ctrl Pts',(-9.51645943884196,0.00649459406765588,
19.7542718995425));
#19219=CARTESIAN_POINT('Ctrl Pts',(-9.516475,0.00324729703461173,19.754424433557));
#19220=CARTESIAN_POINT('Ctrl Pts',(-9.516475,1.11093458257803E-12,19.7545769675715));
#19221=CARTESIAN_POINT('Origin',(-8.5,0.,1.24542303242842));
#19222=CARTESIAN_POINT('',(-9.51601270277673,0.000133638117392702,19.0954230324284));
#19223=CARTESIAN_POINT('',(-9.516475,1.00932180360952E-12,19.1545769675715));
#19224=CARTESIAN_POINT('',(-9.516475,1.78524650477582E-12,1.24542303242842));
#19225=CARTESIAN_POINT('Ctrl Pts',(-9.51496883034704,0.000435394516211426,
19.0954230324284));
#19226=CARTESIAN_POINT('Ctrl Pts',(-9.51430705793103,-0.196566568372251,
19.1046468596573));
#19227=CARTESIAN_POINT('Ctrl Pts',(-9.36399077096857,-0.734371610655675,
19.1297780280378));
#19228=CARTESIAN_POINT('Ctrl Pts',(-8.48915653915779,-1.20258301999602,
19.1708165375699));
#19229=CARTESIAN_POINT('Ctrl Pts',(-7.65254526199483,-0.734500793868192,
19.2105848904489));
#19230=CARTESIAN_POINT('Ctrl Pts',(-7.44542256102972,-0.0668686100755817,
19.2423995727522));
#19231=CARTESIAN_POINT('Ctrl Pts',(-7.56655907558636,0.621577822794718,
19.2742142550554));
#19232=CARTESIAN_POINT('Ctrl Pts',(-8.33734740644836,1.19158198813036,19.3139826079345));
#19233=CARTESIAN_POINT('Ctrl Pts',(-9.3098427577801,0.820233931165877,19.3570367572507));
#19234=CARTESIAN_POINT('Ctrl Pts',(-9.51391568740291,0.238659514922684,
19.3841835654154));
#19235=CARTESIAN_POINT('Ctrl Pts',(-9.51581279021529,-0.000874295316650814,
19.3954230324285));
#19236=CARTESIAN_POINT('Ctrl Pts',(-9.516475,1.06710171779606E-12,19.1545769675715));
#19237=CARTESIAN_POINT('Ctrl Pts',(-9.51647500000028,-0.265706620582902,
19.1670579008197));
#19238=CARTESIAN_POINT('Ctrl Pts',(-9.40727465387251,-0.529786878176188,
19.1795388340679));
#19239=CARTESIAN_POINT('Ctrl Pts',(-9.21961691907831,-0.717894780174117,
19.192019767316));
#19240=CARTESIAN_POINT('Ctrl Pts',(-9.03195918428411,-0.906002682172045,
19.2045007005642));
#19241=CARTESIAN_POINT('Ctrl Pts',(-8.76814132834459,-1.01583545019888,
19.2169816338124));
#19242=CARTESIAN_POINT('Ctrl Pts',(-8.50243547044583,-1.0164720823066,19.2294625670606));
#19243=CARTESIAN_POINT('Ctrl Pts',(-8.23672961254708,-1.01710871441432,
19.2419435003088));
#19244=CARTESIAN_POINT('Ctrl Pts',(-7.97238846933405,-0.908541417083166,
19.254424433557));
#19245=CARTESIAN_POINT('Ctrl Pts',(-7.78383148002395,-0.721334926799137,
19.2669053668052));
#19246=CARTESIAN_POINT('Ctrl Pts',(-7.59527449071385,-0.534128436515108,
19.2793863000534));
#19247=CARTESIAN_POINT('Ctrl Pts',(-7.48480993131724,-0.270574496756521,
19.2918672333016));
#19248=CARTESIAN_POINT('Ctrl Pts',(-7.48353667075686,-0.00487092690903392,
19.3043481665498));
#19249=CARTESIAN_POINT('Ctrl Pts',(-7.48226341019648,0.260832642938453,
19.3168290997979));
#19250=CARTESIAN_POINT('Ctrl Pts',(-7.59019703546711,0.525433154239737,
19.3293100330461));
#19251=CARTESIAN_POINT('Ctrl Pts',(-7.77695120652464,0.714438148392721,
19.3417909662943));
#19252=CARTESIAN_POINT('Ctrl Pts',(-7.96370537758216,0.903443142545706,
19.3542718995425));
#19253=CARTESIAN_POINT('Ctrl Pts',(-8.22699388814751,1.01453885915638,19.3667528327907));
#19254=CARTESIAN_POINT('Ctrl Pts',(-8.49269364459082,1.01644874085988,19.3792337660389));
#19255=CARTESIAN_POINT('Ctrl Pts',(-8.75839340103412,1.01835862256337,19.3917146992871));
#19256=CARTESIAN_POINT('Ctrl Pts',(-9.02325176140319,0.911059288979378,
19.4041956325353));
#19257=CARTESIAN_POINT('Ctrl Pts',(-9.21270367535787,0.724758509268011,
19.4166765657835));
#19258=CARTESIAN_POINT('Ctrl Pts',(-9.40215558931254,0.538457729556643,
19.4291574990317));
#19259=CARTESIAN_POINT('Ctrl Pts',(-9.51388182535822,0.275436159673056,
19.4416384322799));
#19260=CARTESIAN_POINT('Ctrl Pts',(-9.51642831724057,0.00974174196495595,
19.454119365528));
#19261=CARTESIAN_POINT('Ctrl Pts',(-9.51645943884196,0.00649459406734506,
19.4542718995425));
#19262=CARTESIAN_POINT('Ctrl Pts',(-9.516475,0.0032472970344164,19.454424433557));
#19263=CARTESIAN_POINT('Ctrl Pts',(-9.516475,1.0312382360005E-12,19.4545769675715));
#19264=CARTESIAN_POINT('Origin',(-8.5,0.,1.24542303242842));
#19265=CARTESIAN_POINT('',(-9.516475,9.60461557638968E-13,18.7954230324285));
#19266=CARTESIAN_POINT('',(-9.516475,9.87405371218534E-13,18.8545769675715));
#19267=CARTESIAN_POINT('',(-9.516475,1.78524650477582E-12,1.24542303242842));
#19268=CARTESIAN_POINT('Ctrl Pts',(-9.516475,1.01824147182551E-12,18.7954230324285));
#19269=CARTESIAN_POINT('Ctrl Pts',(-9.51647500000027,-0.265706620582951,
18.8079039656766));
#19270=CARTESIAN_POINT('Ctrl Pts',(-9.40727465387248,-0.529786878176232,
18.8203848989248));
#19271=CARTESIAN_POINT('Ctrl Pts',(-9.21961691907827,-0.717894780174151,
18.832865832173));
#19272=CARTESIAN_POINT('Ctrl Pts',(-9.03195918428406,-0.906002682172071,
18.8453467654212));
#19273=CARTESIAN_POINT('Ctrl Pts',(-8.76814132834454,-1.01583545019889,
18.8578276986694));
#19274=CARTESIAN_POINT('Ctrl Pts',(-8.50243547044578,-1.0164720823066,18.8703086319176));
#19275=CARTESIAN_POINT('Ctrl Pts',(-8.23672961254703,-1.0171087144143,18.8827895651658));
#19276=CARTESIAN_POINT('Ctrl Pts',(-7.97238846933401,-0.908541417083141,
18.895270498414));
#19277=CARTESIAN_POINT('Ctrl Pts',(-7.78383148002392,-0.721334926799103,
18.9077514316622));
#19278=CARTESIAN_POINT('Ctrl Pts',(-7.59527449071383,-0.534128436515065,
18.9202323649104));
#19279=CARTESIAN_POINT('Ctrl Pts',(-7.48480993131723,-0.270574496756472,
18.9327132981585));
#19280=CARTESIAN_POINT('Ctrl Pts',(-7.48353667075686,-0.00487092690898506,
18.9451942314067));
#19281=CARTESIAN_POINT('Ctrl Pts',(-7.4822634101965,0.260832642938502,18.9576751646549));
#19282=CARTESIAN_POINT('Ctrl Pts',(-7.59019703546714,0.52543315423978,18.9701560979031));
#19283=CARTESIAN_POINT('Ctrl Pts',(-7.77695120652467,0.714438148392756,
18.9826370311513));
#19284=CARTESIAN_POINT('Ctrl Pts',(-7.9637053775822,0.903443142545731,18.9951179643995));
#19285=CARTESIAN_POINT('Ctrl Pts',(-8.22699388814756,1.0145388591564,19.0075988976477));
#19286=CARTESIAN_POINT('Ctrl Pts',(-8.49269364459087,1.01644874085988,19.0200798308959));
#19287=CARTESIAN_POINT('Ctrl Pts',(-8.75839340103417,1.01835862256336,19.0325607641441));
#19288=CARTESIAN_POINT('Ctrl Pts',(-9.02325176140323,0.911059288979353,
19.0450416973923));
#19289=CARTESIAN_POINT('Ctrl Pts',(-9.2127036753579,0.724758509267977,19.0575226306405));
#19290=CARTESIAN_POINT('Ctrl Pts',(-9.40215558931257,0.5384577295566,19.0700035638886));
#19291=CARTESIAN_POINT('Ctrl Pts',(-9.51388182535823,0.275436159673007,
19.0824844971368));
#19292=CARTESIAN_POINT('Ctrl Pts',(-9.51642831724057,0.00974174196490709,
19.094965430385));
#19293=CARTESIAN_POINT('Ctrl Pts',(-9.51645943884196,0.0064945940672962,
19.0951179643995));
#19294=CARTESIAN_POINT('Ctrl Pts',(-9.516475,0.00324729703436754,19.095270498414));
#19295=CARTESIAN_POINT('Ctrl Pts',(-9.516475,9.82377990029953E-13,19.0954230324285));
#19296=CARTESIAN_POINT('Ctrl Pts',(-9.516475,9.87405371218534E-13,18.8545769675715));
#19297=CARTESIAN_POINT('Ctrl Pts',(-9.51647500000026,-0.26570662058302,
18.8670579008197));
#19298=CARTESIAN_POINT('Ctrl Pts',(-9.40727465387243,-0.529786878176335,
18.8795388340679));
#19299=CARTESIAN_POINT('Ctrl Pts',(-9.21961691907817,-0.717894780174255,
18.8920197673161));
#19300=CARTESIAN_POINT('Ctrl Pts',(-9.03195918428391,-0.906002682172175,
18.9045007005642));
#19301=CARTESIAN_POINT('Ctrl Pts',(-8.76814132834432,-1.01583545019896,
18.9169816338124));
#19302=CARTESIAN_POINT('Ctrl Pts',(-8.50243547044552,-1.0164720823066,18.9294625670606));
#19303=CARTESIAN_POINT('Ctrl Pts',(-8.23672961254673,-1.01710871441424,
18.9419435003088));
#19304=CARTESIAN_POINT('Ctrl Pts',(-7.9723884693337,-0.908541417082972,
18.954424433557));
#19305=CARTESIAN_POINT('Ctrl Pts',(-7.78383148002365,-0.721334926798837,
18.9669053668052));
#19306=CARTESIAN_POINT('Ctrl Pts',(-7.5952744907136,-0.534128436514702,
18.9793863000534));
#19307=CARTESIAN_POINT('Ctrl Pts',(-7.48480993131709,-0.270574496756018,
18.9918672333016));
#19308=CARTESIAN_POINT('Ctrl Pts',(-7.48353667075686,-0.00487092690849199,
19.0043481665498));
#19309=CARTESIAN_POINT('Ctrl Pts',(-7.48226341019662,0.260832642939034,
19.016829099798));
#19310=CARTESIAN_POINT('Ctrl Pts',(-7.59019703546742,0.525433154240298,
19.0293100330462));
#19311=CARTESIAN_POINT('Ctrl Pts',(-7.7769512065251,0.714438148393189,19.0417909662944));
#19312=CARTESIAN_POINT('Ctrl Pts',(-7.96370537758277,0.90344314254608,19.0542718995426));
#19313=CARTESIAN_POINT('Ctrl Pts',(-8.22699388814824,1.01453885915659,19.0667528327907));
#19314=CARTESIAN_POINT('Ctrl Pts',(-8.49269364459159,1.01644874085989,19.0792337660389));
#19315=CARTESIAN_POINT('Ctrl Pts',(-8.75839340103493,1.01835862256318,19.0917146992871));
#19316=CARTESIAN_POINT('Ctrl Pts',(-9.02325176140396,0.911059288978948,
19.1041956325353));
#19317=CARTESIAN_POINT('Ctrl Pts',(-9.2127036753585,0.724758509267388,19.1166765657835));
#19318=CARTESIAN_POINT('Ctrl Pts',(-9.40215558931304,0.538457729555827,
19.1291574990317));
#19319=CARTESIAN_POINT('Ctrl Pts',(-9.51388182535849,0.275436159672093,
19.1416384322799));
#19320=CARTESIAN_POINT('Ctrl Pts',(-9.51642831724057,0.00974174196395182,
19.1541193655281));
#19321=CARTESIAN_POINT('Ctrl Pts',(-9.51645943884197,0.00649459406668756,
19.1542718995426));
#19322=CARTESIAN_POINT('Ctrl Pts',(-9.516475,0.00324729703410568,19.154424433557));
#19323=CARTESIAN_POINT('Ctrl Pts',(-9.516475,1.06710171779606E-12,19.1545769675715));
#19324=CARTESIAN_POINT('Origin',(-8.5,0.,1.24542303242842));
#19325=CARTESIAN_POINT('',(-9.516475,9.38545125247982E-13,18.4954230324285));
#19326=CARTESIAN_POINT('',(-9.516475,9.65488938827549E-13,18.5545769675715));
#19327=CARTESIAN_POINT('',(-9.516475,1.78524650477582E-12,1.24542303242842));
#19328=CARTESIAN_POINT('Ctrl Pts',(-9.516475,9.38545125247982E-13,18.4954230324285));
#19329=CARTESIAN_POINT('Ctrl Pts',(-9.51647500000024,-0.265706620583049,
18.5079039656766));
#19330=CARTESIAN_POINT('Ctrl Pts',(-9.40727465387243,-0.529786878176341,
18.5203848989248));
#19331=CARTESIAN_POINT('Ctrl Pts',(-9.21961691907818,-0.717894780174249,
18.532865832173));
#19332=CARTESIAN_POINT('Ctrl Pts',(-9.03195918428393,-0.906002682172157,
18.5453467654212));
#19333=CARTESIAN_POINT('Ctrl Pts',(-8.76814132834436,-1.01583545019894,
18.5578276986694));
#19334=CARTESIAN_POINT('Ctrl Pts',(-8.50243547044559,-1.0164720823066,18.5703086319176));
#19335=CARTESIAN_POINT('Ctrl Pts',(-8.23672961254682,-1.01710871441425,
18.5827895651658));
#19336=CARTESIAN_POINT('Ctrl Pts',(-7.9723884693338,-0.908541417083023,
18.595270498414));
#19337=CARTESIAN_POINT('Ctrl Pts',(-7.78383148002374,-0.721334926798925,
18.6077514316622));
#19338=CARTESIAN_POINT('Ctrl Pts',(-7.59527449071368,-0.534128436514826,
18.6202323649104));
#19339=CARTESIAN_POINT('Ctrl Pts',(-7.48480993131714,-0.270574496756181,
18.6327132981586));
#19340=CARTESIAN_POINT('Ctrl Pts',(-7.48353667075686,-0.00487092690867425,
18.6451942314068));
#19341=CARTESIAN_POINT('Ctrl Pts',(-7.48226341019657,0.260832642938833,
18.6576751646549));
#19342=CARTESIAN_POINT('Ctrl Pts',(-7.59019703546731,0.525433154240097,
18.6701560979031));
#19343=CARTESIAN_POINT('Ctrl Pts',(-7.77695120652493,0.714438148393018,
18.6826370311513));
#19344=CARTESIAN_POINT('Ctrl Pts',(-7.96370537758255,0.90344314254594,18.6951179643995));
#19345=CARTESIAN_POINT('Ctrl Pts',(-8.22699388814797,1.01453885915651,18.7075988976477));
#19346=CARTESIAN_POINT('Ctrl Pts',(-8.49269364459129,1.01644874085988,18.7200798308959));
#19347=CARTESIAN_POINT('Ctrl Pts',(-8.75839340103462,1.01835862256325,18.7325607641441));
#19348=CARTESIAN_POINT('Ctrl Pts',(-9.02325176140365,0.911059288979118,
18.7450416973923));
#19349=CARTESIAN_POINT('Ctrl Pts',(-9.21270367535825,0.724758509267637,
18.7575226306405));
#19350=CARTESIAN_POINT('Ctrl Pts',(-9.40215558931284,0.538457729556156,
18.7700035638887));
#19351=CARTESIAN_POINT('Ctrl Pts',(-9.51388182535838,0.275436159672486,
18.7824844971369));
#19352=CARTESIAN_POINT('Ctrl Pts',(-9.51642831724057,0.00974174196436518,
18.794965430385));
#19353=CARTESIAN_POINT('Ctrl Pts',(-9.51645943884197,0.00649459406694687,
18.7951179643995));
#19354=CARTESIAN_POINT('Ctrl Pts',(-9.516475,0.00324729703421089,18.795270498414));
#19355=CARTESIAN_POINT('Ctrl Pts',(-9.516475,1.01824147182551E-12,18.7954230324285));
#19356=CARTESIAN_POINT('Ctrl Pts',(-9.516475,9.65488938827549E-13,18.5545769675715));
#19357=CARTESIAN_POINT('Ctrl Pts',(-9.51647500000025,-0.265706620583022,
18.5670579008197));
#19358=CARTESIAN_POINT('Ctrl Pts',(-9.40727465387244,-0.529786878176317,
18.5795388340679));
#19359=CARTESIAN_POINT('Ctrl Pts',(-9.2196169190782,-0.717894780174229,
18.5920197673161));
#19360=CARTESIAN_POINT('Ctrl Pts',(-9.03195918428395,-0.906002682172142,
18.6045007005642));
#19361=CARTESIAN_POINT('Ctrl Pts',(-8.76814132834439,-1.01583545019893,
18.6169816338124));
#19362=CARTESIAN_POINT('Ctrl Pts',(-8.50243547044562,-1.0164720823066,18.6294625670606));
#19363=CARTESIAN_POINT('Ctrl Pts',(-8.23672961254684,-1.01710871441426,
18.6419435003088));
#19364=CARTESIAN_POINT('Ctrl Pts',(-7.97238846933382,-0.908541417083037,
18.654424433557));
#19365=CARTESIAN_POINT('Ctrl Pts',(-7.78383148002376,-0.721334926798944,
18.6669053668052));
#19366=CARTESIAN_POINT('Ctrl Pts',(-7.59527449071369,-0.53412843651485,
18.6793863000534));
#19367=CARTESIAN_POINT('Ctrl Pts',(-7.48480993131715,-0.270574496756208,
18.6918672333016));
#19368=CARTESIAN_POINT('Ctrl Pts',(-7.48353667075686,-0.0048709269087012,
18.7043481665498));
#19369=CARTESIAN_POINT('Ctrl Pts',(-7.48226341019657,0.260832642938806,
18.716829099798));
#19370=CARTESIAN_POINT('Ctrl Pts',(-7.5901970354673,0.525433154240073,18.7293100330462));
#19371=CARTESIAN_POINT('Ctrl Pts',(-7.77695120652491,0.714438148392999,
18.7417909662943));
#19372=CARTESIAN_POINT('Ctrl Pts',(-7.96370537758252,0.903443142545926,
18.7542718995425));
#19373=CARTESIAN_POINT('Ctrl Pts',(-8.22699388814794,1.01453885915651,18.7667528327907));
#19374=CARTESIAN_POINT('Ctrl Pts',(-8.49269364459126,1.01644874085988,18.7792337660389));
#19375=CARTESIAN_POINT('Ctrl Pts',(-8.75839340103459,1.01835862256326,18.7917146992871));
#19376=CARTESIAN_POINT('Ctrl Pts',(-9.02325176140363,0.911059288979131,
18.8041956325353));
#19377=CARTESIAN_POINT('Ctrl Pts',(-9.21270367535823,0.724758509267656,
18.8166765657835));
#19378=CARTESIAN_POINT('Ctrl Pts',(-9.40215558931282,0.53845772955618,18.8291574990317));
#19379=CARTESIAN_POINT('Ctrl Pts',(-9.51388182535837,0.275436159672513,
18.8416384322799));
#19380=CARTESIAN_POINT('Ctrl Pts',(-9.51642831724057,0.00974174196439213,
18.8541193655281));
#19381=CARTESIAN_POINT('Ctrl Pts',(-9.51645943884197,0.00649459406695455,
18.8542718995425));
#19382=CARTESIAN_POINT('Ctrl Pts',(-9.516475,0.00324729703419927,18.854424433557));
#19383=CARTESIAN_POINT('Ctrl Pts',(-9.516475,9.87405371218534E-13,18.8545769675715));
#19384=CARTESIAN_POINT('Origin',(-8.5,0.,1.24542303242842));
#19385=CARTESIAN_POINT('',(-9.516475,9.16628692856997E-13,18.1954230324285));
#19386=CARTESIAN_POINT('',(-9.516475,9.43572506436564E-13,18.2545769675715));
#19387=CARTESIAN_POINT('',(-9.516475,1.78524650477582E-12,1.24542303242842));
#19388=CARTESIAN_POINT('Ctrl Pts',(-9.516475,9.74408607043537E-13,18.1954230324285));
#19389=CARTESIAN_POINT('Ctrl Pts',(-9.51647500000025,-0.265706620583014,
18.2079039656766));
#19390=CARTESIAN_POINT('Ctrl Pts',(-9.40727465387245,-0.529786878176309,
18.2203848989248));
#19391=CARTESIAN_POINT('Ctrl Pts',(-9.2196169190782,-0.717894780174223,
18.232865832173));
#19392=CARTESIAN_POINT('Ctrl Pts',(-9.03195918428396,-0.906002682172138,
18.2453467654212));
#19393=CARTESIAN_POINT('Ctrl Pts',(-8.7681413283444,-1.01583545019893,18.2578276986694));
#19394=CARTESIAN_POINT('Ctrl Pts',(-8.50243547044563,-1.0164720823066,18.2703086319176));
#19395=CARTESIAN_POINT('Ctrl Pts',(-8.23672961254685,-1.01710871441426,
18.2827895651658));
#19396=CARTESIAN_POINT('Ctrl Pts',(-7.97238846933383,-0.908541417083041,
18.295270498414));
#19397=CARTESIAN_POINT('Ctrl Pts',(-7.78383148002376,-0.72133492679895,
18.3077514316622));
#19398=CARTESIAN_POINT('Ctrl Pts',(-7.5952744907137,-0.534128436514858,
18.3202323649104));
#19399=CARTESIAN_POINT('Ctrl Pts',(-7.48480993131715,-0.270574496756217,
18.3327132981586));
#19400=CARTESIAN_POINT('Ctrl Pts',(-7.48353667075686,-0.00487092690871011,
18.3451942314068));
#19401=CARTESIAN_POINT('Ctrl Pts',(-7.48226341019656,0.260832642938797,
18.3576751646549));
#19402=CARTESIAN_POINT('Ctrl Pts',(-7.59019703546729,0.525433154240064,
18.3701560979031));
#19403=CARTESIAN_POINT('Ctrl Pts',(-7.7769512065249,0.714438148392993,18.3826370311513));
#19404=CARTESIAN_POINT('Ctrl Pts',(-7.96370537758251,0.903443142545921,
18.3951179643995));
#19405=CARTESIAN_POINT('Ctrl Pts',(-8.22699388814793,1.0145388591565,18.4075988976477));
#19406=CARTESIAN_POINT('Ctrl Pts',(-8.49269364459126,1.01644874085988,18.4200798308959));
#19407=CARTESIAN_POINT('Ctrl Pts',(-8.75839340103458,1.01835862256326,18.4325607641441));
#19408=CARTESIAN_POINT('Ctrl Pts',(-9.02325176140362,0.911059288979136,
18.4450416973923));
#19409=CARTESIAN_POINT('Ctrl Pts',(-9.21270367535822,0.724758509267662,
18.4575226306405));
#19410=CARTESIAN_POINT('Ctrl Pts',(-9.40215558931282,0.538457729556188,
18.4700035638887));
#19411=CARTESIAN_POINT('Ctrl Pts',(-9.51388182535837,0.275436159672521,
18.4824844971369));
#19412=CARTESIAN_POINT('Ctrl Pts',(-9.51642831724057,0.00974174196440104,
18.494965430385));
#19413=CARTESIAN_POINT('Ctrl Pts',(-9.51645943884197,0.00649459406694421,
18.4951179643995));
#19414=CARTESIAN_POINT('Ctrl Pts',(-9.516475,0.00324729703416963,18.495270498414));
#19415=CARTESIAN_POINT('Ctrl Pts',(-9.516475,9.38545125247982E-13,18.4954230324285));
#19416=CARTESIAN_POINT('Ctrl Pts',(-9.516475,1.0013524206231E-12,18.2545769675715));
#19417=CARTESIAN_POINT('Ctrl Pts',(-9.51647500000026,-0.265706620582967,
18.2670579008197));
#19418=CARTESIAN_POINT('Ctrl Pts',(-9.40727465387248,-0.529786878176246,
18.2795388340679));
#19419=CARTESIAN_POINT('Ctrl Pts',(-9.21961691907826,-0.717894780174163,
18.292019767316));
#19420=CARTESIAN_POINT('Ctrl Pts',(-9.03195918428405,-0.90600268217208,
18.3045007005642));
#19421=CARTESIAN_POINT('Ctrl Pts',(-8.76814132834452,-1.01583545019889,
18.3169816338124));
#19422=CARTESIAN_POINT('Ctrl Pts',(-8.50243547044577,-1.0164720823066,18.3294625670606));
#19423=CARTESIAN_POINT('Ctrl Pts',(-8.23672961254701,-1.0171087144143,18.3419435003088));
#19424=CARTESIAN_POINT('Ctrl Pts',(-7.97238846933399,-0.908541417083132,
18.354424433557));
#19425=CARTESIAN_POINT('Ctrl Pts',(-7.78383148002391,-0.721334926799091,
18.3669053668052));
#19426=CARTESIAN_POINT('Ctrl Pts',(-7.59527449071382,-0.53412843651505,
18.3793863000534));
#19427=CARTESIAN_POINT('Ctrl Pts',(-7.48480993131722,-0.270574496756455,
18.3918672333016));
#19428=CARTESIAN_POINT('Ctrl Pts',(-7.48353667075686,-0.00487092690896818,
18.4043481665498));
#19429=CARTESIAN_POINT('Ctrl Pts',(-7.4822634101965,0.260832642938519,18.416829099798));
#19430=CARTESIAN_POINT('Ctrl Pts',(-7.59019703546714,0.525433154239796,
18.4293100330461));
#19431=CARTESIAN_POINT('Ctrl Pts',(-7.77695120652468,0.714438148392768,
18.4417909662943));
#19432=CARTESIAN_POINT('Ctrl Pts',(-7.96370537758222,0.90344314254574,18.4542718995425));
#19433=CARTESIAN_POINT('Ctrl Pts',(-8.22699388814758,1.0145388591564,18.4667528327907));
#19434=CARTESIAN_POINT('Ctrl Pts',(-8.49269364459088,1.01644874085988,18.4792337660389));
#19435=CARTESIAN_POINT('Ctrl Pts',(-8.75839340103419,1.01835862256336,18.4917146992871));
#19436=CARTESIAN_POINT('Ctrl Pts',(-9.02325176140325,0.911059288979345,
18.5041956325353));
#19437=CARTESIAN_POINT('Ctrl Pts',(-9.21270367535791,0.724758509267965,
18.5166765657835));
#19438=CARTESIAN_POINT('Ctrl Pts',(-9.40215558931258,0.538457729556585,
18.5291574990317));
#19439=CARTESIAN_POINT('Ctrl Pts',(-9.51388182535823,0.27543615967299,18.5416384322799));
#19440=CARTESIAN_POINT('Ctrl Pts',(-9.51642831724057,0.00974174196489021,
18.554119365528));
#19441=CARTESIAN_POINT('Ctrl Pts',(-9.51645943884196,0.00649459406727931,
18.5542718995425));
#19442=CARTESIAN_POINT('Ctrl Pts',(-9.516475,0.00324729703435065,18.554424433557));
#19443=CARTESIAN_POINT('Ctrl Pts',(-9.516475,9.65488938827549E-13,18.5545769675715));
#19444=CARTESIAN_POINT('Origin',(-8.5,0.,1.24542303242842));
#19445=CARTESIAN_POINT('',(-9.516475,8.94712260466012E-13,17.8954230324285));
#19446=CARTESIAN_POINT('',(-9.51621303022904,-8.85939138849132E-5,17.9545769675715));
#19447=CARTESIAN_POINT('',(-9.516475,1.78524650477582E-12,1.24542303242842));
#19448=CARTESIAN_POINT('Ctrl Pts',(-9.516475,9.52492174652552E-13,17.8954230324285));
#19449=CARTESIAN_POINT('Ctrl Pts',(-9.51647500000025,-0.265706620583055,
17.9079039656766));
#19450=CARTESIAN_POINT('Ctrl Pts',(-9.40727465387242,-0.529786878176366,
17.9203848989248));
#19451=CARTESIAN_POINT('Ctrl Pts',(-9.21961691907815,-0.71789478017428,
17.932865832173));
#19452=CARTESIAN_POINT('Ctrl Pts',(-9.03195918428387,-0.906002682172193,
17.9453467654212));
#19453=CARTESIAN_POINT('Ctrl Pts',(-8.76814132834428,-1.01583545019897,
17.9578276986694));
#19454=CARTESIAN_POINT('Ctrl Pts',(-8.50243547044549,-1.0164720823066,17.9703086319176));
#19455=CARTESIAN_POINT('Ctrl Pts',(-8.23672961254669,-1.01710871441423,
17.9827895651658));
#19456=CARTESIAN_POINT('Ctrl Pts',(-7.97238846933367,-0.908541417082954,
17.995270498414));
#19457=CARTESIAN_POINT('Ctrl Pts',(-7.78383148002362,-0.721334926798812,
18.0077514316622));
#19458=CARTESIAN_POINT('Ctrl Pts',(-7.59527449071358,-0.534128436514671,
18.0202323649104));
#19459=CARTESIAN_POINT('Ctrl Pts',(-7.48480993131709,-0.270574496755983,
18.0327132981586));
#19460=CARTESIAN_POINT('Ctrl Pts',(-7.48353667075686,-0.00487092690845708,
18.0451942314068));
#19461=CARTESIAN_POINT('Ctrl Pts',(-7.48226341019663,0.260832642939069,
18.057675164655));
#19462=CARTESIAN_POINT('Ctrl Pts',(-7.59019703546744,0.525433154240329,
18.0701560979031));
#19463=CARTESIAN_POINT('Ctrl Pts',(-7.77695120652512,0.714438148393214,
18.0826370311513));
#19464=CARTESIAN_POINT('Ctrl Pts',(-7.9637053775828,0.903443142546098,18.0951179643995));
#19465=CARTESIAN_POINT('Ctrl Pts',(-8.22699388814828,1.0145388591566,18.1075988976477));
#19466=CARTESIAN_POINT('Ctrl Pts',(-8.49269364459163,1.01644874085989,18.1200798308959));
#19467=CARTESIAN_POINT('Ctrl Pts',(-8.75839340103497,1.01835862256317,18.1325607641441));
#19468=CARTESIAN_POINT('Ctrl Pts',(-9.02325176140399,0.91105928897893,18.1450416973923));
#19469=CARTESIAN_POINT('Ctrl Pts',(-9.21270367535852,0.724758509267363,
18.1575226306405));
#19470=CARTESIAN_POINT('Ctrl Pts',(-9.40215558931306,0.538457729555796,
18.1700035638887));
#19471=CARTESIAN_POINT('Ctrl Pts',(-9.5138818253585,0.275436159672058,18.1824844971369));
#19472=CARTESIAN_POINT('Ctrl Pts',(-9.51642831724057,0.00974174196391691,
18.1949654303851));
#19473=CARTESIAN_POINT('Ctrl Pts',(-9.51645943884197,0.00649459406663339,
18.1951179643995));
#19474=CARTESIAN_POINT('Ctrl Pts',(-9.516475,0.0032472970340322,18.195270498414));
#19475=CARTESIAN_POINT('Ctrl Pts',(-9.516475,9.74408607043537E-13,18.1954230324285));
#19476=CARTESIAN_POINT('Ctrl Pts',(-9.516475,9.21656074045579E-13,17.9545769675715));
#19477=CARTESIAN_POINT('Ctrl Pts',(-9.51647500000024,-0.265706620583009,
17.9670579008197));
#19478=CARTESIAN_POINT('Ctrl Pts',(-9.40727465387247,-0.529786878176242,
17.9795388340679));
#19479=CARTESIAN_POINT('Ctrl Pts',(-9.21961691907829,-0.717894780174138,
17.992019767316));
#19480=CARTESIAN_POINT('Ctrl Pts',(-9.03195918428411,-0.906002682172034,
18.0045007005642));
#19481=CARTESIAN_POINT('Ctrl Pts',(-8.76814132834463,-1.01583545019885,
18.0169816338124));
#19482=CARTESIAN_POINT('Ctrl Pts',(-8.50243547044592,-1.0164720823066,18.0294625670606));
#19483=CARTESIAN_POINT('Ctrl Pts',(-8.2367296125472,-1.01710871441434,18.0419435003088));
#19484=CARTESIAN_POINT('Ctrl Pts',(-7.9723884693342,-0.908541417083243,
18.054424433557));
#19485=CARTESIAN_POINT('Ctrl Pts',(-7.7838314800241,-0.721334926799279,
18.0669053668052));
#19486=CARTESIAN_POINT('Ctrl Pts',(-7.59527449071399,-0.534128436515315,
18.0793863000534));
#19487=CARTESIAN_POINT('Ctrl Pts',(-7.48480993131732,-0.270574496756799,
18.0918672333016));
#19488=CARTESIAN_POINT('Ctrl Pts',(-7.48353667075686,-0.00487092690935071,
18.1043481665497));
#19489=CARTESIAN_POINT('Ctrl Pts',(-7.4822634101964,0.260832642938097,18.1168290997979));
#19490=CARTESIAN_POINT('Ctrl Pts',(-7.59019703546691,0.525433154239377,
18.1293100330461));
#19491=CARTESIAN_POINT('Ctrl Pts',(-7.77695120652433,0.714438148392414,
18.1417909662943));
#19492=CARTESIAN_POINT('Ctrl Pts',(-7.96370537758175,0.90344314254545,18.1542718995425));
#19493=CARTESIAN_POINT('Ctrl Pts',(-8.226993888147,1.01453885915624,18.1667528327907));
#19494=CARTESIAN_POINT('Ctrl Pts',(-8.49269364459027,1.01644874085988,18.1792337660389));
#19495=CARTESIAN_POINT('Ctrl Pts',(-8.75839340103353,1.01835862256351,18.1917146992871));
#19496=CARTESIAN_POINT('Ctrl Pts',(-9.02325176140262,0.911059288979693,
18.2041956325353));
#19497=CARTESIAN_POINT('Ctrl Pts',(-9.21270367535739,0.724758509268476,
18.2166765657834));
#19498=CARTESIAN_POINT('Ctrl Pts',(-9.40215558931216,0.538457729557259,
18.2291574990316));
#19499=CARTESIAN_POINT('Ctrl Pts',(-9.51388182535801,0.275436159673794,
18.2416384322798));
#19500=CARTESIAN_POINT('Ctrl Pts',(-9.51642831724056,0.00974174196573495,
18.254119365528));
#19501=CARTESIAN_POINT('Ctrl Pts',(-9.51645943884196,0.00649459406785445,
18.2542718995425));
#19502=CARTESIAN_POINT('Ctrl Pts',(-9.516475,0.00324729703465622,18.254424433557));
#19503=CARTESIAN_POINT('Ctrl Pts',(-9.516475,1.0013524206231E-12,18.2545769675715));
#19504=CARTESIAN_POINT('Origin',(-8.5,0.,1.24542303242842));
#19505=CARTESIAN_POINT('',(-9.516475,8.72795828075027E-13,17.5954230324285));
#19506=CARTESIAN_POINT('',(-9.51570671108984,0.000850778838430766,17.6545769675715));
#19507=CARTESIAN_POINT('',(-9.516475,1.78524650477582E-12,1.24542303242842));
#19508=CARTESIAN_POINT('Ctrl Pts',(-9.516475,9.30575742261567E-13,17.5954230324285));
#19509=CARTESIAN_POINT('Ctrl Pts',(-9.51647500000024,-0.265706620583019,
17.6079039656766));
#19510=CARTESIAN_POINT('Ctrl Pts',(-9.40727465387245,-0.529786878176272,
17.6203848989248));
#19511=CARTESIAN_POINT('Ctrl Pts',(-9.21961691907825,-0.717894780174172,
17.632865832173));
#19512=CARTESIAN_POINT('Ctrl Pts',(-9.03195918428405,-0.906002682172073,
17.6453467654212));
#19513=CARTESIAN_POINT('Ctrl Pts',(-8.76814132834455,-1.01583545019888,
17.6578276986694));
#19514=CARTESIAN_POINT('Ctrl Pts',(-8.50243547044581,-1.0164720823066,17.6703086319176));
#19515=CARTESIAN_POINT('Ctrl Pts',(-8.23672961254708,-1.01710871441431,
17.6827895651658));
#19516=CARTESIAN_POINT('Ctrl Pts',(-7.97238846933407,-0.908541417083172,
17.695270498414));
#19517=CARTESIAN_POINT('Ctrl Pts',(-7.78383148002398,-0.721334926799163,
17.7077514316622));
#19518=CARTESIAN_POINT('Ctrl Pts',(-7.59527449071389,-0.534128436515155,
17.7202323649103));
#19519=CARTESIAN_POINT('Ctrl Pts',(-7.48480993131726,-0.270574496756596,
17.7327132981585));
#19520=CARTESIAN_POINT('Ctrl Pts',(-7.48353667075686,-0.00487092690912852,
17.7451942314067));
#19521=CARTESIAN_POINT('Ctrl Pts',(-7.48226341019646,0.260832642938339,
17.7576751646549));
#19522=CARTESIAN_POINT('Ctrl Pts',(-7.59019703546705,0.525433154239614,
17.7701560979031));
#19523=CARTESIAN_POINT('Ctrl Pts',(-7.77695120652453,0.714438148392613,
17.7826370311513));
#19524=CARTESIAN_POINT('Ctrl Pts',(-7.96370537758201,0.903443142545612,
17.7951179643995));
#19525=CARTESIAN_POINT('Ctrl Pts',(-8.22699388814732,1.01453885915633,17.8075988976477));
#19526=CARTESIAN_POINT('Ctrl Pts',(-8.49269364459061,1.01644874085988,17.8200798308959));
#19527=CARTESIAN_POINT('Ctrl Pts',(-8.75839340103389,1.01835862256343,17.8325607641441));
#19528=CARTESIAN_POINT('Ctrl Pts',(-9.02325176140296,0.911059288979503,
17.8450416973922));
#19529=CARTESIAN_POINT('Ctrl Pts',(-9.21270367535767,0.724758509268199,
17.8575226306404));
#19530=CARTESIAN_POINT('Ctrl Pts',(-9.40215558931239,0.538457729556894,
17.8700035638886));
#19531=CARTESIAN_POINT('Ctrl Pts',(-9.51388182535813,0.275436159673361,
17.8824844971368));
#19532=CARTESIAN_POINT('Ctrl Pts',(-9.51642831724056,0.00974174196528165,
17.894965430385));
#19533=CARTESIAN_POINT('Ctrl Pts',(-9.51645943884196,0.00649459406753596,
17.8951179643995));
#19534=CARTESIAN_POINT('Ctrl Pts',(-9.516475,0.00324729703447251,17.895270498414));
#19535=CARTESIAN_POINT('Ctrl Pts',(-9.516475,9.52492174652552E-13,17.8954230324285));
#19536=CARTESIAN_POINT('Ctrl Pts',(-9.51570671108984,0.00085077883843071,
17.6545769675715));
#19537=CARTESIAN_POINT('Ctrl Pts',(-9.51391306809171,-0.234644624850221,
17.6656239612628));
#19538=CARTESIAN_POINT('Ctrl Pts',(-9.31537561793486,-0.812092956351842,
17.6925782961058));
#19539=CARTESIAN_POINT('Ctrl Pts',(-8.35176929286965,-1.19346183771808,
17.7354399721004));
#19540=CARTESIAN_POINT('Ctrl Pts',(-7.57414417389279,-0.632820621048115,
17.7752083249795));
#19541=CARTESIAN_POINT('Ctrl Pts',(-7.44469102409625,0.0541105458809273,
17.8070230072827));
#19542=CARTESIAN_POINT('Ctrl Pts',(-7.64372479594433,0.724198677214912,
17.8388376895859));
#19543=CARTESIAN_POINT('Ctrl Pts',(-8.47461430237912,1.20236394946876,17.878606042465));
#19544=CARTESIAN_POINT('Ctrl Pts',(-9.35917600400969,0.742620125736834,
17.9198370253188));
#19545=CARTESIAN_POINT('Ctrl Pts',(-9.51423527094977,0.200593991219319,
17.9451606670209));
#19546=CARTESIAN_POINT('Ctrl Pts',(-9.51501920748671,-0.000492325344205985,
17.9545769675715));
#19547=CARTESIAN_POINT('Origin',(-8.5,0.,1.24542303242842));
#19548=CARTESIAN_POINT('',(-9.516475,8.50879395684042E-13,17.2954230324285));
#19549=CARTESIAN_POINT('',(-9.51688182003018,5.98281162011358E-5,17.3545769675715));
#19550=CARTESIAN_POINT('',(-9.516475,1.78524650477582E-12,1.24542303242842));
#19551=CARTESIAN_POINT('Ctrl Pts',(-9.516475,8.50879395684042E-13,17.2954230324285));
#19552=CARTESIAN_POINT('Ctrl Pts',(-9.51647500000022,-0.265706620583098,
17.3079039656766));
#19553=CARTESIAN_POINT('Ctrl Pts',(-9.40727465387241,-0.529786878176343,
17.3203848989248));
#19554=CARTESIAN_POINT('Ctrl Pts',(-9.2196169190782,-0.717894780174229,
17.332865832173));
#19555=CARTESIAN_POINT('Ctrl Pts',(-9.03195918428398,-0.906002682172115,
17.3453467654212));
#19556=CARTESIAN_POINT('Ctrl Pts',(-8.76814132834447,-1.0158354501989,17.3578276986694));
#19557=CARTESIAN_POINT('Ctrl Pts',(-8.50243547044573,-1.0164720823066,17.3703086319176));
#19558=CARTESIAN_POINT('Ctrl Pts',(-8.236729612547,-1.01710871441429,17.3827895651658));
#19559=CARTESIAN_POINT('Ctrl Pts',(-7.972388469334,-0.90854141708313,17.395270498414));
#19560=CARTESIAN_POINT('Ctrl Pts',(-7.78383148002392,-0.721334926799107,
17.4077514316622));
#19561=CARTESIAN_POINT('Ctrl Pts',(-7.59527449071384,-0.534128436515084,
17.4202323649104));
#19562=CARTESIAN_POINT('Ctrl Pts',(-7.48480993131724,-0.270574496756517,
17.4327132981585));
#19563=CARTESIAN_POINT('Ctrl Pts',(-7.48353667075686,-0.00487092690904882,
17.4451942314067));
#19564=CARTESIAN_POINT('Ctrl Pts',(-7.48226341019648,0.260832642938419,
17.4576751646549));
#19565=CARTESIAN_POINT('Ctrl Pts',(-7.59019703546709,0.525433154239685,
17.4701560979031));
#19566=CARTESIAN_POINT('Ctrl Pts',(-7.77695120652458,0.71443814839267,17.4826370311513));
#19567=CARTESIAN_POINT('Ctrl Pts',(-7.96370537758208,0.903443142545654,
17.4951179643995));
#19568=CARTESIAN_POINT('Ctrl Pts',(-8.2269938881474,1.01453885915635,17.5075988976477));
#19569=CARTESIAN_POINT('Ctrl Pts',(-8.49269364459069,1.01644874085988,17.5200798308959));
#19570=CARTESIAN_POINT('Ctrl Pts',(-8.75839340103397,1.01835862256341,17.5325607641441));
#19571=CARTESIAN_POINT('Ctrl Pts',(-9.02325176140304,0.911059288979462,
17.5450416973923));
#19572=CARTESIAN_POINT('Ctrl Pts',(-9.21270367535773,0.724758509268143,
17.5575226306404));
#19573=CARTESIAN_POINT('Ctrl Pts',(-9.40215558931243,0.538457729556824,
17.5700035638886));
#19574=CARTESIAN_POINT('Ctrl Pts',(-9.51388182535815,0.275436159673282,
17.5824844971368));
#19575=CARTESIAN_POINT('Ctrl Pts',(-9.51642831724056,0.00974174196520196,
17.594965430385));
#19576=CARTESIAN_POINT('Ctrl Pts',(-9.51645943884196,0.00649459406747552,
17.5951179643995));
#19577=CARTESIAN_POINT('Ctrl Pts',(-9.516475,0.00324729703443137,17.595270498414));
#19578=CARTESIAN_POINT('Ctrl Pts',(-9.516475,9.30575742261567E-13,17.5954230324285));
#19579=CARTESIAN_POINT('Ctrl Pts',(-9.51821859738619,0.000256418416867737,
17.3545769675715));
#19580=CARTESIAN_POINT('Ctrl Pts',(-9.5176126438481,-0.330488117619876,
17.3701799143531));
#19581=CARTESIAN_POINT('Ctrl Pts',(-9.16144800526121,-1.00019275742554,
17.4016902022864));
#19582=CARTESIAN_POINT('Ctrl Pts',(-8.21385965450184,-1.08434065304146,
17.4411541607954));
#19583=CARTESIAN_POINT('Ctrl Pts',(-7.66651569284325,-0.649545145099307,
17.4729688430987));
#19584=CARTESIAN_POINT('Ctrl Pts',(-7.37861109970015,-0.0125651679117135,
17.5047835254019));
#19585=CARTESIAN_POINT('Ctrl Pts',(-7.69412058637172,0.892682402266311,
17.544551878281));
#19586=CARTESIAN_POINT('Ctrl Pts',(-8.81654339210534,1.16012687698589,17.5922739017358));
#19587=CARTESIAN_POINT('Ctrl Pts',(-9.45404978590041,0.546214074355226,
17.6289489314993));
#19588=CARTESIAN_POINT('Ctrl Pts',(-9.51649586046696,0.104461726685567,
17.6497166201112));
#19589=CARTESIAN_POINT('Ctrl Pts',(-9.51570671108984,0.00085077883843071,
17.6545769675715));
#19590=CARTESIAN_POINT('Origin',(-8.5,0.,1.24542303242842));
#19591=CARTESIAN_POINT('',(-9.516475,8.28962963293057E-13,16.9954230324285));
#19592=CARTESIAN_POINT('',(-9.516475,8.55906776872624E-13,17.0545769675715));
#19593=CARTESIAN_POINT('',(-9.516475,1.78524650477582E-12,1.24542303242842));
#19594=CARTESIAN_POINT('Ctrl Pts',(-9.516475,8.28962963293057E-13,16.9954230324285));
#19595=CARTESIAN_POINT('Ctrl Pts',(-9.51647500000022,-0.26570662058314,
17.0079039656767));
#19596=CARTESIAN_POINT('Ctrl Pts',(-9.40727465387238,-0.5297868781764,17.0203848989248));
#19597=CARTESIAN_POINT('Ctrl Pts',(-9.21961691907814,-0.717894780174285,
17.032865832173));
#19598=CARTESIAN_POINT('Ctrl Pts',(-9.0319591842839,-0.90600268217217,17.0453467654212));
#19599=CARTESIAN_POINT('Ctrl Pts',(-8.76814132834435,-1.01583545019894,
17.0578276986694));
#19600=CARTESIAN_POINT('Ctrl Pts',(-8.5024354704456,-1.0164720823066,17.0703086319176));
#19601=CARTESIAN_POINT('Ctrl Pts',(-8.23672961254684,-1.01710871441425,
17.0827895651658));
#19602=CARTESIAN_POINT('Ctrl Pts',(-7.97238846933384,-0.908541417083042,
17.095270498414));
#19603=CARTESIAN_POINT('Ctrl Pts',(-7.78383148002378,-0.721334926798969,
17.1077514316622));
#19604=CARTESIAN_POINT('Ctrl Pts',(-7.59527449071373,-0.534128436514896,
17.1202323649104));
#19605=CARTESIAN_POINT('Ctrl Pts',(-7.48480993131718,-0.270574496756283,
17.1327132981586));
#19606=CARTESIAN_POINT('Ctrl Pts',(-7.48353667075686,-0.00487092690879579,
17.1451942314067));
#19607=CARTESIAN_POINT('Ctrl Pts',(-7.48226341019654,0.260832642938692,
17.1576751646549));
#19608=CARTESIAN_POINT('Ctrl Pts',(-7.59019703546723,0.52543315423995,17.1701560979031));
#19609=CARTESIAN_POINT('Ctrl Pts',(-7.7769512065248,0.714438148392891,17.1826370311513));
#19610=CARTESIAN_POINT('Ctrl Pts',(-7.96370537758237,0.903443142545831,
17.1951179643995));
#19611=CARTESIAN_POINT('Ctrl Pts',(-8.22699388814775,1.01453885915645,17.2075988976477));
#19612=CARTESIAN_POINT('Ctrl Pts',(-8.49269364459106,1.01644874085988,17.2200798308959));
#19613=CARTESIAN_POINT('Ctrl Pts',(-8.75839340103436,1.01835862256331,17.2325607641441));
#19614=CARTESIAN_POINT('Ctrl Pts',(-9.0232517614034,0.911059288979256,17.2450416973923));
#19615=CARTESIAN_POINT('Ctrl Pts',(-9.21270367535804,0.724758509267844,
17.2575226306405));
#19616=CARTESIAN_POINT('Ctrl Pts',(-9.40215558931267,0.538457729556432,
17.2700035638887));
#19617=CARTESIAN_POINT('Ctrl Pts',(-9.51388182535828,0.275436159672818,
17.2824844971368));
#19618=CARTESIAN_POINT('Ctrl Pts',(-9.51642831724057,0.00974174196471782,
17.294965430385));
#19619=CARTESIAN_POINT('Ctrl Pts',(-9.51645943884197,0.00649459406712618,
17.2951179643995));
#19620=CARTESIAN_POINT('Ctrl Pts',(-9.516475,0.00324729703421682,17.295270498414));
#19621=CARTESIAN_POINT('Ctrl Pts',(-9.516475,8.50879395684042E-13,17.2954230324285));
#19622=CARTESIAN_POINT('Ctrl Pts',(-9.516475,9.13686691059164E-13,17.0545769675715));
#19623=CARTESIAN_POINT('Ctrl Pts',(-9.51647500000024,-0.265706620583055,
17.0670579008197));
#19624=CARTESIAN_POINT('Ctrl Pts',(-9.40727465387243,-0.529786878176325,
17.0795388340679));
#19625=CARTESIAN_POINT('Ctrl Pts',(-9.2196169190782,-0.717894780174225,
17.092019767316));
#19626=CARTESIAN_POINT('Ctrl Pts',(-9.03195918428397,-0.906002682172126,
17.1045007005642));
#19627=CARTESIAN_POINT('Ctrl Pts',(-8.76814132834443,-1.01583545019892,
17.1169816338124));
#19628=CARTESIAN_POINT('Ctrl Pts',(-8.50243547044568,-1.0164720823066,17.1294625670606));
#19629=CARTESIAN_POINT('Ctrl Pts',(-8.23672961254693,-1.01710871441428,
17.1419435003088));
#19630=CARTESIAN_POINT('Ctrl Pts',(-7.97238846933391,-0.908541417083087,
17.154424433557));
#19631=CARTESIAN_POINT('Ctrl Pts',(-7.78383148002384,-0.721334926799029,
17.1669053668052));
#19632=CARTESIAN_POINT('Ctrl Pts',(-7.59527449071377,-0.534128436514972,
17.1793863000534));
#19633=CARTESIAN_POINT('Ctrl Pts',(-7.4848099313172,-0.270574496756368,
17.1918672333016));
#19634=CARTESIAN_POINT('Ctrl Pts',(-7.48353667075686,-0.00487092690888051,
17.2043481665498));
#19635=CARTESIAN_POINT('Ctrl Pts',(-7.48226341019652,0.260832642938607,
17.216829099798));
#19636=CARTESIAN_POINT('Ctrl Pts',(-7.59019703546719,0.525433154239874,
17.2293100330461));
#19637=CARTESIAN_POINT('Ctrl Pts',(-7.77695120652474,0.71443814839283,17.2417909662943));
#19638=CARTESIAN_POINT('Ctrl Pts',(-7.9637053775823,0.903443142545787,17.2542718995425));
#19639=CARTESIAN_POINT('Ctrl Pts',(-8.22699388814766,1.01453885915643,17.2667528327907));
#19640=CARTESIAN_POINT('Ctrl Pts',(-8.49269364459097,1.01644874085988,17.2792337660389));
#19641=CARTESIAN_POINT('Ctrl Pts',(-8.75839340103428,1.01835862256333,17.2917146992871));
#19642=CARTESIAN_POINT('Ctrl Pts',(-9.02325176140333,0.911059288979299,
17.3041956325353));
#19643=CARTESIAN_POINT('Ctrl Pts',(-9.21270367535798,0.724758509267903,
17.3166765657835));
#19644=CARTESIAN_POINT('Ctrl Pts',(-9.40215558931262,0.538457729556507,
17.3291574990317));
#19645=CARTESIAN_POINT('Ctrl Pts',(-9.51388182535826,0.275436159672903,
17.3416384322799));
#19646=CARTESIAN_POINT('Ctrl Pts',(-9.51642831724057,0.00974174196480255,
17.3541193655281));
#19647=CARTESIAN_POINT('Ctrl Pts',(-9.51645943884197,0.00649459406719165,
17.3542718995425));
#19648=CARTESIAN_POINT('Ctrl Pts',(-9.516475,0.00324729703426298,17.354424433557));
#19649=CARTESIAN_POINT('Ctrl Pts',(-9.516475,8.77823209263609E-13,17.3545769675715));
#19650=CARTESIAN_POINT('Origin',(-8.5,0.,1.24542303242842));
#19651=CARTESIAN_POINT('',(-9.516475,8.07046530902072E-13,16.6954230324285));
#19652=CARTESIAN_POINT('',(-9.51596013594239,0.000134652220364405,16.7545769675715));
#19653=CARTESIAN_POINT('',(-9.516475,1.78524650477582E-12,1.24542303242842));
#19654=CARTESIAN_POINT('Ctrl Pts',(-9.516475,7.49266616715532E-13,16.6954230324285));
#19655=CARTESIAN_POINT('Ctrl Pts',(-9.5164750000002,-0.265706620583219,
16.7079039656767));
#19656=CARTESIAN_POINT('Ctrl Pts',(-9.40727465387234,-0.529786878176472,
16.7203848989248));
#19657=CARTESIAN_POINT('Ctrl Pts',(-9.21961691907808,-0.717894780174342,
16.732865832173));
#19658=CARTESIAN_POINT('Ctrl Pts',(-9.03195918428382,-0.906002682172212,
16.7453467654212));
#19659=CARTESIAN_POINT('Ctrl Pts',(-8.76814132834427,-1.01583545019896,
16.7578276986694));
#19660=CARTESIAN_POINT('Ctrl Pts',(-8.50243547044552,-1.0164720823066,16.7703086319176));
#19661=CARTESIAN_POINT('Ctrl Pts',(-8.23672961254676,-1.01710871441423,
16.7827895651658));
#19662=CARTESIAN_POINT('Ctrl Pts',(-7.97238846933377,-0.908541417083001,
16.795270498414));
#19663=CARTESIAN_POINT('Ctrl Pts',(-7.78383148002373,-0.721334926798913,
16.8077514316622));
#19664=CARTESIAN_POINT('Ctrl Pts',(-7.59527449071369,-0.534128436514826,
16.8202323649104));
#19665=CARTESIAN_POINT('Ctrl Pts',(-7.48480993131715,-0.270574496756204,
16.8327132981586));
#19666=CARTESIAN_POINT('Ctrl Pts',(-7.48353667075686,-0.00487092690871609,
16.8451942314067));
#19667=CARTESIAN_POINT('Ctrl Pts',(-7.48226341019656,0.260832642938771,
16.8576751646549));
#19668=CARTESIAN_POINT('Ctrl Pts',(-7.59019703546727,0.525433154240021,
16.8701560979031));
#19669=CARTESIAN_POINT('Ctrl Pts',(-7.77695120652486,0.714438148392947,
16.8826370311513));
#19670=CARTESIAN_POINT('Ctrl Pts',(-7.96370537758244,0.903443142545873,
16.8951179643995));
#19671=CARTESIAN_POINT('Ctrl Pts',(-8.22699388814783,1.01453885915647,16.9075988976477));
#19672=CARTESIAN_POINT('Ctrl Pts',(-8.49269364459114,1.01644874085988,16.9200798308959));
#19673=CARTESIAN_POINT('Ctrl Pts',(-8.75839340103444,1.01835862256329,16.9325607641441));
#19674=CARTESIAN_POINT('Ctrl Pts',(-9.02325176140348,0.911059288979215,
16.9450416973923));
#19675=CARTESIAN_POINT('Ctrl Pts',(-9.21270367535809,0.724758509267788,
16.9575226306405));
#19676=CARTESIAN_POINT('Ctrl Pts',(-9.40215558931271,0.538457729556361,
16.9700035638887));
#19677=CARTESIAN_POINT('Ctrl Pts',(-9.5138818253583,0.275436159672739,16.9824844971368));
#19678=CARTESIAN_POINT('Ctrl Pts',(-9.51642831724057,0.00974174196463813,
16.994965430385));
#19679=CARTESIAN_POINT('Ctrl Pts',(-9.51645943884197,0.00649459406706575,
16.9951179643995));
#19680=CARTESIAN_POINT('Ctrl Pts',(-9.516475,0.00324729703417569,16.995270498414));
#19681=CARTESIAN_POINT('Ctrl Pts',(-9.516475,8.28962963293057E-13,16.9954230324285));
#19682=CARTESIAN_POINT('Ctrl Pts',(-9.516475,8.33990344481639E-13,16.7545769675715));
#19683=CARTESIAN_POINT('Ctrl Pts',(-9.51647500000022,-0.265706620583135,
16.7670579008197));
#19684=CARTESIAN_POINT('Ctrl Pts',(-9.40727465387239,-0.529786878176396,
16.7795388340679));
#19685=CARTESIAN_POINT('Ctrl Pts',(-9.21961691907814,-0.717894780174282,
16.7920197673161));
#19686=CARTESIAN_POINT('Ctrl Pts',(-9.0319591842839,-0.906002682172167,
16.8045007005642));
#19687=CARTESIAN_POINT('Ctrl Pts',(-8.76814132834435,-1.01583545019894,
16.8169816338124));
#19688=CARTESIAN_POINT('Ctrl Pts',(-8.5024354704456,-1.0164720823066,16.8294625670606));
#19689=CARTESIAN_POINT('Ctrl Pts',(-8.23672961254685,-1.01710871441426,
16.8419435003088));
#19690=CARTESIAN_POINT('Ctrl Pts',(-7.97238846933384,-0.908541417083045,
16.854424433557));
#19691=CARTESIAN_POINT('Ctrl Pts',(-7.78383148002379,-0.721334926798973,
16.8669053668052));
#19692=CARTESIAN_POINT('Ctrl Pts',(-7.59527449071373,-0.534128436514901,
16.8793863000534));
#19693=CARTESIAN_POINT('Ctrl Pts',(-7.48480993131718,-0.270574496756288,
16.8918672333016));
#19694=CARTESIAN_POINT('Ctrl Pts',(-7.48353667075686,-0.00487092690880082,
16.9043481665498));
#19695=CARTESIAN_POINT('Ctrl Pts',(-7.48226341019654,0.260832642938687,
16.916829099798));
#19696=CARTESIAN_POINT('Ctrl Pts',(-7.59019703546723,0.525433154239945,
16.9293100330461));
#19697=CARTESIAN_POINT('Ctrl Pts',(-7.7769512065248,0.714438148392887,16.9417909662943));
#19698=CARTESIAN_POINT('Ctrl Pts',(-7.96370537758237,0.903443142545829,
16.9542718995425));
#19699=CARTESIAN_POINT('Ctrl Pts',(-8.22699388814774,1.01453885915645,16.9667528327907));
#19700=CARTESIAN_POINT('Ctrl Pts',(-8.49269364459105,1.01644874085988,16.9792337660389));
#19701=CARTESIAN_POINT('Ctrl Pts',(-8.75839340103436,1.01835862256331,16.9917146992871));
#19702=CARTESIAN_POINT('Ctrl Pts',(-9.0232517614034,0.911059288979258,17.0041956325353));
#19703=CARTESIAN_POINT('Ctrl Pts',(-9.21270367535803,0.724758509267847,
17.0166765657835));
#19704=CARTESIAN_POINT('Ctrl Pts',(-9.40215558931266,0.538457729556436,
17.0291574990317));
#19705=CARTESIAN_POINT('Ctrl Pts',(-9.51388182535828,0.275436159672823,
17.0416384322799));
#19706=CARTESIAN_POINT('Ctrl Pts',(-9.51642831724057,0.00974174196472285,
17.0541193655281));
#19707=CARTESIAN_POINT('Ctrl Pts',(-9.51645943884197,0.00649459406715047,
17.0542718995425));
#19708=CARTESIAN_POINT('Ctrl Pts',(-9.516475,0.00324729703426041,17.054424433557));
#19709=CARTESIAN_POINT('Ctrl Pts',(-9.516475,9.13686691059164E-13,17.0545769675715));
#19710=CARTESIAN_POINT('Origin',(-8.5,0.,1.24542303242842));
#19711=CARTESIAN_POINT('',(-9.5164968973349,-2.65839347229251E-5,16.3954230324285));
#19712=CARTESIAN_POINT('',(-9.51655837487022,5.83812892711161E-5,16.4545769675715));
#19713=CARTESIAN_POINT('',(-9.516475,1.78524650477582E-12,1.24542303242842));
#19714=CARTESIAN_POINT('Ctrl Pts',(-9.516475,7.85130098511087E-13,16.3954230324285));
#19715=CARTESIAN_POINT('Ctrl Pts',(-9.51647500000021,-0.265706620583203,
16.4079039656767));
#19716=CARTESIAN_POINT('Ctrl Pts',(-9.40727465387235,-0.529786878176478,
16.4203848989248));
#19717=CARTESIAN_POINT('Ctrl Pts',(-9.21961691907807,-0.717894780174357,
16.432865832173));
#19718=CARTESIAN_POINT('Ctrl Pts',(-9.03195918428379,-0.906002682172237,
16.4453467654212));
#19719=CARTESIAN_POINT('Ctrl Pts',(-8.76814132834421,-1.01583545019898,
16.4578276986694));
#19720=CARTESIAN_POINT('Ctrl Pts',(-8.50243547044544,-1.0164720823066,16.4703086319176));
#19721=CARTESIAN_POINT('Ctrl Pts',(-8.23672961254666,-1.01710871441421,
16.4827895651658));
#19722=CARTESIAN_POINT('Ctrl Pts',(-7.97238846933366,-0.908541417082943,
16.495270498414));
#19723=CARTESIAN_POINT('Ctrl Pts',(-7.78383148002363,-0.721334926798817,
16.5077514316622));
#19724=CARTESIAN_POINT('Ctrl Pts',(-7.5952744907136,-0.53412843651469,16.5202323649104));
#19725=CARTESIAN_POINT('Ctrl Pts',(-7.4848099313171,-0.270574496756028,
16.5327132981586));
#19726=CARTESIAN_POINT('Ctrl Pts',(-7.48353667075686,-0.00487092690852084,
16.5451942314068));
#19727=CARTESIAN_POINT('Ctrl Pts',(-7.48226341019661,0.260832642938986,
16.5576751646549));
#19728=CARTESIAN_POINT('Ctrl Pts',(-7.59019703546739,0.525433154240234,
16.5701560979031));
#19729=CARTESIAN_POINT('Ctrl Pts',(-7.77695120652504,0.714438148393127,
16.5826370311513));
#19730=CARTESIAN_POINT('Ctrl Pts',(-7.96370537758268,0.903443142546021,
16.5951179643995));
#19731=CARTESIAN_POINT('Ctrl Pts',(-8.22699388814812,1.01453885915655,16.6075988976477));
#19732=CARTESIAN_POINT('Ctrl Pts',(-8.49269364459145,1.01644874085988,16.6200798308959));
#19733=CARTESIAN_POINT('Ctrl Pts',(-8.75839340103477,1.01835862256321,16.6325607641441));
#19734=CARTESIAN_POINT('Ctrl Pts',(-9.02325176140379,0.911059288979039,
16.6450416973923));
#19735=CARTESIAN_POINT('Ctrl Pts',(-9.21270367535836,0.724758509267529,
16.6575226306405));
#19736=CARTESIAN_POINT('Ctrl Pts',(-9.40215558931292,0.53845772955602,16.6700035638887));
#19737=CARTESIAN_POINT('Ctrl Pts',(-9.51388182535842,0.275436159672333,
16.6824844971369));
#19738=CARTESIAN_POINT('Ctrl Pts',(-9.51642831724057,0.00974174196421177,
16.6949654303851));
#19739=CARTESIAN_POINT('Ctrl Pts',(-9.51645943884197,0.00649459406675493,
16.6951179643995));
#19740=CARTESIAN_POINT('Ctrl Pts',(-9.516475,0.00324729703398035,16.695270498414));
#19741=CARTESIAN_POINT('Ctrl Pts',(-9.516475,7.49266616715532E-13,16.6954230324285));
#19742=CARTESIAN_POINT('Ctrl Pts',(-9.51726025283138,0.000549854815502043,
16.4545769675715));
#19743=CARTESIAN_POINT('Ctrl Pts',(-9.51657489923479,-0.114420558160816,
16.4599867618965));
#19744=CARTESIAN_POINT('Ctrl Pts',(-9.46572759915602,-0.399134064589724,
16.4733502267973));
#19745=CARTESIAN_POINT('Ctrl Pts',(-9.11467520479983,-0.938000704161855,
16.5026210328498));
#19746=CARTESIAN_POINT('Ctrl Pts',(-8.18204041706793,-1.15983848287103,
16.5423893857288));
#19747=CARTESIAN_POINT('Ctrl Pts',(-7.35207269505694,-0.358269358953146,
16.5901114091837));
#19748=CARTESIAN_POINT('Ctrl Pts',(-7.57822133797448,0.770938669115475,
16.6378334326386));
#19749=CARTESIAN_POINT('Ctrl Pts',(-8.64964987006652,1.19318859338267,16.6855554560934));
#19750=CARTESIAN_POINT('Ctrl Pts',(-9.41265229748654,0.642636493326239,
16.7244699677377));
#19751=CARTESIAN_POINT('Ctrl Pts',(-9.5151794075,0.152076348271911,16.7474771382304));
#19752=CARTESIAN_POINT('Ctrl Pts',(-9.51462108838776,0.000484852865797483,
16.7545769675715));
#19753=CARTESIAN_POINT('Origin',(-8.5,0.,1.24542303242842));
#19754=CARTESIAN_POINT('',(-9.5160543088948,-7.03488242669728E-5,16.0954230324285));
#19755=CARTESIAN_POINT('',(-9.51662919665684,-7.0250937289264E-5,16.1545769675715));
#19756=CARTESIAN_POINT('',(-9.516475,1.78524650477582E-12,1.24542303242842));
#19757=CARTESIAN_POINT('Ctrl Pts',(-9.51497316338417,-0.000251140182777485,
16.0954230324285));
#19758=CARTESIAN_POINT('Ctrl Pts',(-9.51542015839452,-0.151106629532047,
16.1024843671052));
#19759=CARTESIAN_POINT('Ctrl Pts',(-9.41308036725428,-0.641309918179512,
16.1254530429335));
#19760=CARTESIAN_POINT('Ctrl Pts',(-8.65222970570018,-1.19292557033944,
16.1643290599136));
#19761=CARTESIAN_POINT('Ctrl Pts',(-7.75981223837764,-0.842543822233083,
16.2040974127926));
#19762=CARTESIAN_POINT('Ctrl Pts',(-7.46421470806744,-0.209092634934189,
16.2359120950958));
#19763=CARTESIAN_POINT('Ctrl Pts',(-7.49095487068437,0.48940290682626,16.2677267773991));
#19764=CARTESIAN_POINT('Ctrl Pts',(-8.17744624771311,1.15857095575367,16.3074951302781));
#19765=CARTESIAN_POINT('Ctrl Pts',(-9.24219277385032,0.910507051205119,
16.3527117721465));
#19766=CARTESIAN_POINT('Ctrl Pts',(-9.514732772302,0.283866876007315,16.3820210728633));
#19767=CARTESIAN_POINT('Ctrl Pts',(-9.51712864820514,-0.000793545963003017,
16.3954230324284));
#19768=CARTESIAN_POINT('Ctrl Pts',(-9.516475,8.47937393886208E-13,16.1545769675715));
#19769=CARTESIAN_POINT('Ctrl Pts',(-9.51647500000022,-0.265706620583101,
16.1670579008197));
#19770=CARTESIAN_POINT('Ctrl Pts',(-9.40727465387241,-0.529786878176346,
16.1795388340679));
#19771=CARTESIAN_POINT('Ctrl Pts',(-9.21961691907819,-0.717894780174231,
16.1920197673161));
#19772=CARTESIAN_POINT('Ctrl Pts',(-9.03195918428398,-0.906002682172116,
16.2045007005642));
#19773=CARTESIAN_POINT('Ctrl Pts',(-8.76814132834446,-1.0158354501989,16.2169816338124));
#19774=CARTESIAN_POINT('Ctrl Pts',(-8.50243547044573,-1.0164720823066,16.2294625670606));
#19775=CARTESIAN_POINT('Ctrl Pts',(-8.236729612547,-1.01710871441429,16.2419435003088));
#19776=CARTESIAN_POINT('Ctrl Pts',(-7.972388469334,-0.908541417083129,16.254424433557));
#19777=CARTESIAN_POINT('Ctrl Pts',(-7.78383148002392,-0.721334926799105,
16.2669053668052));
#19778=CARTESIAN_POINT('Ctrl Pts',(-7.59527449071384,-0.534128436515081,
16.2793863000534));
#19779=CARTESIAN_POINT('Ctrl Pts',(-7.48480993131724,-0.270574496756514,
16.2918672333016));
#19780=CARTESIAN_POINT('Ctrl Pts',(-7.48353667075686,-0.00487092690904588,
16.3043481665498));
#19781=CARTESIAN_POINT('Ctrl Pts',(-7.48226341019648,0.260832642938422,
16.3168290997979));
#19782=CARTESIAN_POINT('Ctrl Pts',(-7.59019703546709,0.525433154239688,
16.3293100330461));
#19783=CARTESIAN_POINT('Ctrl Pts',(-7.77695120652459,0.714438148392672,
16.3417909662943));
#19784=CARTESIAN_POINT('Ctrl Pts',(-7.96370537758209,0.903443142545655,
16.3542718995425));
#19785=CARTESIAN_POINT('Ctrl Pts',(-8.2269938881474,1.01453885915635,16.3667528327907));
#19786=CARTESIAN_POINT('Ctrl Pts',(-8.49269364459069,1.01644874085988,16.3792337660389));
#19787=CARTESIAN_POINT('Ctrl Pts',(-8.75839340103398,1.01835862256341,16.3917146992871));
#19788=CARTESIAN_POINT('Ctrl Pts',(-9.02325176140304,0.91105928897946,16.4041956325353));
#19789=CARTESIAN_POINT('Ctrl Pts',(-9.21270367535773,0.724758509268141,
16.4166765657835));
#19790=CARTESIAN_POINT('Ctrl Pts',(-9.40215558931243,0.538457729556821,
16.4291574990316));
#19791=CARTESIAN_POINT('Ctrl Pts',(-9.51388182535815,0.275436159673279,
16.4416384322798));
#19792=CARTESIAN_POINT('Ctrl Pts',(-9.51642831724056,0.00974174196519902,
16.454119365528));
#19793=CARTESIAN_POINT('Ctrl Pts',(-9.51645943884197,0.00649459406745332,
16.4542718995425));
#19794=CARTESIAN_POINT('Ctrl Pts',(-9.516475,0.00324729703438987,16.454424433557));
#19795=CARTESIAN_POINT('Ctrl Pts',(-9.516475,8.69853826277193E-13,16.4545769675715));
#19796=CARTESIAN_POINT('Origin',(-8.5,0.,1.24542303242842));
#19797=CARTESIAN_POINT('',(-9.516475,7.41297233729117E-13,15.7954230324285));
#19798=CARTESIAN_POINT('',(-9.51632173115293,-4.86293170693105E-5,15.8545769675715));
#19799=CARTESIAN_POINT('',(-9.516475,1.78524650477582E-12,1.24542303242842));
#19800=CARTESIAN_POINT('Ctrl Pts',(-9.516475,7.41297233729117E-13,15.7954230324285));
#19801=CARTESIAN_POINT('Ctrl Pts',(-9.51647500000019,-0.265706620583227,
15.8079039656767));
#19802=CARTESIAN_POINT('Ctrl Pts',(-9.40727465387234,-0.529786878176479,
15.8203848989248));
#19803=CARTESIAN_POINT('Ctrl Pts',(-9.21961691907808,-0.717894780174347,
15.832865832173));
#19804=CARTESIAN_POINT('Ctrl Pts',(-9.03195918428382,-0.906002682172216,
15.8453467654212));
#19805=CARTESIAN_POINT('Ctrl Pts',(-8.76814132834426,-1.01583545019896,
15.8578276986694));
#19806=CARTESIAN_POINT('Ctrl Pts',(-8.50243547044551,-1.0164720823066,15.8703086319176));
#19807=CARTESIAN_POINT('Ctrl Pts',(-8.23672961254675,-1.01710871441423,
15.8827895651658));
#19808=CARTESIAN_POINT('Ctrl Pts',(-7.97238846933376,-0.908541417082997,
15.895270498414));
#19809=CARTESIAN_POINT('Ctrl Pts',(-7.78383148002372,-0.721334926798908,
15.9077514316622));
#19810=CARTESIAN_POINT('Ctrl Pts',(-7.59527449071368,-0.534128436514818,
15.9202323649104));
#19811=CARTESIAN_POINT('Ctrl Pts',(-7.48480993131715,-0.270574496756196,
15.9327132981586));
#19812=CARTESIAN_POINT('Ctrl Pts',(-7.48353667075686,-0.00487092690870812,
15.9451942314067));
#19813=CARTESIAN_POINT('Ctrl Pts',(-7.48226341019657,0.260832642938779,
15.9576751646549));
#19814=CARTESIAN_POINT('Ctrl Pts',(-7.59019703546728,0.525433154240028,
15.9701560979031));
#19815=CARTESIAN_POINT('Ctrl Pts',(-7.77695120652487,0.714438148392953,
15.9826370311513));
#19816=CARTESIAN_POINT('Ctrl Pts',(-7.96370537758245,0.903443142545878,
15.9951179643995));
#19817=CARTESIAN_POINT('Ctrl Pts',(-8.22699388814784,1.01453885915647,16.0075988976477));
#19818=CARTESIAN_POINT('Ctrl Pts',(-8.49269364459114,1.01644874085988,16.0200798308959));
#19819=CARTESIAN_POINT('Ctrl Pts',(-8.75839340103445,1.01835862256329,16.0325607641441));
#19820=CARTESIAN_POINT('Ctrl Pts',(-9.02325176140348,0.911059288979211,
16.0450416973923));
#19821=CARTESIAN_POINT('Ctrl Pts',(-9.2127036753581,0.724758509267782,16.0575226306405));
#19822=CARTESIAN_POINT('Ctrl Pts',(-9.40215558931271,0.538457729556354,
16.0700035638887));
#19823=CARTESIAN_POINT('Ctrl Pts',(-9.51388182535831,0.275436159672731,
16.0824844971368));
#19824=CARTESIAN_POINT('Ctrl Pts',(-9.51642831724057,0.00974174196463016,
16.094965430385));
#19825=CARTESIAN_POINT('Ctrl Pts',(-9.51645943884197,0.00649459406705778,
16.0951179643995));
#19826=CARTESIAN_POINT('Ctrl Pts',(-9.516475,0.00324729703416772,16.095270498414));
#19827=CARTESIAN_POINT('Ctrl Pts',(-9.516475,8.20993580306641E-13,16.0954230324285));
#19828=CARTESIAN_POINT('Ctrl Pts',(-9.51501971928355,-0.000461733140268747,
15.8545769675715));
#19829=CARTESIAN_POINT('Ctrl Pts',(-9.5155994996451,-0.140751556887071,
15.8611449975012));
#19830=CARTESIAN_POINT('Ctrl Pts',(-9.42291436670724,-0.620084892104978,
15.8836203685826));
#19831=CARTESIAN_POINT('Ctrl Pts',(-8.68981880352144,-1.18720590861504,
15.9220030808156));
#19832=CARTESIAN_POINT('Ctrl Pts',(-7.60428317324231,-0.801471685911831,
15.9697251042705));
#19833=CARTESIAN_POINT('Ctrl Pts',(-7.34085844261802,0.319812236206833,
16.0174471277253));
#19834=CARTESIAN_POINT('Ctrl Pts',(-8.14340243192267,1.1485135933495,16.0651691511802));
#19835=CARTESIAN_POINT('Ctrl Pts',(-9.08302755349385,0.958038040322845,
16.1049375040593));
#19836=CARTESIAN_POINT('Ctrl Pts',(-9.45854569172234,0.421593892220246,
16.134740109523));
#19837=CARTESIAN_POINT('Ctrl Pts',(-9.51681144570197,0.125735362396135,
16.1486353738352));
#19838=CARTESIAN_POINT('Ctrl Pts',(-9.51746519719392,-0.000451127041978173,
16.1545769675715));
#19839=CARTESIAN_POINT('Origin',(-8.5,0.,1.24542303242842));
#19840=CARTESIAN_POINT('',(-9.51673427260373,-1.76325846619593E-5,15.4954230324285));
#19841=CARTESIAN_POINT('',(-9.516475,7.46324614917698E-13,15.5545769675715));
#19842=CARTESIAN_POINT('',(-9.516475,1.78524650477582E-12,1.24542303242842));
#19843=CARTESIAN_POINT('Ctrl Pts',(-9.516475,7.77160715524671E-13,15.4954230324285));
#19844=CARTESIAN_POINT('Ctrl Pts',(-9.5164750000002,-0.265706620583192,
15.5079039656767));
#19845=CARTESIAN_POINT('Ctrl Pts',(-9.40727465387236,-0.529786878176447,
15.5203848989248));
#19846=CARTESIAN_POINT('Ctrl Pts',(-9.2196169190781,-0.717894780174322,
15.532865832173));
#19847=CARTESIAN_POINT('Ctrl Pts',(-9.03195918428385,-0.906002682172197,
15.5453467654212));
#19848=CARTESIAN_POINT('Ctrl Pts',(-8.7681413283443,-1.01583545019895,15.5578276986694));
#19849=CARTESIAN_POINT('Ctrl Pts',(-8.50243547044554,-1.0164720823066,15.5703086319176));
#19850=CARTESIAN_POINT('Ctrl Pts',(-8.23672961254679,-1.01710871441424,
15.5827895651658));
#19851=CARTESIAN_POINT('Ctrl Pts',(-7.97238846933379,-0.908541417083016,
15.595270498414));
#19852=CARTESIAN_POINT('Ctrl Pts',(-7.78383148002375,-0.721334926798933,
15.6077514316622));
#19853=CARTESIAN_POINT('Ctrl Pts',(-7.5952744907137,-0.53412843651485,15.6202323649104));
#19854=CARTESIAN_POINT('Ctrl Pts',(-7.48480993131716,-0.270574496756232,
15.6327132981586));
#19855=CARTESIAN_POINT('Ctrl Pts',(-7.48353667075686,-0.00487092690874399,
15.6451942314067));
#19856=CARTESIAN_POINT('Ctrl Pts',(-7.48226341019656,0.260832642938744,
15.6576751646549));
#19857=CARTESIAN_POINT('Ctrl Pts',(-7.59019703546726,0.525433154239996,
15.6701560979031));
#19858=CARTESIAN_POINT('Ctrl Pts',(-7.77695120652484,0.714438148392927,
15.6826370311513));
#19859=CARTESIAN_POINT('Ctrl Pts',(-7.96370537758242,0.903443142545859,
15.6951179643995));
#19860=CARTESIAN_POINT('Ctrl Pts',(-8.2269938881478,1.01453885915646,15.7075988976477));
#19861=CARTESIAN_POINT('Ctrl Pts',(-8.49269364459111,1.01644874085988,15.7200798308959));
#19862=CARTESIAN_POINT('Ctrl Pts',(-8.75839340103441,1.0183586225633,15.7325607641441));
#19863=CARTESIAN_POINT('Ctrl Pts',(-9.02325176140345,0.911059288979229,
15.7450416973923));
#19864=CARTESIAN_POINT('Ctrl Pts',(-9.21270367535807,0.724758509267807,
15.7575226306405));
#19865=CARTESIAN_POINT('Ctrl Pts',(-9.4021555893127,0.538457729556386,15.7700035638887));
#19866=CARTESIAN_POINT('Ctrl Pts',(-9.5138818253583,0.275436159672767,15.7824844971368));
#19867=CARTESIAN_POINT('Ctrl Pts',(-9.51642831724057,0.00974174196466602,
15.794965430385));
#19868=CARTESIAN_POINT('Ctrl Pts',(-9.51645943884197,0.00649459406705512,
15.7951179643995));
#19869=CARTESIAN_POINT('Ctrl Pts',(-9.516475,0.00324729703412654,15.795270498414));
#19870=CARTESIAN_POINT('Ctrl Pts',(-9.516475,7.41297233729117E-13,15.7954230324285));
#19871=CARTESIAN_POINT('Ctrl Pts',(-9.516475,8.04104529104238E-13,15.5545769675715));
#19872=CARTESIAN_POINT('Ctrl Pts',(-9.51647500000021,-0.265706620583184,
15.5670579008197));
#19873=CARTESIAN_POINT('Ctrl Pts',(-9.40727465387236,-0.529786878176461,
15.5795388340679));
#19874=CARTESIAN_POINT('Ctrl Pts',(-9.21961691907808,-0.717894780174344,
15.5920197673161));
#19875=CARTESIAN_POINT('Ctrl Pts',(-9.03195918428381,-0.906002682172227,
15.6045007005642));
#19876=CARTESIAN_POINT('Ctrl Pts',(-8.76814132834423,-1.01583545019898,
15.6169816338124));
#19877=CARTESIAN_POINT('Ctrl Pts',(-8.50243547044546,-1.0164720823066,15.6294625670606));
#19878=CARTESIAN_POINT('Ctrl Pts',(-8.23672961254668,-1.01710871441422,
15.6419435003088));
#19879=CARTESIAN_POINT('Ctrl Pts',(-7.97238846933367,-0.908541417082953,
15.654424433557));
#19880=CARTESIAN_POINT('Ctrl Pts',(-7.78383148002364,-0.72133492679883,
15.6669053668052));
#19881=CARTESIAN_POINT('Ctrl Pts',(-7.59527449071361,-0.534128436514707,
15.6793863000534));
#19882=CARTESIAN_POINT('Ctrl Pts',(-7.48480993131711,-0.270574496756047,
15.6918672333016));
#19883=CARTESIAN_POINT('Ctrl Pts',(-7.48353667075686,-0.00487092690853981,
15.7043481665498));
#19884=CARTESIAN_POINT('Ctrl Pts',(-7.48226341019661,0.260832642938967,
15.716829099798));
#19885=CARTESIAN_POINT('Ctrl Pts',(-7.59019703546738,0.525433154240217,
15.7293100330462));
#19886=CARTESIAN_POINT('Ctrl Pts',(-7.77695120652502,0.714438148393114,
15.7417909662944));
#19887=CARTESIAN_POINT('Ctrl Pts',(-7.96370537758267,0.903443142546011,
15.7542718995425));
#19888=CARTESIAN_POINT('Ctrl Pts',(-8.2269938881481,1.01453885915655,15.7667528327907));
#19889=CARTESIAN_POINT('Ctrl Pts',(-8.49269364459143,1.01644874085988,15.7792337660389));
#19890=CARTESIAN_POINT('Ctrl Pts',(-8.75839340103475,1.01835862256322,15.7917146992871));
#19891=CARTESIAN_POINT('Ctrl Pts',(-9.02325176140378,0.911059288979048,
15.8041956325353));
#19892=CARTESIAN_POINT('Ctrl Pts',(-9.21270367535834,0.724758509267543,
15.8166765657835));
#19893=CARTESIAN_POINT('Ctrl Pts',(-9.40215558931291,0.538457729556037,
15.8291574990317));
#19894=CARTESIAN_POINT('Ctrl Pts',(-9.51388182535841,0.275436159672352,
15.8416384322799));
#19895=CARTESIAN_POINT('Ctrl Pts',(-9.51642831724057,0.00974174196423075,
15.8541193655281));
#19896=CARTESIAN_POINT('Ctrl Pts',(-9.51645943884197,0.00649459406679317,
15.8542718995425));
#19897=CARTESIAN_POINT('Ctrl Pts',(-9.516475,0.00324729703403789,15.854424433557));
#19898=CARTESIAN_POINT('Ctrl Pts',(-9.516475,8.26020961495223E-13,15.8545769675715));
#19899=CARTESIAN_POINT('Origin',(-8.5,0.,1.24542303242842));
#19900=CARTESIAN_POINT('',(-9.516475,6.97464221793842E-13,15.1954230324285));
#19901=CARTESIAN_POINT('',(-9.516475,7.24408182526713E-13,15.2545769675715));
#19902=CARTESIAN_POINT('',(-9.516475,1.78524650477582E-12,1.24542303242842));
#19903=CARTESIAN_POINT('Ctrl Pts',(-9.51588249276368,-0.000783484411897156,
15.1954230324285));
#19904=CARTESIAN_POINT('Ctrl Pts',(-9.51674493951057,-0.10355898154087,
15.2002448852244));
#19905=CARTESIAN_POINT('Ctrl Pts',(-9.45513167617793,-0.544468194336532,
15.220974079172));
#19906=CARTESIAN_POINT('Ctrl Pts',(-8.81795958293278,-1.15983848287083,
15.2576106142711));
#19907=CARTESIAN_POINT('Ctrl Pts',(-7.88532479520075,-0.938000704162233,
15.2973789671502));
#19908=CARTESIAN_POINT('Ctrl Pts',(-7.50376303095584,-0.352302076284569,
15.3291936494535));
#19909=CARTESIAN_POINT('Ctrl Pts',(-7.43230033380396,0.343058292157666,
15.3610083317567));
#19910=CARTESIAN_POINT('Ctrl Pts',(-8.01814288331926,1.10187833907963,15.4007766846357));
#19911=CARTESIAN_POINT('Ctrl Pts',(-9.161100060691,1.0008324173858,15.4482328083849));
#19912=CARTESIAN_POINT('Ctrl Pts',(-9.51752766989334,0.331365264287844,
15.4797815909825));
#19913=CARTESIAN_POINT('Ctrl Pts',(-9.5180041082211,-0.000103991438988233,
15.4954230324285));
#19914=CARTESIAN_POINT('Ctrl Pts',(-9.516475,7.24408182526713E-13,15.2545769675715));
#19915=CARTESIAN_POINT('Ctrl Pts',(-9.51647500000019,-0.265706620583264,
15.2670579008197));
#19916=CARTESIAN_POINT('Ctrl Pts',(-9.40727465387231,-0.529786878176532,
15.2795388340679));
#19917=CARTESIAN_POINT('Ctrl Pts',(-9.21961691907802,-0.7178947801744,15.2920197673161));
#19918=CARTESIAN_POINT('Ctrl Pts',(-9.03195918428374,-0.906002682172269,
15.3045007005643));
#19919=CARTESIAN_POINT('Ctrl Pts',(-8.76814132834415,-1.015835450199,15.3169816338124));
#19920=CARTESIAN_POINT('Ctrl Pts',(-8.50243547044538,-1.0164720823066,15.3294625670606));
#19921=CARTESIAN_POINT('Ctrl Pts',(-8.2367296125466,-1.0171087144142,15.3419435003088));
#19922=CARTESIAN_POINT('Ctrl Pts',(-7.9723884693336,-0.908541417082912,
15.354424433557));
#19923=CARTESIAN_POINT('Ctrl Pts',(-7.78383148002359,-0.721334926798774,
15.3669053668052));
#19924=CARTESIAN_POINT('Ctrl Pts',(-7.59527449071357,-0.534128436514636,
15.3793863000534));
#19925=CARTESIAN_POINT('Ctrl Pts',(-7.48480993131709,-0.270574496755967,
15.3918672333016));
#19926=CARTESIAN_POINT('Ctrl Pts',(-7.48353667075686,-0.00487092690846012,
15.4043481665498));
#19927=CARTESIAN_POINT('Ctrl Pts',(-7.48226341019663,0.260832642939047,
15.416829099798));
#19928=CARTESIAN_POINT('Ctrl Pts',(-7.59019703546742,0.525433154240288,
15.4293100330462));
#19929=CARTESIAN_POINT('Ctrl Pts',(-7.77695120652508,0.71443814839317,15.4417909662944));
#19930=CARTESIAN_POINT('Ctrl Pts',(-7.96370537758274,0.903443142546053,
15.4542718995426));
#19931=CARTESIAN_POINT('Ctrl Pts',(-8.22699388814818,1.01453885915657,15.4667528327907));
#19932=CARTESIAN_POINT('Ctrl Pts',(-8.49269364459151,1.01644874085988,15.4792337660389));
#19933=CARTESIAN_POINT('Ctrl Pts',(-8.75839340103483,1.0183586225632,15.4917146992871));
#19934=CARTESIAN_POINT('Ctrl Pts',(-9.02325176140385,0.911059288979007,
15.5041956325353));
#19935=CARTESIAN_POINT('Ctrl Pts',(-9.2127036753584,0.724758509267487,15.5166765657835));
#19936=CARTESIAN_POINT('Ctrl Pts',(-9.40215558931295,0.538457729555966,
15.5291574990317));
#19937=CARTESIAN_POINT('Ctrl Pts',(-9.51388182535844,0.275436159672272,
15.5416384322799));
#19938=CARTESIAN_POINT('Ctrl Pts',(-9.51642831724057,0.00974174196415106,
15.5541193655281));
#19939=CARTESIAN_POINT('Ctrl Pts',(-9.51645943884197,0.00649459406673273,
15.5542718995425));
#19940=CARTESIAN_POINT('Ctrl Pts',(-9.516475,0.00324729703399675,15.554424433557));
#19941=CARTESIAN_POINT('Ctrl Pts',(-9.516475,8.04104529104238E-13,15.5545769675715));
#19942=CARTESIAN_POINT('Origin',(-8.5,0.,1.24542303242842));
#19943=CARTESIAN_POINT('',(-9.516475,6.75547936556161E-13,14.8954230324285));
#19944=CARTESIAN_POINT('',(-9.516475,7.02491750135728E-13,14.9545769675715));
#19945=CARTESIAN_POINT('',(-9.516475,1.78524650477582E-12,1.24542303242842));
#19946=CARTESIAN_POINT('Ctrl Pts',(-9.516475,6.75547936556161E-13,14.8954230324285));
#19947=CARTESIAN_POINT('Ctrl Pts',(-9.51647500000018,-0.265706620583293,
14.9079039656767));
#19948=CARTESIAN_POINT('Ctrl Pts',(-9.4072746538723,-0.529786878176537,
14.9203848989248));
#19949=CARTESIAN_POINT('Ctrl Pts',(-9.21961691907803,-0.717894780174394,
14.932865832173));
#19950=CARTESIAN_POINT('Ctrl Pts',(-9.03195918428376,-0.90600268217225,
14.9453467654212));
#19951=CARTESIAN_POINT('Ctrl Pts',(-8.76814132834419,-1.01583545019898,
14.9578276986694));
#19952=CARTESIAN_POINT('Ctrl Pts',(-8.50243547044544,-1.0164720823066,14.9703086319176));
#19953=CARTESIAN_POINT('Ctrl Pts',(-8.23672961254669,-1.01710871441421,
14.9827895651658));
#19954=CARTESIAN_POINT('Ctrl Pts',(-7.9723884693337,-0.908541417082963,
14.995270498414));
#19955=CARTESIAN_POINT('Ctrl Pts',(-7.78383148002367,-0.721334926798861,
15.0077514316622));
#19956=CARTESIAN_POINT('Ctrl Pts',(-7.59527449071365,-0.53412843651476,
15.0202323649104));
#19957=CARTESIAN_POINT('Ctrl Pts',(-7.48480993131714,-0.27057449675613,
15.0327132981586));
#19958=CARTESIAN_POINT('Ctrl Pts',(-7.48353667075686,-0.00487092690864238,
15.0451942314068));
#19959=CARTESIAN_POINT('Ctrl Pts',(-7.48226341019658,0.260832642938845,
15.0576751646549));
#19960=CARTESIAN_POINT('Ctrl Pts',(-7.59019703546731,0.525433154240087,
15.0701560979031));
#19961=CARTESIAN_POINT('Ctrl Pts',(-7.77695120652491,0.714438148393,15.0826370311513));
#19962=CARTESIAN_POINT('Ctrl Pts',(-7.96370537758251,0.903443142545912,
15.0951179643995));
#19963=CARTESIAN_POINT('Ctrl Pts',(-8.2269938881479,1.01453885915649,15.1075988976477));
#19964=CARTESIAN_POINT('Ctrl Pts',(-8.49269364459121,1.01644874085988,15.1200798308959));
#19965=CARTESIAN_POINT('Ctrl Pts',(-8.75839340103451,1.01835862256327,15.1325607641441));
#19966=CARTESIAN_POINT('Ctrl Pts',(-9.02325176140354,0.911059288979177,
15.1450416973923));
#19967=CARTESIAN_POINT('Ctrl Pts',(-9.21270367535815,0.724758509267736,
15.1575226306405));
#19968=CARTESIAN_POINT('Ctrl Pts',(-9.40215558931275,0.538457729556296,
15.1700035638887));
#19969=CARTESIAN_POINT('Ctrl Pts',(-9.51388182535832,0.275436159672665,
15.1824844971368));
#19970=CARTESIAN_POINT('Ctrl Pts',(-9.51642831724057,0.00974174196456442,
15.194965430385));
#19971=CARTESIAN_POINT('Ctrl Pts',(-9.51645943884197,0.00649459406697277,
15.1951179643995));
#19972=CARTESIAN_POINT('Ctrl Pts',(-9.516475,0.0032472970340634,15.195270498414));
#19973=CARTESIAN_POINT('Ctrl Pts',(-9.516475,6.97464368947146E-13,15.1954230324285));
#19974=CARTESIAN_POINT('Ctrl Pts',(-9.516475,8.18051578508808E-13,14.9545769675715));
#19975=CARTESIAN_POINT('Ctrl Pts',(-9.51647500000021,-0.265706620583151,
14.9670579008197));
#19976=CARTESIAN_POINT('Ctrl Pts',(-9.40727465387238,-0.52978687817641,
14.9795388340679));
#19977=CARTESIAN_POINT('Ctrl Pts',(-9.21961691907813,-0.717894780174293,
14.9920197673161));
#19978=CARTESIAN_POINT('Ctrl Pts',(-9.03195918428389,-0.906002682172176,
15.0045007005642));
#19979=CARTESIAN_POINT('Ctrl Pts',(-8.76814132834434,-1.01583545019894,
15.0169816338124));
#19980=CARTESIAN_POINT('Ctrl Pts',(-8.50243547044558,-1.0164720823066,15.0294625670606));
#19981=CARTESIAN_POINT('Ctrl Pts',(-8.23672961254683,-1.01710871441425,
15.0419435003088));
#19982=CARTESIAN_POINT('Ctrl Pts',(-7.97238846933383,-0.908541417083037,
15.054424433557));
#19983=CARTESIAN_POINT('Ctrl Pts',(-7.78383148002378,-0.721334926798962,
15.0669053668052));
#19984=CARTESIAN_POINT('Ctrl Pts',(-7.59527449071372,-0.534128436514887,
15.0793863000534));
#19985=CARTESIAN_POINT('Ctrl Pts',(-7.48480993131717,-0.270574496756272,
15.0918672333016));
#19986=CARTESIAN_POINT('Ctrl Pts',(-7.48353667075686,-0.00487092690878488,
15.1043481665498));
#19987=CARTESIAN_POINT('Ctrl Pts',(-7.48226341019655,0.260832642938703,
15.116829099798));
#19988=CARTESIAN_POINT('Ctrl Pts',(-7.59019703546724,0.52543315423996,15.1293100330462));
#19989=CARTESIAN_POINT('Ctrl Pts',(-7.77695120652481,0.714438148392898,
15.1417909662943));
#19990=CARTESIAN_POINT('Ctrl Pts',(-7.96370537758238,0.903443142545837,
15.1542718995425));
#19991=CARTESIAN_POINT('Ctrl Pts',(-8.22699388814776,1.01453885915645,15.1667528327907));
#19992=CARTESIAN_POINT('Ctrl Pts',(-8.49269364459107,1.01644874085988,15.1792337660389));
#19993=CARTESIAN_POINT('Ctrl Pts',(-8.75839340103437,1.01835862256331,15.1917146992871));
#19994=CARTESIAN_POINT('Ctrl Pts',(-9.02325176140341,0.91105928897925,15.2041956325353));
#19995=CARTESIAN_POINT('Ctrl Pts',(-9.21270367535804,0.724758509267836,
15.2166765657835));
#19996=CARTESIAN_POINT('Ctrl Pts',(-9.40215558931267,0.538457729556422,
15.2291574990317));
#19997=CARTESIAN_POINT('Ctrl Pts',(-9.51388182535828,0.275436159672807,
15.2416384322799));
#19998=CARTESIAN_POINT('Ctrl Pts',(-9.51642831724057,0.00974174196470691,
15.2541193655281));
#19999=CARTESIAN_POINT('Ctrl Pts',(-9.51645943884197,0.00649459406707676,
15.2542718995425));
#20000=CARTESIAN_POINT('Ctrl Pts',(-9.516475,0.00324729703412887,15.254424433557));
#20001=CARTESIAN_POINT('Ctrl Pts',(-9.516475,7.24408182526713E-13,15.2545769675715));
#20002=CARTESIAN_POINT('Origin',(-8.5,0.,1.24542303242842));
#20003=CARTESIAN_POINT('',(-9.516475,6.53631504165176E-13,14.5954230324285));
#20004=CARTESIAN_POINT('',(-9.516475,6.80575317744743E-13,14.6545769675715));
#20005=CARTESIAN_POINT('',(-9.516475,1.78524650477582E-12,1.24542303242842));
#20006=CARTESIAN_POINT('Ctrl Pts',(-9.516475,7.11411418351716E-13,14.5954230324285));
#20007=CARTESIAN_POINT('Ctrl Pts',(-9.51647500000019,-0.265706620583277,
14.6079039656767));
#20008=CARTESIAN_POINT('Ctrl Pts',(-9.40727465387231,-0.529786878176543,
14.6203848989248));
#20009=CARTESIAN_POINT('Ctrl Pts',(-9.21961691907802,-0.717894780174409,
14.632865832173));
#20010=CARTESIAN_POINT('Ctrl Pts',(-9.03195918428372,-0.906002682172275,
14.6453467654212));
#20011=CARTESIAN_POINT('Ctrl Pts',(-8.76814132834414,-1.015835450199,14.6578276986694));
#20012=CARTESIAN_POINT('Ctrl Pts',(-8.50243547044536,-1.0164720823066,14.6703086319176));
#20013=CARTESIAN_POINT('Ctrl Pts',(-8.23672961254659,-1.01710871441419,
14.6827895651658));
#20014=CARTESIAN_POINT('Ctrl Pts',(-7.97238846933359,-0.908541417082905,
14.695270498414));
#20015=CARTESIAN_POINT('Ctrl Pts',(-7.78383148002358,-0.721334926798765,
14.7077514316622));
#20016=CARTESIAN_POINT('Ctrl Pts',(-7.59527449071356,-0.534128436514624,
14.7202323649104));
#20017=CARTESIAN_POINT('Ctrl Pts',(-7.48480993131708,-0.270574496755954,
14.7327132981586));
#20018=CARTESIAN_POINT('Ctrl Pts',(-7.48353667075686,-0.00487092690844712,
14.7451942314068));
#20019=CARTESIAN_POINT('Ctrl Pts',(-7.48226341019663,0.26083264293906,14.757675164655));
#20020=CARTESIAN_POINT('Ctrl Pts',(-7.59019703546743,0.5254331542403,14.7701560979031));
#20021=CARTESIAN_POINT('Ctrl Pts',(-7.77695120652509,0.71443814839318,14.7826370311513));
#20022=CARTESIAN_POINT('Ctrl Pts',(-7.96370537758275,0.903443142546059,
14.7951179643995));
#20023=CARTESIAN_POINT('Ctrl Pts',(-8.22699388814819,1.01453885915657,14.8075988976477));
#20024=CARTESIAN_POINT('Ctrl Pts',(-8.49269364459152,1.01644874085988,14.8200798308959));
#20025=CARTESIAN_POINT('Ctrl Pts',(-8.75839340103484,1.0183586225632,14.8325607641441));
#20026=CARTESIAN_POINT('Ctrl Pts',(-9.02325176140386,0.911059288979001,
14.8450416973923));
#20027=CARTESIAN_POINT('Ctrl Pts',(-9.21270367535841,0.724758509267478,
14.8575226306405));
#20028=CARTESIAN_POINT('Ctrl Pts',(-9.40215558931296,0.538457729555955,
14.8700035638887));
#20029=CARTESIAN_POINT('Ctrl Pts',(-9.51388182535844,0.275436159672259,
14.8824844971369));
#20030=CARTESIAN_POINT('Ctrl Pts',(-9.51642831724057,0.00974174196413806,
14.8949654303851));
#20031=CARTESIAN_POINT('Ctrl Pts',(-9.51645943884197,0.00649459406668122,
14.8951179643995));
#20032=CARTESIAN_POINT('Ctrl Pts',(-9.516475,0.00324729703390672,14.895270498414));
#20033=CARTESIAN_POINT('Ctrl Pts',(-9.516475,6.75547936556161E-13,14.8954230324285));
#20034=CARTESIAN_POINT('Ctrl Pts',(-9.516475,6.80575317744743E-13,14.6545769675715));
#20035=CARTESIAN_POINT('Ctrl Pts',(-9.51647500000018,-0.265706620583288,
14.6670579008197));
#20036=CARTESIAN_POINT('Ctrl Pts',(-9.40727465387231,-0.529786878176533,
14.6795388340679));
#20037=CARTESIAN_POINT('Ctrl Pts',(-9.21961691907804,-0.71789478017439,
14.6920197673161));
#20038=CARTESIAN_POINT('Ctrl Pts',(-9.03195918428376,-0.906002682172248,
14.7045007005643));
#20039=CARTESIAN_POINT('Ctrl Pts',(-8.7681413283442,-1.01583545019898,14.7169816338124));
#20040=CARTESIAN_POINT('Ctrl Pts',(-8.50243547044545,-1.0164720823066,14.7294625670606));
#20041=CARTESIAN_POINT('Ctrl Pts',(-8.23672961254669,-1.01710871441422,
14.7419435003088));
#20042=CARTESIAN_POINT('Ctrl Pts',(-7.97238846933371,-0.908541417082965,
14.754424433557));
#20043=CARTESIAN_POINT('Ctrl Pts',(-7.78383148002368,-0.721334926798865,
14.7669053668052));
#20044=CARTESIAN_POINT('Ctrl Pts',(-7.59527449071365,-0.534128436514764,
14.7793863000534));
#20045=CARTESIAN_POINT('Ctrl Pts',(-7.48480993131714,-0.270574496756135,
14.7918672333016));
#20046=CARTESIAN_POINT('Ctrl Pts',(-7.48353667075686,-0.0048709269086474,
14.8043481665498));
#20047=CARTESIAN_POINT('Ctrl Pts',(-7.48226341019658,0.26083264293884,14.816829099798));
#20048=CARTESIAN_POINT('Ctrl Pts',(-7.59019703546731,0.525433154240083,
14.8293100330462));
#20049=CARTESIAN_POINT('Ctrl Pts',(-7.77695120652491,0.714438148392996,
14.8417909662943));
#20050=CARTESIAN_POINT('Ctrl Pts',(-7.9637053775825,0.90344314254591,14.8542718995425));
#20051=CARTESIAN_POINT('Ctrl Pts',(-8.2269938881479,1.01453885915649,14.8667528327907));
#20052=CARTESIAN_POINT('Ctrl Pts',(-8.4926936445912,1.01644874085988,14.8792337660389));
#20053=CARTESIAN_POINT('Ctrl Pts',(-8.75839340103451,1.01835862256328,14.8917146992871));
#20054=CARTESIAN_POINT('Ctrl Pts',(-9.02325176140354,0.91105928897918,14.9041956325353));
#20055=CARTESIAN_POINT('Ctrl Pts',(-9.21270367535814,0.72475850926774,14.9166765657835));
#20056=CARTESIAN_POINT('Ctrl Pts',(-9.40215558931275,0.5384577295563,14.9291574990317));
#20057=CARTESIAN_POINT('Ctrl Pts',(-9.51388182535832,0.27543615967267,14.9416384322799));
#20058=CARTESIAN_POINT('Ctrl Pts',(-9.51642831724057,0.00974174196456944,
14.9541193655281));
#20059=CARTESIAN_POINT('Ctrl Pts',(-9.51645943884197,0.00649459406701632,
14.9542718995425));
#20060=CARTESIAN_POINT('Ctrl Pts',(-9.516475,0.00324729703414547,14.954424433557));
#20061=CARTESIAN_POINT('Ctrl Pts',(-9.516475,8.18051578508808E-13,14.9545769675715));
#20062=CARTESIAN_POINT('Origin',(-8.5,0.,1.24542303242842));
#20063=CARTESIAN_POINT('',(-9.516475,6.31715071774191E-13,14.2954230324285));
#20064=CARTESIAN_POINT('',(-9.516475,6.58658885353758E-13,14.3545769675715));
#20065=CARTESIAN_POINT('',(-9.516475,1.78524650477582E-12,1.24542303242842));
#20066=CARTESIAN_POINT('Ctrl Pts',(-9.516475,6.31715071774191E-13,14.2954230324285));
#20067=CARTESIAN_POINT('Ctrl Pts',(-9.51647500000016,-0.265706620583337,
14.3079039656767));
#20068=CARTESIAN_POINT('Ctrl Pts',(-9.40727465387228,-0.529786878176576,
14.3203848989248));
#20069=CARTESIAN_POINT('Ctrl Pts',(-9.219616919078,-0.717894780174425,14.332865832173));
#20070=CARTESIAN_POINT('Ctrl Pts',(-9.03195918428372,-0.906002682172273,
14.3453467654212));
#20071=CARTESIAN_POINT('Ctrl Pts',(-8.76814132834415,-1.01583545019899,
14.3578276986694));
#20072=CARTESIAN_POINT('Ctrl Pts',(-8.5024354704454,-1.0164720823066,14.3703086319176));
#20073=CARTESIAN_POINT('Ctrl Pts',(-8.23672961254664,-1.0171087144142,14.3827895651658));
#20074=CARTESIAN_POINT('Ctrl Pts',(-7.97238846933366,-0.90854141708294,
14.395270498414));
#20075=CARTESIAN_POINT('Ctrl Pts',(-7.78383148002364,-0.72133492679883,
14.4077514316622));
#20076=CARTESIAN_POINT('Ctrl Pts',(-7.59527449071362,-0.534128436514721,
14.4202323649104));
#20077=CARTESIAN_POINT('Ctrl Pts',(-7.48480993131712,-0.270574496756086,
14.4327132981586));
#20078=CARTESIAN_POINT('Ctrl Pts',(-7.48353667075686,-0.00487092690859854,
14.4451942314068));
#20079=CARTESIAN_POINT('Ctrl Pts',(-7.48226341019659,0.260832642938889,
14.4576751646549));
#20080=CARTESIAN_POINT('Ctrl Pts',(-7.59019703546734,0.525433154240126,
14.4701560979031));
#20081=CARTESIAN_POINT('Ctrl Pts',(-7.77695120652494,0.714438148393031,
14.4826370311513));
#20082=CARTESIAN_POINT('Ctrl Pts',(-7.96370537758255,0.903443142545935,
14.4951179643995));
#20083=CARTESIAN_POINT('Ctrl Pts',(-8.22699388814795,1.0145388591565,14.5075988976477));
#20084=CARTESIAN_POINT('Ctrl Pts',(-8.49269364459125,1.01644874085988,14.5200798308959));
#20085=CARTESIAN_POINT('Ctrl Pts',(-8.75839340103456,1.01835862256326,14.5325607641441));
#20086=CARTESIAN_POINT('Ctrl Pts',(-9.02325176140358,0.911059288979154,
14.5450416973923));
#20087=CARTESIAN_POINT('Ctrl Pts',(-9.21270367535818,0.724758509267706,
14.5575226306405));
#20088=CARTESIAN_POINT('Ctrl Pts',(-9.40215558931277,0.538457729556257,
14.5700035638887));
#20089=CARTESIAN_POINT('Ctrl Pts',(-9.51388182535834,0.275436159672622,
14.5824844971368));
#20090=CARTESIAN_POINT('Ctrl Pts',(-9.51642831724057,0.00974174196452058,
14.594965430385));
#20091=CARTESIAN_POINT('Ctrl Pts',(-9.51645943884197,0.0064945940669482,
14.5951179643995));
#20092=CARTESIAN_POINT('Ctrl Pts',(-9.516475,0.00324729703405813,14.595270498414));
#20093=CARTESIAN_POINT('Ctrl Pts',(-9.516475,7.11411418351716E-13,14.5954230324285));
#20094=CARTESIAN_POINT('Ctrl Pts',(-9.516475,7.16438799540298E-13,14.3545769675715));
#20095=CARTESIAN_POINT('Ctrl Pts',(-9.51647500000019,-0.265706620583272,
14.3670579008197));
#20096=CARTESIAN_POINT('Ctrl Pts',(-9.40727465387231,-0.529786878176539,
14.3795388340679));
#20097=CARTESIAN_POINT('Ctrl Pts',(-9.21961691907802,-0.717894780174406,
14.3920197673161));
#20098=CARTESIAN_POINT('Ctrl Pts',(-9.03195918428373,-0.906002682172273,
14.4045007005643));
#20099=CARTESIAN_POINT('Ctrl Pts',(-8.76814132834414,-1.015835450199,14.4169816338124));
#20100=CARTESIAN_POINT('Ctrl Pts',(-8.50243547044537,-1.0164720823066,14.4294625670606));
#20101=CARTESIAN_POINT('Ctrl Pts',(-8.23672961254659,-1.0171087144142,14.4419435003088));
#20102=CARTESIAN_POINT('Ctrl Pts',(-7.9723884693336,-0.908541417082908,
14.454424433557));
#20103=CARTESIAN_POINT('Ctrl Pts',(-7.78383148002358,-0.721334926798768,
14.4669053668052));
#20104=CARTESIAN_POINT('Ctrl Pts',(-7.59527449071356,-0.534128436514628,
14.4793863000534));
#20105=CARTESIAN_POINT('Ctrl Pts',(-7.48480993131709,-0.270574496755959,
14.4918672333016));
#20106=CARTESIAN_POINT('Ctrl Pts',(-7.48353667075686,-0.00487092690845215,
14.5043481665498));
#20107=CARTESIAN_POINT('Ctrl Pts',(-7.48226341019663,0.260832642939055,
14.516829099798));
#20108=CARTESIAN_POINT('Ctrl Pts',(-7.59019703546743,0.525433154240295,
14.5293100330462));
#20109=CARTESIAN_POINT('Ctrl Pts',(-7.77695120652509,0.714438148393176,
14.5417909662944));
#20110=CARTESIAN_POINT('Ctrl Pts',(-7.96370537758274,0.903443142546057,
14.5542718995425));
#20111=CARTESIAN_POINT('Ctrl Pts',(-8.22699388814819,1.01453885915657,14.5667528327907));
#20112=CARTESIAN_POINT('Ctrl Pts',(-8.49269364459151,1.01644874085988,14.5792337660389));
#20113=CARTESIAN_POINT('Ctrl Pts',(-8.75839340103484,1.0183586225632,14.5917146992871));
#20114=CARTESIAN_POINT('Ctrl Pts',(-9.02325176140386,0.911059288979003,
14.6041956325353));
#20115=CARTESIAN_POINT('Ctrl Pts',(-9.21270367535841,0.724758509267481,
14.6166765657835));
#20116=CARTESIAN_POINT('Ctrl Pts',(-9.40215558931295,0.538457729555959,
14.6291574990317));
#20117=CARTESIAN_POINT('Ctrl Pts',(-9.51388182535844,0.275436159672264,
14.6416384322799));
#20118=CARTESIAN_POINT('Ctrl Pts',(-9.51642831724057,0.00974174196414309,
14.6541193655281));
#20119=CARTESIAN_POINT('Ctrl Pts',(-9.51645943884197,0.00649459406668624,
14.6542718995426));
#20120=CARTESIAN_POINT('Ctrl Pts',(-9.516475,0.00324729703391174,14.654424433557));
#20121=CARTESIAN_POINT('Ctrl Pts',(-9.516475,6.80575317744743E-13,14.6545769675715));
#20122=CARTESIAN_POINT('Origin',(-8.5,0.,1.24542303242842));
#20123=CARTESIAN_POINT('',(-9.516475,6.09798639383206E-13,13.9954230324285));
#20124=CARTESIAN_POINT('',(-9.51650473276395,-2.35768713140684E-5,14.0545769675715));
#20125=CARTESIAN_POINT('',(-9.516475,1.78524650477582E-12,1.24542303242842));
#20126=CARTESIAN_POINT('Ctrl Pts',(-9.516475,6.67578553569746E-13,13.9954230324285));
#20127=CARTESIAN_POINT('Ctrl Pts',(-9.51647500000017,-0.265706620583301,
14.0079039656767));
#20128=CARTESIAN_POINT('Ctrl Pts',(-9.4072746538723,-0.529786878176544,
14.0203848989248));
#20129=CARTESIAN_POINT('Ctrl Pts',(-9.21961691907803,-0.717894780174399,
14.032865832173));
#20130=CARTESIAN_POINT('Ctrl Pts',(-9.03195918428375,-0.906002682172254,
14.0453467654212));
#20131=CARTESIAN_POINT('Ctrl Pts',(-8.76814132834419,-1.01583545019898,
14.0578276986694));
#20132=CARTESIAN_POINT('Ctrl Pts',(-8.50243547044543,-1.0164720823066,14.0703086319176));
#20133=CARTESIAN_POINT('Ctrl Pts',(-8.23672961254668,-1.01710871441421,
14.0827895651658));
#20134=CARTESIAN_POINT('Ctrl Pts',(-7.9723884693337,-0.908541417082959,
14.095270498414));
#20135=CARTESIAN_POINT('Ctrl Pts',(-7.78383148002367,-0.721334926798856,
14.1077514316622));
#20136=CARTESIAN_POINT('Ctrl Pts',(-7.59527449071364,-0.534128436514753,
14.1202323649104));
#20137=CARTESIAN_POINT('Ctrl Pts',(-7.48480993131713,-0.270574496756122,
14.1327132981586));
#20138=CARTESIAN_POINT('Ctrl Pts',(-7.48353667075686,-0.0048709269086344,
14.1451942314067));
#20139=CARTESIAN_POINT('Ctrl Pts',(-7.48226341019658,0.260832642938853,
14.1576751646549));
#20140=CARTESIAN_POINT('Ctrl Pts',(-7.59019703546732,0.525433154240094,
14.1701560979031));
#20141=CARTESIAN_POINT('Ctrl Pts',(-7.77695120652492,0.714438148393005,
14.1826370311513));
#20142=CARTESIAN_POINT('Ctrl Pts',(-7.96370537758252,0.903443142545917,
14.1951179643995));
#20143=CARTESIAN_POINT('Ctrl Pts',(-8.22699388814791,1.01453885915649,14.2075988976477));
#20144=CARTESIAN_POINT('Ctrl Pts',(-8.49269364459122,1.01644874085988,14.2200798308959));
#20145=CARTESIAN_POINT('Ctrl Pts',(-8.75839340103452,1.01835862256327,14.2325607641441));
#20146=CARTESIAN_POINT('Ctrl Pts',(-9.02325176140355,0.911059288979173,
14.2450416973923));
#20147=CARTESIAN_POINT('Ctrl Pts',(-9.21270367535815,0.724758509267731,
14.2575226306405));
#20148=CARTESIAN_POINT('Ctrl Pts',(-9.40215558931275,0.538457729556288,
14.2700035638887));
#20149=CARTESIAN_POINT('Ctrl Pts',(-9.51388182535833,0.275436159672657,
14.2824844971368));
#20150=CARTESIAN_POINT('Ctrl Pts',(-9.51642831724057,0.00974174196455645,
14.294965430385));
#20151=CARTESIAN_POINT('Ctrl Pts',(-9.51645943884197,0.00649459406694554,
14.2951179643995));
#20152=CARTESIAN_POINT('Ctrl Pts',(-9.516475,0.00324729703401696,14.295270498414));
#20153=CARTESIAN_POINT('Ctrl Pts',(-9.516475,6.31715071774191E-13,14.2954230324285));
#20154=CARTESIAN_POINT('Ctrl Pts',(-9.516475,6.36742452962773E-13,14.0545769675715));
#20155=CARTESIAN_POINT('Ctrl Pts',(-9.51647500000017,-0.265706620583313,
14.0670579008197));
#20156=CARTESIAN_POINT('Ctrl Pts',(-9.4072746538723,-0.529786878176534,
14.0795388340679));
#20157=CARTESIAN_POINT('Ctrl Pts',(-9.21961691907805,-0.71789478017438,
14.0920197673161));
#20158=CARTESIAN_POINT('Ctrl Pts',(-9.03195918428379,-0.906002682172227,
14.1045007005642));
#20159=CARTESIAN_POINT('Ctrl Pts',(-8.76814132834425,-1.01583545019896,
14.1169816338124));
#20160=CARTESIAN_POINT('Ctrl Pts',(-8.50243547044552,-1.0164720823066,14.1294625670606));
#20161=CARTESIAN_POINT('Ctrl Pts',(-8.23672961254679,-1.01710871441423,
14.1419435003088));
#20162=CARTESIAN_POINT('Ctrl Pts',(-7.97238846933381,-0.908541417083019,
14.154424433557));
#20163=CARTESIAN_POINT('Ctrl Pts',(-7.78383148002377,-0.721334926798956,
14.1669053668052));
#20164=CARTESIAN_POINT('Ctrl Pts',(-7.59527449071373,-0.534128436514893,
14.1793863000534));
#20165=CARTESIAN_POINT('Ctrl Pts',(-7.48480993131719,-0.270574496756303,
14.1918672333016));
#20166=CARTESIAN_POINT('Ctrl Pts',(-7.48353667075686,-0.00487092690883469,
14.2043481665498));
#20167=CARTESIAN_POINT('Ctrl Pts',(-7.48226341019653,0.260832642938633,
14.216829099798));
#20168=CARTESIAN_POINT('Ctrl Pts',(-7.5901970354672,0.525433154239877,14.2293100330461));
#20169=CARTESIAN_POINT('Ctrl Pts',(-7.77695120652474,0.714438148392822,
14.2417909662943));
#20170=CARTESIAN_POINT('Ctrl Pts',(-7.96370537758227,0.903443142545767,
14.2542718995425));
#20171=CARTESIAN_POINT('Ctrl Pts',(-8.22699388814761,1.01453885915641,14.2667528327907));
#20172=CARTESIAN_POINT('Ctrl Pts',(-8.4926936445909,1.01644874085988,14.2792337660389));
#20173=CARTESIAN_POINT('Ctrl Pts',(-8.75839340103419,1.01835862256335,14.2917146992871));
#20174=CARTESIAN_POINT('Ctrl Pts',(-9.02325176140323,0.911059288979352,
14.3041956325353));
#20175=CARTESIAN_POINT('Ctrl Pts',(-9.21270367535788,0.724758509267993,
14.3166765657835));
#20176=CARTESIAN_POINT('Ctrl Pts',(-9.40215558931254,0.538457729556634,
14.3291574990317));
#20177=CARTESIAN_POINT('Ctrl Pts',(-9.51388182535821,0.275436159673068,
14.3416384322799));
#20178=CARTESIAN_POINT('Ctrl Pts',(-9.51642831724057,0.00974174196498783,
14.354119365528));
#20179=CARTESIAN_POINT('Ctrl Pts',(-9.51645943884197,0.00649459406726139,
14.3542718995425));
#20180=CARTESIAN_POINT('Ctrl Pts',(-9.516475,0.00324729703421724,14.354424433557));
#20181=CARTESIAN_POINT('Ctrl Pts',(-9.516475,7.16438799540298E-13,14.3545769675715));
#20182=CARTESIAN_POINT('Origin',(-8.5,0.,1.24542303242842));
#20183=CARTESIAN_POINT('',(-9.516475,5.87882206992221E-13,13.6954230324285));
#20184=CARTESIAN_POINT('',(-9.51614186447112,-9.25009508935906E-5,13.7545769675715));
#20185=CARTESIAN_POINT('',(-9.516475,1.78524650477582E-12,1.24542303242842));
#20186=CARTESIAN_POINT('Ctrl Pts',(-9.516475,5.87882206992221E-13,13.6954230324285));
#20187=CARTESIAN_POINT('Ctrl Pts',(-9.51647500000015,-0.265706620583381,
13.7079039656767));
#20188=CARTESIAN_POINT('Ctrl Pts',(-9.40727465387226,-0.529786878176616,
13.7203848989249));
#20189=CARTESIAN_POINT('Ctrl Pts',(-9.21961691907797,-0.717894780174456,
13.732865832173));
#20190=CARTESIAN_POINT('Ctrl Pts',(-9.03195918428368,-0.906002682172296,
13.7453467654212));
#20191=CARTESIAN_POINT('Ctrl Pts',(-8.76814132834411,-1.015835450199,13.7578276986694));
#20192=CARTESIAN_POINT('Ctrl Pts',(-8.50243547044535,-1.0164720823066,13.7703086319176));
#20193=CARTESIAN_POINT('Ctrl Pts',(-8.2367296125466,-1.01710871441419,13.7827895651658));
#20194=CARTESIAN_POINT('Ctrl Pts',(-7.97238846933362,-0.908541417082917,
13.795270498414));
#20195=CARTESIAN_POINT('Ctrl Pts',(-7.78383148002361,-0.7213349267988,13.8077514316622));
#20196=CARTESIAN_POINT('Ctrl Pts',(-7.5952744907136,-0.534128436514682,
13.8202323649104));
#20197=CARTESIAN_POINT('Ctrl Pts',(-7.48480993131711,-0.270574496756043,
13.8327132981586));
#20198=CARTESIAN_POINT('Ctrl Pts',(-7.48353667075686,-0.00487092690855471,
13.8451942314068));
#20199=CARTESIAN_POINT('Ctrl Pts',(-7.48226341019661,0.260832642938933,
13.8576751646549));
#20200=CARTESIAN_POINT('Ctrl Pts',(-7.59019703546736,0.525433154240165,
13.8701560979031));
#20201=CARTESIAN_POINT('Ctrl Pts',(-7.77695120652497,0.714438148393062,
13.8826370311513));
#20202=CARTESIAN_POINT('Ctrl Pts',(-7.96370537758259,0.903443142545958,
13.8951179643995));
#20203=CARTESIAN_POINT('Ctrl Pts',(-8.22699388814799,1.01453885915651,13.9075988976477));
#20204=CARTESIAN_POINT('Ctrl Pts',(-8.4926936445913,1.01644874085988,13.9200798308959));
#20205=CARTESIAN_POINT('Ctrl Pts',(-8.7583934010346,1.01835862256325,13.9325607641441));
#20206=CARTESIAN_POINT('Ctrl Pts',(-9.02325176140362,0.911059288979132,
13.9450416973923));
#20207=CARTESIAN_POINT('Ctrl Pts',(-9.21270367535821,0.724758509267675,
13.9575226306405));
#20208=CARTESIAN_POINT('Ctrl Pts',(-9.40215558931279,0.538457729556218,
13.9700035638887));
#20209=CARTESIAN_POINT('Ctrl Pts',(-9.51388182535835,0.275436159672578,
13.9824844971369));
#20210=CARTESIAN_POINT('Ctrl Pts',(-9.51642831724057,0.00974174196447676,
13.994965430385));
#20211=CARTESIAN_POINT('Ctrl Pts',(-9.51645943884197,0.00649459406690437,
13.9951179643995));
#20212=CARTESIAN_POINT('Ctrl Pts',(-9.516475,0.0032472970340143,13.995270498414));
#20213=CARTESIAN_POINT('Ctrl Pts',(-9.516475,6.67578553569746E-13,13.9954230324285));
#20214=CARTESIAN_POINT('Ctrl Pts',(-9.51504772062611,-0.000396309267489167,
13.7545769675715));
#20215=CARTESIAN_POINT('Ctrl Pts',(-9.51566105818666,-0.142309670683462,
13.7612219868299));
#20216=CARTESIAN_POINT('Ctrl Pts',(-9.42163809550689,-0.623275699977225,
13.78377434724));
#20217=CARTESIAN_POINT('Ctrl Pts',(-8.68330312999737,-1.18858044034005,
13.8222340488017));
#20218=CARTESIAN_POINT('Ctrl Pts',(-7.78213757023688,-0.861594151033408,
13.8620024016807));
#20219=CARTESIAN_POINT('Ctrl Pts',(-7.47002326942581,-0.236120563005943,
13.893817083984));
#20220=CARTESIAN_POINT('Ctrl Pts',(-7.47851070073035,0.462850473304309,
13.9256317662872));
#20221=CARTESIAN_POINT('Ctrl Pts',(-8.14724805356803,1.14973456280755,13.9654001191663));
#20222=CARTESIAN_POINT('Ctrl Pts',(-9.22798704108243,0.927582382414148,
14.011033076453));
#20223=CARTESIAN_POINT('Ctrl Pts',(-9.51508506382702,0.292620752306052,
14.040758692588));
#20224=CARTESIAN_POINT('Ctrl Pts',(-9.51736327555368,-0.000704366368343423,
14.0545769675715));
#20225=CARTESIAN_POINT('Origin',(-8.5,0.,1.24542303242842));
#20226=CARTESIAN_POINT('',(-9.516475,5.65965774601236E-13,13.3954230324285));
#20227=CARTESIAN_POINT('',(-9.516475,5.92909588180802E-13,13.4545769675715));
#20228=CARTESIAN_POINT('',(-9.516475,1.78524650477582E-12,1.24542303242842));
#20229=CARTESIAN_POINT('Ctrl Pts',(-9.516475,5.65965774601236E-13,13.3954230324285));
#20230=CARTESIAN_POINT('Ctrl Pts',(-9.51647500000015,-0.265706620583383,
13.4079039656767));
#20231=CARTESIAN_POINT('Ctrl Pts',(-9.40727465387226,-0.529786878176597,
13.4203848989248));
#20232=CARTESIAN_POINT('Ctrl Pts',(-9.21961691907799,-0.71789478017443,
13.432865832173));
#20233=CARTESIAN_POINT('Ctrl Pts',(-9.03195918428372,-0.906002682172264,
13.4453467654212));
#20234=CARTESIAN_POINT('Ctrl Pts',(-8.76814132834418,-1.01583545019898,
13.4578276986694));
#20235=CARTESIAN_POINT('Ctrl Pts',(-8.50243547044545,-1.0164720823066,13.4703086319176));
#20236=CARTESIAN_POINT('Ctrl Pts',(-8.23672961254671,-1.01710871441422,
13.4827895651658));
#20237=CARTESIAN_POINT('Ctrl Pts',(-7.97238846933374,-0.908541417082982,
13.495270498414));
#20238=CARTESIAN_POINT('Ctrl Pts',(-7.78383148002372,-0.721334926798906,
13.5077514316622));
#20239=CARTESIAN_POINT('Ctrl Pts',(-7.59527449071369,-0.53412843651483,
13.5202323649104));
#20240=CARTESIAN_POINT('Ctrl Pts',(-7.48480993131717,-0.270574496756232,
13.5327132981586));
#20241=CARTESIAN_POINT('Ctrl Pts',(-7.48353667075686,-0.00487092690876391,
13.5451942314067));
#20242=CARTESIAN_POINT('Ctrl Pts',(-7.48226341019655,0.260832642938704,
13.5576751646549));
#20243=CARTESIAN_POINT('Ctrl Pts',(-7.59019703546723,0.52543315423994,13.5701560979031));
#20244=CARTESIAN_POINT('Ctrl Pts',(-7.77695120652479,0.714438148392872,
13.5826370311513));
#20245=CARTESIAN_POINT('Ctrl Pts',(-7.96370537758234,0.903443142545804,
13.5951179643995));
#20246=CARTESIAN_POINT('Ctrl Pts',(-8.22699388814769,1.01453885915643,13.6075988976477));
#20247=CARTESIAN_POINT('Ctrl Pts',(-8.49269364459097,1.01644874085988,13.6200798308959));
#20248=CARTESIAN_POINT('Ctrl Pts',(-8.75839340103426,1.01835862256333,13.6325607641441));
#20249=CARTESIAN_POINT('Ctrl Pts',(-9.02325176140329,0.911059288979315,
13.6450416973923));
#20250=CARTESIAN_POINT('Ctrl Pts',(-9.21270367535793,0.724758509267943,
13.6575226306405));
#20251=CARTESIAN_POINT('Ctrl Pts',(-9.40215558931258,0.538457729556571,
13.6700035638886));
#20252=CARTESIAN_POINT('Ctrl Pts',(-9.51388182535823,0.275436159672998,
13.6824844971368));
#20253=CARTESIAN_POINT('Ctrl Pts',(-9.51642831724057,0.00974174196491706,
13.694965430385));
#20254=CARTESIAN_POINT('Ctrl Pts',(-9.51645943884197,0.00649459406717135,
13.6951179643995));
#20255=CARTESIAN_POINT('Ctrl Pts',(-9.516475,0.0032472970341079,13.695270498414));
#20256=CARTESIAN_POINT('Ctrl Pts',(-9.516475,5.87882206992221E-13,13.6954230324285));
#20257=CARTESIAN_POINT('Ctrl Pts',(-9.516475,6.21799545274072E-13,13.4545769675715));
#20258=CARTESIAN_POINT('Ctrl Pts',(-9.51647500000016,-0.265706620583337,
13.4670579008197));
#20259=CARTESIAN_POINT('Ctrl Pts',(-9.40727465387229,-0.529786878176566,
13.4795388340679));
#20260=CARTESIAN_POINT('Ctrl Pts',(-9.21961691907801,-0.717894780174411,
13.4920197673161));
#20261=CARTESIAN_POINT('Ctrl Pts',(-9.03195918428375,-0.90600268217225,
13.5045007005643));
#20262=CARTESIAN_POINT('Ctrl Pts',(-8.76814132834421,-1.01583545019897,
13.5169816338124));
#20263=CARTESIAN_POINT('Ctrl Pts',(-8.50243547044547,-1.0164720823066,13.5294625670606));
#20264=CARTESIAN_POINT('Ctrl Pts',(-8.23672961254674,-1.01710871441422,
13.5419435003088));
#20265=CARTESIAN_POINT('Ctrl Pts',(-7.97238846933377,-0.908541417082996,
13.554424433557));
#20266=CARTESIAN_POINT('Ctrl Pts',(-7.78383148002374,-0.721334926798925,
13.5669053668052));
#20267=CARTESIAN_POINT('Ctrl Pts',(-7.59527449071371,-0.534128436514854,
13.5793863000534));
#20268=CARTESIAN_POINT('Ctrl Pts',(-7.48480993131717,-0.270574496756259,
13.5918672333016));
#20269=CARTESIAN_POINT('Ctrl Pts',(-7.48353667075686,-0.00487092690879085,
13.6043481665498));
#20270=CARTESIAN_POINT('Ctrl Pts',(-7.48226341019654,0.260832642938677,
13.616829099798));
#20271=CARTESIAN_POINT('Ctrl Pts',(-7.59019703546722,0.525433154239916,
13.6293100330461));
#20272=CARTESIAN_POINT('Ctrl Pts',(-7.77695120652477,0.714438148392853,
13.6417909662943));
#20273=CARTESIAN_POINT('Ctrl Pts',(-7.96370537758231,0.90344314254579,13.6542718995425));
#20274=CARTESIAN_POINT('Ctrl Pts',(-8.22699388814766,1.01453885915642,13.6667528327907));
#20275=CARTESIAN_POINT('Ctrl Pts',(-8.49269364459095,1.01644874085988,13.6792337660389));
#20276=CARTESIAN_POINT('Ctrl Pts',(-8.75839340103423,1.01835862256334,13.6917146992871));
#20277=CARTESIAN_POINT('Ctrl Pts',(-9.02325176140327,0.911059288979329,
13.7041956325353));
#20278=CARTESIAN_POINT('Ctrl Pts',(-9.21270367535791,0.724758509267962,
13.7166765657835));
#20279=CARTESIAN_POINT('Ctrl Pts',(-9.40215558931256,0.538457729556595,
13.7291574990317));
#20280=CARTESIAN_POINT('Ctrl Pts',(-9.51388182535822,0.275436159673025,
13.7416384322799));
#20281=CARTESIAN_POINT('Ctrl Pts',(-9.51642831724057,0.009741741964944,
13.754119365528));
#20282=CARTESIAN_POINT('Ctrl Pts',(-9.51645943884197,0.00649459406721755,
13.7542718995425));
#20283=CARTESIAN_POINT('Ctrl Pts',(-9.516475,0.0032472970341734,13.754424433557));
#20284=CARTESIAN_POINT('Ctrl Pts',(-9.516475,6.72605934758328E-13,13.7545769675715));
#20285=CARTESIAN_POINT('Origin',(-8.5,0.,1.24542303242842));
#20286=CARTESIAN_POINT('',(-9.516475,5.44049342210251E-13,13.0954230324285));
#20287=CARTESIAN_POINT('',(-9.516475,5.70993155789817E-13,13.1545769675715));
#20288=CARTESIAN_POINT('',(-9.516475,1.78524650477582E-12,1.24542303242842));
#20289=CARTESIAN_POINT('Ctrl Pts',(-9.516475,5.72939299303521E-13,13.0954230324285));
#20290=CARTESIAN_POINT('Ctrl Pts',(-9.51647500000015,-0.265706620583386,
13.1079039656767));
#20291=CARTESIAN_POINT('Ctrl Pts',(-9.40727465387226,-0.52978687817661,
13.1203848989248));
#20292=CARTESIAN_POINT('Ctrl Pts',(-9.21961691907798,-0.717894780174446,
13.132865832173));
#20293=CARTESIAN_POINT('Ctrl Pts',(-9.0319591842837,-0.906002682172282,
13.1453467654212));
#20294=CARTESIAN_POINT('Ctrl Pts',(-8.76814132834414,-1.01583545019899,
13.1578276986694));
#20295=CARTESIAN_POINT('Ctrl Pts',(-8.5024354704454,-1.0164720823066,13.1703086319176));
#20296=CARTESIAN_POINT('Ctrl Pts',(-8.23672961254665,-1.0171087144142,13.1827895651658));
#20297=CARTESIAN_POINT('Ctrl Pts',(-7.97238846933368,-0.908541417082948,
13.195270498414));
#20298=CARTESIAN_POINT('Ctrl Pts',(-7.78383148002366,-0.72133492679885,
13.2077514316622));
#20299=CARTESIAN_POINT('Ctrl Pts',(-7.59527449071365,-0.534128436514753,
13.2202323649104));
#20300=CARTESIAN_POINT('Ctrl Pts',(-7.48480993131714,-0.270574496756133,
13.2327132981586));
#20301=CARTESIAN_POINT('Ctrl Pts',(-7.48353667075686,-0.00487092690865533,
13.2451942314067));
#20302=CARTESIAN_POINT('Ctrl Pts',(-7.48226341019658,0.260832642938823,
13.2576751646549));
#20303=CARTESIAN_POINT('Ctrl Pts',(-7.5901970354673,0.525433154240057,13.2701560979031));
#20304=CARTESIAN_POINT('Ctrl Pts',(-7.77695120652488,0.71443814839297,13.2826370311513));
#20305=CARTESIAN_POINT('Ctrl Pts',(-7.96370537758247,0.903443142545883,
13.2951179643995));
#20306=CARTESIAN_POINT('Ctrl Pts',(-8.22699388814784,1.01453885915647,13.3075988976477));
#20307=CARTESIAN_POINT('Ctrl Pts',(-8.49269364459114,1.01644874085988,13.3200798308959));
#20308=CARTESIAN_POINT('Ctrl Pts',(-8.75839340103443,1.01835862256329,13.3325607641441));
#20309=CARTESIAN_POINT('Ctrl Pts',(-9.02325176140346,0.911059288979222,
13.3450416973923));
#20310=CARTESIAN_POINT('Ctrl Pts',(-9.21270367535807,0.724758509267806,
13.3575226306405));
#20311=CARTESIAN_POINT('Ctrl Pts',(-9.40215558931269,0.538457729556391,
13.3700035638887));
#20312=CARTESIAN_POINT('Ctrl Pts',(-9.51388182535829,0.275436159672784,
13.3824844971368));
#20313=CARTESIAN_POINT('Ctrl Pts',(-9.51642831724057,0.00974174196469292,
13.394965430385));
#20314=CARTESIAN_POINT('Ctrl Pts',(-9.51645943884197,0.00649459406701462,
13.3951179643995));
#20315=CARTESIAN_POINT('Ctrl Pts',(-9.516475,0.00324729703401863,13.395270498414));
#20316=CARTESIAN_POINT('Ctrl Pts',(-9.516475,5.65965774601236E-13,13.3954230324285));
#20317=CARTESIAN_POINT('Ctrl Pts',(-9.516475,6.28773069976357E-13,13.1545769675715));
#20318=CARTESIAN_POINT('Ctrl Pts',(-9.51647500000016,-0.26570662058334,
13.1670579008197));
#20319=CARTESIAN_POINT('Ctrl Pts',(-9.40727465387228,-0.529786878176579,
13.1795388340679));
#20320=CARTESIAN_POINT('Ctrl Pts',(-9.219616919078,-0.717894780174427,13.1920197673161));
#20321=CARTESIAN_POINT('Ctrl Pts',(-9.03195918428372,-0.906002682172275,
13.2045007005643));
#20322=CARTESIAN_POINT('Ctrl Pts',(-8.76814132834415,-1.01583545019899,
13.2169816338124));
#20323=CARTESIAN_POINT('Ctrl Pts',(-8.50243547044539,-1.0164720823066,13.2294625670606));
#20324=CARTESIAN_POINT('Ctrl Pts',(-8.23672961254664,-1.0171087144142,13.2419435003088));
#20325=CARTESIAN_POINT('Ctrl Pts',(-7.97238846933366,-0.908541417082939,
13.254424433557));
#20326=CARTESIAN_POINT('Ctrl Pts',(-7.78383148002364,-0.721334926798828,
13.2669053668052));
#20327=CARTESIAN_POINT('Ctrl Pts',(-7.59527449071362,-0.534128436514718,
13.2793863000534));
#20328=CARTESIAN_POINT('Ctrl Pts',(-7.48480993131712,-0.270574496756083,
13.2918672333016));
#20329=CARTESIAN_POINT('Ctrl Pts',(-7.48353667075686,-0.0048709269085956,
13.3043481665498));
#20330=CARTESIAN_POINT('Ctrl Pts',(-7.48226341019659,0.260832642938892,
13.316829099798));
#20331=CARTESIAN_POINT('Ctrl Pts',(-7.59019703546734,0.525433154240129,
13.3293100330462));
#20332=CARTESIAN_POINT('Ctrl Pts',(-7.77695120652494,0.714438148393033,
13.3417909662943));
#20333=CARTESIAN_POINT('Ctrl Pts',(-7.96370537758255,0.903443142545937,
13.3542718995425));
#20334=CARTESIAN_POINT('Ctrl Pts',(-8.22699388814795,1.0145388591565,13.3667528327907));
#20335=CARTESIAN_POINT('Ctrl Pts',(-8.49269364459126,1.01644874085988,13.3792337660389));
#20336=CARTESIAN_POINT('Ctrl Pts',(-8.75839340103456,1.01835862256326,13.3917146992871));
#20337=CARTESIAN_POINT('Ctrl Pts',(-9.02325176140358,0.911059288979153,
13.4041956325353));
#20338=CARTESIAN_POINT('Ctrl Pts',(-9.21270367535818,0.724758509267703,
13.4166765657835));
#20339=CARTESIAN_POINT('Ctrl Pts',(-9.40215558931277,0.538457729556254,
13.4291574990317));
#20340=CARTESIAN_POINT('Ctrl Pts',(-9.51388182535834,0.275436159672619,
13.4416384322799));
#20341=CARTESIAN_POINT('Ctrl Pts',(-9.51642831724057,0.00974174196451764,
13.4541193655281));
#20342=CARTESIAN_POINT('Ctrl Pts',(-9.51645943884197,0.00649459406691637,
13.4542718995425));
#20343=CARTESIAN_POINT('Ctrl Pts',(-9.516475,0.00324729703399743,13.454424433557));
#20344=CARTESIAN_POINT('Ctrl Pts',(-9.516475,6.21799545274072E-13,13.4545769675715));
#20345=CARTESIAN_POINT('Origin',(-8.5,0.,1.24542303242842));
#20346=CARTESIAN_POINT('',(-9.51612357761841,0.000116121315980709,12.7954230324285));
#20347=CARTESIAN_POINT('',(-9.516475,5.49076723398832E-13,12.8545769675715));
#20348=CARTESIAN_POINT('',(-9.516475,1.78524650477582E-12,1.24542303242842));
#20349=CARTESIAN_POINT('Ctrl Pts',(-9.516475,5.22132909819266E-13,12.7954230324285));
#20350=CARTESIAN_POINT('Ctrl Pts',(-9.51647500000014,-0.265706620583447,
12.8079039656767));
#20351=CARTESIAN_POINT('Ctrl Pts',(-9.40727465387222,-0.529786878176674,
12.8203848989249));
#20352=CARTESIAN_POINT('Ctrl Pts',(-9.21961691907792,-0.717894780174502,
12.832865832173));
#20353=CARTESIAN_POINT('Ctrl Pts',(-9.03195918428362,-0.906002682172331,
12.8453467654212));
#20354=CARTESIAN_POINT('Ctrl Pts',(-8.76814132834404,-1.01583545019902,
12.8578276986694));
#20355=CARTESIAN_POINT('Ctrl Pts',(-8.50243547044529,-1.0164720823066,12.8703086319176));
#20356=CARTESIAN_POINT('Ctrl Pts',(-8.23672961254653,-1.01710871441417,
12.8827895651658));
#20357=CARTESIAN_POINT('Ctrl Pts',(-7.97238846933356,-0.908541417082883,
12.895270498414));
#20358=CARTESIAN_POINT('Ctrl Pts',(-7.78383148002357,-0.721334926798753,
12.9077514316622));
#20359=CARTESIAN_POINT('Ctrl Pts',(-7.59527449071357,-0.534128436514623,
12.9202323649104));
#20360=CARTESIAN_POINT('Ctrl Pts',(-7.48480993131709,-0.270574496755977,
12.9327132981586));
#20361=CARTESIAN_POINT('Ctrl Pts',(-7.48353667075686,-0.00487092690848896,
12.9451942314068));
#20362=CARTESIAN_POINT('Ctrl Pts',(-7.48226341019662,0.260832642938999,
12.9576751646549));
#20363=CARTESIAN_POINT('Ctrl Pts',(-7.59019703546739,0.525433154240224,
12.9701560979031));
#20364=CARTESIAN_POINT('Ctrl Pts',(-7.77695120652502,0.714438148393109,
12.9826370311513));
#20365=CARTESIAN_POINT('Ctrl Pts',(-7.96370537758265,0.903443142545993,
12.9951179643995));
#20366=CARTESIAN_POINT('Ctrl Pts',(-8.22699388814806,1.01453885915653,13.0075988976477));
#20367=CARTESIAN_POINT('Ctrl Pts',(-8.49269364459136,1.01644874085988,13.0200798308959));
#20368=CARTESIAN_POINT('Ctrl Pts',(-8.75839340103467,1.01835862256324,13.0325607641441));
#20369=CARTESIAN_POINT('Ctrl Pts',(-9.02325176140368,0.911059288979098,
13.0450416973923));
#20370=CARTESIAN_POINT('Ctrl Pts',(-9.21270367535825,0.724758509267629,
13.0575226306405));
#20371=CARTESIAN_POINT('Ctrl Pts',(-9.40215558931283,0.538457729556159,
13.0700035638887));
#20372=CARTESIAN_POINT('Ctrl Pts',(-9.51388182535837,0.275436159672512,
13.0824844971369));
#20373=CARTESIAN_POINT('Ctrl Pts',(-9.51642831724057,0.00974174196441101,
13.094965430385));
#20374=CARTESIAN_POINT('Ctrl Pts',(-9.51645943884197,0.00649459406682899,
13.0951179643995));
#20375=CARTESIAN_POINT('Ctrl Pts',(-9.516475,0.00324729703392927,13.095270498414));
#20376=CARTESIAN_POINT('Ctrl Pts',(-9.516475,5.72939299303521E-13,13.0954230324285));
#20377=CARTESIAN_POINT('Ctrl Pts',(-9.516475,5.20186766305562E-13,12.8545769675715));
#20378=CARTESIAN_POINT('Ctrl Pts',(-9.51647500000014,-0.265706620583449,
12.8670579008197));
#20379=CARTESIAN_POINT('Ctrl Pts',(-9.40727465387222,-0.529786878176676,
12.8795388340679));
#20380=CARTESIAN_POINT('Ctrl Pts',(-9.21961691907792,-0.717894780174504,
12.8920197673161));
#20381=CARTESIAN_POINT('Ctrl Pts',(-9.03195918428362,-0.906002682172331,
12.9045007005643));
#20382=CARTESIAN_POINT('Ctrl Pts',(-8.76814132834404,-1.01583545019902,
12.9169816338124));
#20383=CARTESIAN_POINT('Ctrl Pts',(-8.50243547044529,-1.0164720823066,12.9294625670606));
#20384=CARTESIAN_POINT('Ctrl Pts',(-8.23672961254653,-1.01710871441417,
12.9419435003088));
#20385=CARTESIAN_POINT('Ctrl Pts',(-7.97238846933356,-0.908541417082882,
12.954424433557));
#20386=CARTESIAN_POINT('Ctrl Pts',(-7.78383148002356,-0.721334926798752,
12.9669053668052));
#20387=CARTESIAN_POINT('Ctrl Pts',(-7.59527449071357,-0.534128436514622,
12.9793863000534));
#20388=CARTESIAN_POINT('Ctrl Pts',(-7.48480993131709,-0.270574496755975,
12.9918672333016));
#20389=CARTESIAN_POINT('Ctrl Pts',(-7.48353667075686,-0.00487092690848702,
13.0043481665498));
#20390=CARTESIAN_POINT('Ctrl Pts',(-7.48226341019662,0.260832642939001,
13.016829099798));
#20391=CARTESIAN_POINT('Ctrl Pts',(-7.59019703546739,0.525433154240226,
13.0293100330462));
#20392=CARTESIAN_POINT('Ctrl Pts',(-7.77695120652502,0.71443814839311,13.0417909662944));
#20393=CARTESIAN_POINT('Ctrl Pts',(-7.96370537758265,0.903443142545994,
13.0542718995425));
#20394=CARTESIAN_POINT('Ctrl Pts',(-8.22699388814806,1.01453885915653,13.0667528327907));
#20395=CARTESIAN_POINT('Ctrl Pts',(-8.49269364459136,1.01644874085988,13.0792337660389));
#20396=CARTESIAN_POINT('Ctrl Pts',(-8.75839340103467,1.01835862256323,13.0917146992871));
#20397=CARTESIAN_POINT('Ctrl Pts',(-9.02325176140368,0.911059288979097,
13.1041956325353));
#20398=CARTESIAN_POINT('Ctrl Pts',(-9.21270367535826,0.724758509267627,
13.1166765657835));
#20399=CARTESIAN_POINT('Ctrl Pts',(-9.40215558931283,0.538457729556157,
13.1291574990317));
#20400=CARTESIAN_POINT('Ctrl Pts',(-9.51388182535837,0.27543615967251,13.1416384322799));
#20401=CARTESIAN_POINT('Ctrl Pts',(-9.51642831724057,0.00974174196440906,
13.1541193655281));
#20402=CARTESIAN_POINT('Ctrl Pts',(-9.51645943884197,0.0064945940668463,
13.1542718995425));
#20403=CARTESIAN_POINT('Ctrl Pts',(-9.516475,0.00324729703396589,13.154424433557));
#20404=CARTESIAN_POINT('Ctrl Pts',(-9.516475,6.28773069976357E-13,13.1545769675715));
#20405=CARTESIAN_POINT('Origin',(-8.5,0.,1.24542303242842));
#20406=CARTESIAN_POINT('',(-9.51653950885578,4.27590676786889E-5,12.4954230324285));
#20407=CARTESIAN_POINT('',(-9.516475,5.27160291007847E-13,12.5545769675715));
#20408=CARTESIAN_POINT('',(-9.516475,1.78524650477582E-12,1.24542303242842));
#20409=CARTESIAN_POINT('Ctrl Pts',(-9.51746434211765,0.000655775794156509,
12.4954230324285));
#20410=CARTESIAN_POINT('Ctrl Pts',(-9.51527198270641,-0.296676988704239,
12.5094337807337));
#20411=CARTESIAN_POINT('Ctrl Pts',(-9.22128580559795,-0.935436405005595,
12.5393518701905));
#20412=CARTESIAN_POINT('Ctrl Pts',(-8.13336992371389,-1.14538460256293,
12.5851773007989));
#20413=CARTESIAN_POINT('Ctrl Pts',(-7.47298807192611,-0.450463593150824,
12.6249456536779));
#20414=CARTESIAN_POINT('Ctrl Pts',(-7.47295403032462,0.248558970813969,
12.6567603359812));
#20415=CARTESIAN_POINT('Ctrl Pts',(-7.79260946040346,0.87021237272846,12.6885750182844));
#20416=CARTESIAN_POINT('Ctrl Pts',(-8.69766342022542,1.1862768112589,12.7283433711635));
#20417=CARTESIAN_POINT('Ctrl Pts',(-9.42544752600762,0.614958176341259,
12.7666105994034));
#20418=CARTESIAN_POINT('Ctrl Pts',(-9.51577746299321,0.138234549146154,
12.7889704864918));
#20419=CARTESIAN_POINT('Ctrl Pts',(-9.51510940460441,0.00045123686540878,
12.7954230324285));
#20420=CARTESIAN_POINT('Ctrl Pts',(-9.516475,5.84940205194387E-13,12.5545769675715));
#20421=CARTESIAN_POINT('Ctrl Pts',(-9.51647500000015,-0.265706620583384,
12.5670579008197));
#20422=CARTESIAN_POINT('Ctrl Pts',(-9.40727465387226,-0.529786878176618,
12.5795388340679));
#20423=CARTESIAN_POINT('Ctrl Pts',(-9.21961691907797,-0.717894780174458,
12.5920197673161));
#20424=CARTESIAN_POINT('Ctrl Pts',(-9.03195918428368,-0.906002682172298,
12.6045007005643));
#20425=CARTESIAN_POINT('Ctrl Pts',(-8.7681413283441,-1.015835450199,12.6169816338124));
#20426=CARTESIAN_POINT('Ctrl Pts',(-8.50243547044535,-1.0164720823066,12.6294625670606));
#20427=CARTESIAN_POINT('Ctrl Pts',(-8.2367296125466,-1.01710871441419,12.6419435003088));
#20428=CARTESIAN_POINT('Ctrl Pts',(-7.97238846933362,-0.908541417082916,
12.654424433557));
#20429=CARTESIAN_POINT('Ctrl Pts',(-7.78383148002361,-0.721334926798798,
12.6669053668052));
#20430=CARTESIAN_POINT('Ctrl Pts',(-7.5952744907136,-0.534128436514679,
12.6793863000534));
#20431=CARTESIAN_POINT('Ctrl Pts',(-7.48480993131711,-0.27057449675604,
12.6918672333016));
#20432=CARTESIAN_POINT('Ctrl Pts',(-7.48353667075686,-0.00487092690855177,
12.7043481665498));
#20433=CARTESIAN_POINT('Ctrl Pts',(-7.48226341019661,0.260832642938936,
12.716829099798));
#20434=CARTESIAN_POINT('Ctrl Pts',(-7.59019703546736,0.525433154240168,
12.7293100330462));
#20435=CARTESIAN_POINT('Ctrl Pts',(-7.77695120652497,0.714438148393064,
12.7417909662943));
#20436=CARTESIAN_POINT('Ctrl Pts',(-7.96370537758259,0.90344314254596,12.7542718995425));
#20437=CARTESIAN_POINT('Ctrl Pts',(-8.22699388814799,1.01453885915651,12.7667528327907));
#20438=CARTESIAN_POINT('Ctrl Pts',(-8.4926936445913,1.01644874085988,12.7792337660389));
#20439=CARTESIAN_POINT('Ctrl Pts',(-8.7583934010346,1.01835862256325,12.7917146992871));
#20440=CARTESIAN_POINT('Ctrl Pts',(-9.02325176140362,0.91105928897913,12.8041956325353));
#20441=CARTESIAN_POINT('Ctrl Pts',(-9.21270367535821,0.724758509267673,
12.8166765657835));
#20442=CARTESIAN_POINT('Ctrl Pts',(-9.4021555893128,0.538457729556215,12.8291574990317));
#20443=CARTESIAN_POINT('Ctrl Pts',(-9.51388182535835,0.275436159672575,
12.8416384322799));
#20444=CARTESIAN_POINT('Ctrl Pts',(-9.51642831724057,0.00974174196447381,
12.8541193655281));
#20445=CARTESIAN_POINT('Ctrl Pts',(-9.51645943884197,0.00649459406685328,
12.8542718995425));
#20446=CARTESIAN_POINT('Ctrl Pts',(-9.516475,0.00324729703391504,12.854424433557));
#20447=CARTESIAN_POINT('Ctrl Pts',(-9.516475,5.20186766305562E-13,12.8545769675715));
#20448=CARTESIAN_POINT('Origin',(-8.5,0.,1.24542303242842));
#20449=CARTESIAN_POINT('',(-9.516475,4.78300045037296E-13,12.1954230324285));
#20450=CARTESIAN_POINT('',(-9.516475,5.05243858616862E-13,12.2545769675715));
#20451=CARTESIAN_POINT('',(-9.516475,1.78524650477582E-12,1.24542303242842));
#20452=CARTESIAN_POINT('Ctrl Pts',(-9.516475,4.78300045037296E-13,12.1954230324285));
#20453=CARTESIAN_POINT('Ctrl Pts',(-9.51647500000012,-0.265706620583481,
12.2079039656767));
#20454=CARTESIAN_POINT('Ctrl Pts',(-9.40727465387221,-0.529786878176695,
12.2203848989249));
#20455=CARTESIAN_POINT('Ctrl Pts',(-9.21961691907791,-0.717894780174513,
12.232865832173));
#20456=CARTESIAN_POINT('Ctrl Pts',(-9.03195918428361,-0.906002682172331,
12.2453467654212));
#20457=CARTESIAN_POINT('Ctrl Pts',(-8.76814132834405,-1.01583545019902,
12.2578276986694));
#20458=CARTESIAN_POINT('Ctrl Pts',(-8.5024354704453,-1.0164720823066,12.2703086319176));
#20459=CARTESIAN_POINT('Ctrl Pts',(-8.23672961254656,-1.01710871441418,
12.2827895651658));
#20460=CARTESIAN_POINT('Ctrl Pts',(-7.9723884693336,-0.908541417082899,
12.295270498414));
#20461=CARTESIAN_POINT('Ctrl Pts',(-7.7838314800236,-0.721334926798783,
12.3077514316622));
#20462=CARTESIAN_POINT('Ctrl Pts',(-7.5952744907136,-0.534128436514668,
12.3202323649104));
#20463=CARTESIAN_POINT('Ctrl Pts',(-7.48480993131711,-0.270574496756039,
12.3327132981586));
#20464=CARTESIAN_POINT('Ctrl Pts',(-7.48353667075686,-0.00487092690856069,
12.3451942314068));
#20465=CARTESIAN_POINT('Ctrl Pts',(-7.4822634101966,0.260832642938917,12.3576751646549));
#20466=CARTESIAN_POINT('Ctrl Pts',(-7.59019703546735,0.525433154240141,
12.3701560979031));
#20467=CARTESIAN_POINT('Ctrl Pts',(-7.77695120652495,0.714438148393037,
12.3826370311513));
#20468=CARTESIAN_POINT('Ctrl Pts',(-7.96370537758255,0.903443142545933,
12.3951179643995));
#20469=CARTESIAN_POINT('Ctrl Pts',(-8.22699388814794,1.0145388591565,12.4075988976477));
#20470=CARTESIAN_POINT('Ctrl Pts',(-8.49269364459123,1.01644874085988,12.4200798308959));
#20471=CARTESIAN_POINT('Ctrl Pts',(-8.75839340103453,1.01835862256327,12.4325607641441));
#20472=CARTESIAN_POINT('Ctrl Pts',(-9.02325176140354,0.911059288979173,
12.4450416973923));
#20473=CARTESIAN_POINT('Ctrl Pts',(-9.21270367535814,0.72475850926774,12.4575226306405));
#20474=CARTESIAN_POINT('Ctrl Pts',(-9.40215558931274,0.538457729556307,
12.4700035638887));
#20475=CARTESIAN_POINT('Ctrl Pts',(-9.51388182535831,0.275436159672689,
12.4824844971368));
#20476=CARTESIAN_POINT('Ctrl Pts',(-9.51642831724057,0.00974174196459828,
12.494965430385));
#20477=CARTESIAN_POINT('Ctrl Pts',(-9.51645943884197,0.00649459406691998,
12.4951179643995));
#20478=CARTESIAN_POINT('Ctrl Pts',(-9.516475,0.003247297033924,12.495270498414));
#20479=CARTESIAN_POINT('Ctrl Pts',(-9.516475,4.71326520335011E-13,12.4954230324285));
#20480=CARTESIAN_POINT('Ctrl Pts',(-9.516475,5.05243858616862E-13,12.2545769675715));
#20481=CARTESIAN_POINT('Ctrl Pts',(-9.51647500000013,-0.265706620583483,
12.2670579008197));
#20482=CARTESIAN_POINT('Ctrl Pts',(-9.4072746538722,-0.529786878176727,
12.2795388340679));
#20483=CARTESIAN_POINT('Ctrl Pts',(-9.21961691907787,-0.717894780174555,
12.2920197673161));
#20484=CARTESIAN_POINT('Ctrl Pts',(-9.03195918428354,-0.906002682172383,
12.3045007005643));
#20485=CARTESIAN_POINT('Ctrl Pts',(-8.76814132834393,-1.01583545019905,
12.3169816338125));
#20486=CARTESIAN_POINT('Ctrl Pts',(-8.50243547044516,-1.0164720823066,12.3294625670606));
#20487=CARTESIAN_POINT('Ctrl Pts',(-8.23672961254638,-1.01710871441414,
12.3419435003088));
#20488=CARTESIAN_POINT('Ctrl Pts',(-7.97238846933341,-0.908541417082798,
12.354424433557));
#20489=CARTESIAN_POINT('Ctrl Pts',(-7.78383148002343,-0.721334926798619,
12.3669053668052));
#20490=CARTESIAN_POINT('Ctrl Pts',(-7.59527449071345,-0.534128436514441,
12.3793863000534));
#20491=CARTESIAN_POINT('Ctrl Pts',(-7.48480993131703,-0.270574496755748,
12.3918672333016));
#20492=CARTESIAN_POINT('Ctrl Pts',(-7.48353667075686,-0.00487092690824096,
12.4043481665498));
#20493=CARTESIAN_POINT('Ctrl Pts',(-7.48226341019669,0.260832642939266,
12.416829099798));
#20494=CARTESIAN_POINT('Ctrl Pts',(-7.59019703546754,0.525433154240484,
12.4293100330462));
#20495=CARTESIAN_POINT('Ctrl Pts',(-7.77695120652523,0.714438148393326,
12.4417909662944));
#20496=CARTESIAN_POINT('Ctrl Pts',(-7.96370537758293,0.903443142546168,
12.4542718995426));
#20497=CARTESIAN_POINT('Ctrl Pts',(-8.2269938881484,1.01453885915663,12.4667528327907));
#20498=CARTESIAN_POINT('Ctrl Pts',(-8.49269364459172,1.01644874085989,12.4792337660389));
#20499=CARTESIAN_POINT('Ctrl Pts',(-8.75839340103505,1.01835862256314,12.4917146992871));
#20500=CARTESIAN_POINT('Ctrl Pts',(-9.02325176140404,0.911059288978894,
12.5041956325353));
#20501=CARTESIAN_POINT('Ctrl Pts',(-9.21270367535855,0.724758509267333,
12.5166765657835));
#20502=CARTESIAN_POINT('Ctrl Pts',(-9.40215558931307,0.538457729555772,
12.5291574990317));
#20503=CARTESIAN_POINT('Ctrl Pts',(-9.51388182535849,0.275436159672054,
12.5416384322799));
#20504=CARTESIAN_POINT('Ctrl Pts',(-9.51642831724057,0.0097417419639319,
12.5541193655281));
#20505=CARTESIAN_POINT('Ctrl Pts',(-9.51645943884197,0.00649459406651357,
12.5542718995426));
#20506=CARTESIAN_POINT('Ctrl Pts',(-9.516475,0.00324729703377759,12.554424433557));
#20507=CARTESIAN_POINT('Ctrl Pts',(-9.516475,5.84940205194387E-13,12.5545769675715));
#20508=CARTESIAN_POINT('Origin',(-8.5,0.,1.24542303242842));
#20509=CARTESIAN_POINT('',(-9.516475,4.5638361264631E-13,11.8954230324285));
#20510=CARTESIAN_POINT('',(-9.516475,4.83327426225877E-13,11.9545769675715));
#20511=CARTESIAN_POINT('',(-9.516475,1.78524650477582E-12,1.24542303242842));
#20512=CARTESIAN_POINT('Ctrl Pts',(-9.516475,4.2749365555304E-13,11.8954230324285));
#20513=CARTESIAN_POINT('Ctrl Pts',(-9.51647500000011,-0.265706620583551,
11.9079039656767));
#20514=CARTESIAN_POINT('Ctrl Pts',(-9.40727465387217,-0.529786878176778,
11.9203848989249));
#20515=CARTESIAN_POINT('Ctrl Pts',(-9.21961691907784,-0.71789478017459,
11.932865832173));
#20516=CARTESIAN_POINT('Ctrl Pts',(-9.0319591842835,-0.906002682172402,
11.9453467654212));
#20517=CARTESIAN_POINT('Ctrl Pts',(-8.7681413283439,-1.01583545019906,11.9578276986694));
#20518=CARTESIAN_POINT('Ctrl Pts',(-8.50243547044514,-1.0164720823066,11.9703086319176));
#20519=CARTESIAN_POINT('Ctrl Pts',(-8.23672961254637,-1.01710871441414,
11.9827895651658));
#20520=CARTESIAN_POINT('Ctrl Pts',(-7.97238846933341,-0.908541417082796,
11.995270498414));
#20521=CARTESIAN_POINT('Ctrl Pts',(-7.78383148002344,-0.721334926798626,
12.0077514316622));
#20522=CARTESIAN_POINT('Ctrl Pts',(-7.59527449071346,-0.534128436514455,
12.0202323649104));
#20523=CARTESIAN_POINT('Ctrl Pts',(-7.48480993131704,-0.270574496755776,
12.0327132981586));
#20524=CARTESIAN_POINT('Ctrl Pts',(-7.48353667075686,-0.00487092690827876,
12.0451942314068));
#20525=CARTESIAN_POINT('Ctrl Pts',(-7.48226341019668,0.260832642939219,
12.057675164655));
#20526=CARTESIAN_POINT('Ctrl Pts',(-7.59019703546751,0.525433154240432,
12.0701560979031));
#20527=CARTESIAN_POINT('Ctrl Pts',(-7.77695120652519,0.714438148393279,
12.0826370311513));
#20528=CARTESIAN_POINT('Ctrl Pts',(-7.96370537758286,0.903443142546126,
12.0951179643995));
#20529=CARTESIAN_POINT('Ctrl Pts',(-8.22699388814831,1.0145388591566,12.1075988976477));
#20530=CARTESIAN_POINT('Ctrl Pts',(-8.49269364459163,1.01644874085989,12.1200798308959));
#20531=CARTESIAN_POINT('Ctrl Pts',(-8.75839340103495,1.01835862256317,12.1325607641441));
#20532=CARTESIAN_POINT('Ctrl Pts',(-9.02325176140394,0.911059288978952,
12.1450416973923));
#20533=CARTESIAN_POINT('Ctrl Pts',(-9.21270367535847,0.72475850926742,12.1575226306405));
#20534=CARTESIAN_POINT('Ctrl Pts',(-9.40215558931299,0.538457729555889,
12.1700035638887));
#20535=CARTESIAN_POINT('Ctrl Pts',(-9.51388182535845,0.275436159672197,
12.1824844971369));
#20536=CARTESIAN_POINT('Ctrl Pts',(-9.51642831724057,0.00974174196408526,
12.1949654303851));
#20537=CARTESIAN_POINT('Ctrl Pts',(-9.51645943884197,0.00649459406658027,
12.1951179643995));
#20538=CARTESIAN_POINT('Ctrl Pts',(-9.516475,0.00324729703375759,12.195270498414));
#20539=CARTESIAN_POINT('Ctrl Pts',(-9.516475,4.78300045037296E-13,12.1954230324285));
#20540=CARTESIAN_POINT('Ctrl Pts',(-9.516475,5.12217383319147E-13,11.9545769675715));
#20541=CARTESIAN_POINT('Ctrl Pts',(-9.51647500000013,-0.265706620583457,
11.9670579008197));
#20542=CARTESIAN_POINT('Ctrl Pts',(-9.40727465387222,-0.529786878176683,
11.9795388340679));
#20543=CARTESIAN_POINT('Ctrl Pts',(-9.21961691907792,-0.717894780174509,
11.9920197673161));
#20544=CARTESIAN_POINT('Ctrl Pts',(-9.03195918428361,-0.906002682172336,
12.0045007005643));
#20545=CARTESIAN_POINT('Ctrl Pts',(-8.76814132834403,-1.01583545019902,
12.0169816338125));
#20546=CARTESIAN_POINT('Ctrl Pts',(-8.50243547044528,-1.0164720823066,12.0294625670606));
#20547=CARTESIAN_POINT('Ctrl Pts',(-8.23672961254653,-1.01710871441417,
12.0419435003088));
#20548=CARTESIAN_POINT('Ctrl Pts',(-7.97238846933355,-0.908541417082878,
12.054424433557));
#20549=CARTESIAN_POINT('Ctrl Pts',(-7.78383148002356,-0.721334926798746,
12.0669053668052));
#20550=CARTESIAN_POINT('Ctrl Pts',(-7.59527449071356,-0.534128436514615,
12.0793863000534));
#20551=CARTESIAN_POINT('Ctrl Pts',(-7.48480993131709,-0.270574496755967,
12.0918672333016));
#20552=CARTESIAN_POINT('Ctrl Pts',(-7.48353667075686,-0.00487092690847905,
12.1043481665498));
#20553=CARTESIAN_POINT('Ctrl Pts',(-7.48226341019662,0.260832642939009,
12.116829099798));
#20554=CARTESIAN_POINT('Ctrl Pts',(-7.5901970354674,0.525433154240233,12.1293100330462));
#20555=CARTESIAN_POINT('Ctrl Pts',(-7.77695120652503,0.714438148393116,
12.1417909662944));
#20556=CARTESIAN_POINT('Ctrl Pts',(-7.96370537758265,0.903443142545999,
12.1542718995425));
#20557=CARTESIAN_POINT('Ctrl Pts',(-8.22699388814807,1.01453885915653,12.1667528327907));
#20558=CARTESIAN_POINT('Ctrl Pts',(-8.49269364459137,1.01644874085988,12.1792337660389));
#20559=CARTESIAN_POINT('Ctrl Pts',(-8.75839340103468,1.01835862256323,12.1917146992871));
#20560=CARTESIAN_POINT('Ctrl Pts',(-9.02325176140369,0.911059288979093,
12.2041956325353));
#20561=CARTESIAN_POINT('Ctrl Pts',(-9.21270367535826,0.724758509267622,
12.2166765657835));
#20562=CARTESIAN_POINT('Ctrl Pts',(-9.40215558931283,0.53845772955615,12.2291574990317));
#20563=CARTESIAN_POINT('Ctrl Pts',(-9.51388182535837,0.275436159672502,
12.2416384322799));
#20564=CARTESIAN_POINT('Ctrl Pts',(-9.51642831724057,0.00974174196440109,
12.2541193655281));
#20565=CARTESIAN_POINT('Ctrl Pts',(-9.51645943884197,0.00649459406679982,
12.2542718995425));
#20566=CARTESIAN_POINT('Ctrl Pts',(-9.516475,0.00324729703388088,12.254424433557));
#20567=CARTESIAN_POINT('Ctrl Pts',(-9.516475,5.05243858616862E-13,12.2545769675715));
#20568=CARTESIAN_POINT('Origin',(-8.5,0.,1.24542303242842));
#20569=CARTESIAN_POINT('',(-9.516475,4.34467180255325E-13,11.5954230324285));
#20570=CARTESIAN_POINT('',(-9.516475,4.61410993834892E-13,11.6545769675715));
#20571=CARTESIAN_POINT('',(-9.516475,1.78524650477582E-12,1.24542303242842));
#20572=CARTESIAN_POINT('Ctrl Pts',(-9.516475,4.63357137348595E-13,11.5954230324285));
#20573=CARTESIAN_POINT('Ctrl Pts',(-9.51647500000012,-0.265706620583515,
11.6079039656767));
#20574=CARTESIAN_POINT('Ctrl Pts',(-9.40727465387219,-0.529786878176746,
11.6203848989249));
#20575=CARTESIAN_POINT('Ctrl Pts',(-9.21961691907786,-0.717894780174565,
11.632865832173));
#20576=CARTESIAN_POINT('Ctrl Pts',(-9.03195918428354,-0.906002682172383,
11.6453467654212));
#20577=CARTESIAN_POINT('Ctrl Pts',(-8.76814132834394,-1.01583545019905,
11.6578276986694));
#20578=CARTESIAN_POINT('Ctrl Pts',(-8.50243547044517,-1.0164720823066,11.6703086319176));
#20579=CARTESIAN_POINT('Ctrl Pts',(-8.23672961254641,-1.01710871441414,
11.6827895651658));
#20580=CARTESIAN_POINT('Ctrl Pts',(-7.97238846933344,-0.908541417082815,
11.695270498414));
#20581=CARTESIAN_POINT('Ctrl Pts',(-7.78383148002346,-0.721334926798651,
11.7077514316622));
#20582=CARTESIAN_POINT('Ctrl Pts',(-7.59527449071348,-0.534128436514487,
11.7202323649104));
#20583=CARTESIAN_POINT('Ctrl Pts',(-7.48480993131705,-0.270574496755812,
11.7327132981586));
#20584=CARTESIAN_POINT('Ctrl Pts',(-7.48353667075686,-0.00487092690831463,
11.7451942314068));
#20585=CARTESIAN_POINT('Ctrl Pts',(-7.48226341019667,0.260832642939183,
11.757675164655));
#20586=CARTESIAN_POINT('Ctrl Pts',(-7.59019703546749,0.525433154240399,
11.7701560979031));
#20587=CARTESIAN_POINT('Ctrl Pts',(-7.77695120652516,0.714438148393253,
11.7826370311513));
#20588=CARTESIAN_POINT('Ctrl Pts',(-7.96370537758283,0.903443142546107,
11.7951179643995));
#20589=CARTESIAN_POINT('Ctrl Pts',(-8.22699388814828,1.01453885915659,11.8075988976477));
#20590=CARTESIAN_POINT('Ctrl Pts',(-8.49269364459159,1.01644874085989,11.8200798308959));
#20591=CARTESIAN_POINT('Ctrl Pts',(-8.75839340103491,1.01835862256318,11.8325607641441));
#20592=CARTESIAN_POINT('Ctrl Pts',(-9.02325176140391,0.91105928897897,11.8450416973923));
#20593=CARTESIAN_POINT('Ctrl Pts',(-9.21270367535844,0.724758509267446,
11.8575226306405));
#20594=CARTESIAN_POINT('Ctrl Pts',(-9.40215558931297,0.538457729555921,
11.8700035638887));
#20595=CARTESIAN_POINT('Ctrl Pts',(-9.51388182535844,0.275436159672233,
11.8824844971369));
#20596=CARTESIAN_POINT('Ctrl Pts',(-9.51642831724057,0.00974174196412112,
11.8949654303851));
#20597=CARTESIAN_POINT('Ctrl Pts',(-9.51645943884197,0.00649459406658725,
11.8951179643995));
#20598=CARTESIAN_POINT('Ctrl Pts',(-9.516475,0.0032472970337357,11.895270498414));
#20599=CARTESIAN_POINT('Ctrl Pts',(-9.516475,4.2749365555304E-13,11.8954230324285));
#20600=CARTESIAN_POINT('Ctrl Pts',(-9.516475,4.61410993834892E-13,11.6545769675715));
#20601=CARTESIAN_POINT('Ctrl Pts',(-9.51647500000012,-0.265706620583517,
11.6670579008197));
#20602=CARTESIAN_POINT('Ctrl Pts',(-9.40727465387218,-0.529786878176748,
11.6795388340679));
#20603=CARTESIAN_POINT('Ctrl Pts',(-9.21961691907786,-0.717894780174566,
11.6920197673161));
#20604=CARTESIAN_POINT('Ctrl Pts',(-9.03195918428353,-0.906002682172384,
11.7045007005643));
#20605=CARTESIAN_POINT('Ctrl Pts',(-8.76814132834393,-1.01583545019905,
11.7169816338125));
#20606=CARTESIAN_POINT('Ctrl Pts',(-8.50243547044517,-1.0164720823066,11.7294625670606));
#20607=CARTESIAN_POINT('Ctrl Pts',(-8.23672961254641,-1.01710871441414,
11.7419435003088));
#20608=CARTESIAN_POINT('Ctrl Pts',(-7.97238846933344,-0.908541417082814,
11.754424433557));
#20609=CARTESIAN_POINT('Ctrl Pts',(-7.78383148002346,-0.72133492679865,
11.7669053668052));
#20610=CARTESIAN_POINT('Ctrl Pts',(-7.59527449071348,-0.534128436514485,
11.7793863000534));
#20611=CARTESIAN_POINT('Ctrl Pts',(-7.48480993131705,-0.27057449675581,
11.7918672333016));
#20612=CARTESIAN_POINT('Ctrl Pts',(-7.48353667075686,-0.00487092690831268,
11.8043481665498));
#20613=CARTESIAN_POINT('Ctrl Pts',(-7.48226341019667,0.260832642939185,
11.816829099798));
#20614=CARTESIAN_POINT('Ctrl Pts',(-7.59019703546749,0.525433154240401,
11.8293100330462));
#20615=CARTESIAN_POINT('Ctrl Pts',(-7.77695120652516,0.714438148393255,
11.8417909662944));
#20616=CARTESIAN_POINT('Ctrl Pts',(-7.96370537758284,0.903443142546108,
11.8542718995426));
#20617=CARTESIAN_POINT('Ctrl Pts',(-8.22699388814828,1.01453885915659,11.8667528327907));
#20618=CARTESIAN_POINT('Ctrl Pts',(-8.4926936445916,1.01644874085989,11.8792337660389));
#20619=CARTESIAN_POINT('Ctrl Pts',(-8.75839340103491,1.01835862256318,11.8917146992871));
#20620=CARTESIAN_POINT('Ctrl Pts',(-9.02325176140391,0.911059288978969,
11.9041956325353));
#20621=CARTESIAN_POINT('Ctrl Pts',(-9.21270367535844,0.724758509267444,
11.9166765657835));
#20622=CARTESIAN_POINT('Ctrl Pts',(-9.40215558931298,0.538457729555919,
11.9291574990317));
#20623=CARTESIAN_POINT('Ctrl Pts',(-9.51388182535845,0.275436159672231,
11.9416384322799));
#20624=CARTESIAN_POINT('Ctrl Pts',(-9.51642831724057,0.00974174196411918,
11.9541193655281));
#20625=CARTESIAN_POINT('Ctrl Pts',(-9.51645943884197,0.00649459406661419,
11.9542718995426));
#20626=CARTESIAN_POINT('Ctrl Pts',(-9.516475,0.00324729703379151,11.954424433557));
#20627=CARTESIAN_POINT('Ctrl Pts',(-9.516475,5.12217383319147E-13,11.9545769675715));
#20628=CARTESIAN_POINT('Origin',(-8.5,0.,1.24542303242842));
#20629=CARTESIAN_POINT('',(-9.51672394194905,-5.37065327258883E-5,11.2954230324285));
#20630=CARTESIAN_POINT('',(-9.516475,4.39494561443907E-13,11.3545769675715));
#20631=CARTESIAN_POINT('',(-9.516475,1.78524650477582E-12,1.24542303242842));
#20632=CARTESIAN_POINT('Ctrl Pts',(-9.516475,4.4144070495761E-13,11.2954230324285));
#20633=CARTESIAN_POINT('Ctrl Pts',(-9.51647500000012,-0.265706620583537,
11.3079039656767));
#20634=CARTESIAN_POINT('Ctrl Pts',(-9.40727465387217,-0.529786878176765,
11.3203848989249));
#20635=CARTESIAN_POINT('Ctrl Pts',(-9.21961691907785,-0.71789478017458,
11.332865832173));
#20636=CARTESIAN_POINT('Ctrl Pts',(-9.03195918428352,-0.906002682172395,
11.3453467654212));
#20637=CARTESIAN_POINT('Ctrl Pts',(-8.76814132834391,-1.01583545019906,
11.3578276986694));
#20638=CARTESIAN_POINT('Ctrl Pts',(-8.50243547044515,-1.0164720823066,11.3703086319176));
#20639=CARTESIAN_POINT('Ctrl Pts',(-8.23672961254639,-1.01710871441414,
11.3827895651658));
#20640=CARTESIAN_POINT('Ctrl Pts',(-7.97238846933342,-0.908541417082803,
11.395270498414));
#20641=CARTESIAN_POINT('Ctrl Pts',(-7.78383148002345,-0.721334926798635,
11.4077514316622));
#20642=CARTESIAN_POINT('Ctrl Pts',(-7.59527449071347,-0.534128436514468,
11.4202323649104));
#20643=CARTESIAN_POINT('Ctrl Pts',(-7.48480993131704,-0.27057449675579,
11.4327132981586));
#20644=CARTESIAN_POINT('Ctrl Pts',(-7.48353667075686,-0.00487092690829271,
11.4451942314068));
#20645=CARTESIAN_POINT('Ctrl Pts',(-7.48226341019667,0.260832642939205,
11.457675164655));
#20646=CARTESIAN_POINT('Ctrl Pts',(-7.5901970354675,0.525433154240419,11.4701560979031));
#20647=CARTESIAN_POINT('Ctrl Pts',(-7.77695120652518,0.714438148393269,
11.4826370311513));
#20648=CARTESIAN_POINT('Ctrl Pts',(-7.96370537758285,0.903443142546119,
11.4951179643995));
#20649=CARTESIAN_POINT('Ctrl Pts',(-8.2269938881483,1.0145388591566,11.5075988976477));
#20650=CARTESIAN_POINT('Ctrl Pts',(-8.49269364459162,1.01644874085989,11.5200798308959));
#20651=CARTESIAN_POINT('Ctrl Pts',(-8.75839340103493,1.01835862256317,11.5325607641441));
#20652=CARTESIAN_POINT('Ctrl Pts',(-9.02325176140393,0.911059288978959,
11.5450416973923));
#20653=CARTESIAN_POINT('Ctrl Pts',(-9.21270367535846,0.72475850926743,11.5575226306405));
#20654=CARTESIAN_POINT('Ctrl Pts',(-9.40215558931299,0.538457729555902,
11.5700035638887));
#20655=CARTESIAN_POINT('Ctrl Pts',(-9.51388182535845,0.275436159672211,
11.5824844971369));
#20656=CARTESIAN_POINT('Ctrl Pts',(-9.51642831724057,0.00974174196409921,
11.5949654303851));
#20657=CARTESIAN_POINT('Ctrl Pts',(-9.51645943884197,0.00649459406658459,
11.5951179643995));
#20658=CARTESIAN_POINT('Ctrl Pts',(-9.516475,0.00324729703375226,11.595270498414));
#20659=CARTESIAN_POINT('Ctrl Pts',(-9.516475,4.63357137348595E-13,11.5954230324285));
#20660=CARTESIAN_POINT('Ctrl Pts',(-9.516475,4.68384518537177E-13,11.3545769675715));
#20661=CARTESIAN_POINT('Ctrl Pts',(-9.51647500000012,-0.26570662058351,
11.3670579008197));
#20662=CARTESIAN_POINT('Ctrl Pts',(-9.40727465387219,-0.529786878176741,
11.3795388340679));
#20663=CARTESIAN_POINT('Ctrl Pts',(-9.21961691907786,-0.717894780174561,
11.3920197673161));
#20664=CARTESIAN_POINT('Ctrl Pts',(-9.03195918428354,-0.906002682172381,
11.4045007005643));
#20665=CARTESIAN_POINT('Ctrl Pts',(-8.76814132834394,-1.01583545019905,
11.4169816338125));
#20666=CARTESIAN_POINT('Ctrl Pts',(-8.50243547044518,-1.0164720823066,11.4294625670606));
#20667=CARTESIAN_POINT('Ctrl Pts',(-8.23672961254641,-1.01710871441415,
11.4419435003088));
#20668=CARTESIAN_POINT('Ctrl Pts',(-7.97238846933345,-0.908541417082817,
11.454424433557));
#20669=CARTESIAN_POINT('Ctrl Pts',(-7.78383148002347,-0.721334926798654,
11.4669053668052));
#20670=CARTESIAN_POINT('Ctrl Pts',(-7.59527449071349,-0.534128436514492,
11.4793863000534));
#20671=CARTESIAN_POINT('Ctrl Pts',(-7.48480993131705,-0.270574496755817,
11.4918672333016));
#20672=CARTESIAN_POINT('Ctrl Pts',(-7.48353667075686,-0.00487092690831965,
11.5043481665498));
#20673=CARTESIAN_POINT('Ctrl Pts',(-7.48226341019666,0.260832642939178,
11.516829099798));
#20674=CARTESIAN_POINT('Ctrl Pts',(-7.59019703546749,0.525433154240395,
11.5293100330462));
#20675=CARTESIAN_POINT('Ctrl Pts',(-7.77695120652516,0.71443814839325,11.5417909662944));
#20676=CARTESIAN_POINT('Ctrl Pts',(-7.96370537758283,0.903443142546105,
11.5542718995426));
#20677=CARTESIAN_POINT('Ctrl Pts',(-8.22699388814827,1.01453885915659,11.5667528327907));
#20678=CARTESIAN_POINT('Ctrl Pts',(-8.49269364459159,1.01644874085988,11.5792337660389));
#20679=CARTESIAN_POINT('Ctrl Pts',(-8.7583934010349,1.01835862256318,11.5917146992871));
#20680=CARTESIAN_POINT('Ctrl Pts',(-9.0232517614039,0.911059288978973,11.6041956325353));
#20681=CARTESIAN_POINT('Ctrl Pts',(-9.21270367535844,0.724758509267449,
11.6166765657835));
#20682=CARTESIAN_POINT('Ctrl Pts',(-9.40215558931297,0.538457729555925,
11.6291574990317));
#20683=CARTESIAN_POINT('Ctrl Pts',(-9.51388182535844,0.275436159672238,
11.6416384322799));
#20684=CARTESIAN_POINT('Ctrl Pts',(-9.51642831724057,0.00974174196412615,
11.6541193655281));
#20685=CARTESIAN_POINT('Ctrl Pts',(-9.51645943884197,0.0064945940666019,
11.6542718995426));
#20686=CARTESIAN_POINT('Ctrl Pts',(-9.516475,0.00324729703376001,11.654424433557));
#20687=CARTESIAN_POINT('Ctrl Pts',(-9.516475,4.61410993834892E-13,11.6545769675715));
#20688=CARTESIAN_POINT('Origin',(-8.5,0.,1.24542303242842));
#20689=CARTESIAN_POINT('',(-9.516475,4.19524224387624E-13,10.9954230324285));
#20690=CARTESIAN_POINT('',(-9.516475,4.17578129052922E-13,11.0545769675715));
#20691=CARTESIAN_POINT('',(-9.516475,1.78524650477582E-12,1.24542303242842));
#20692=CARTESIAN_POINT('Ctrl Pts',(-9.51619870214038,-0.000607203370645813,
10.9954230324285));
#20693=CARTESIAN_POINT('Ctrl Pts',(-9.51677980361449,-0.106684728097461,
11.0003988638818));
#20694=CARTESIAN_POINT('Ctrl Pts',(-9.45103666736097,-0.551056728109718,
11.0212820364867));
#20695=CARTESIAN_POINT('Ctrl Pts',(-8.80852576484242,-1.162383479345,11.0580725502433));
#20696=CARTESIAN_POINT('Ctrl Pts',(-7.68802200901459,-0.88700948808109,
11.1057945736981));
#20697=CARTESIAN_POINT('Ctrl Pts',(-7.31554839363375,0.202723257387539,
11.153516597153));
#20698=CARTESIAN_POINT('Ctrl Pts',(-8.02922823218693,1.10655683650717,11.2012386206079));
#20699=CARTESIAN_POINT('Ctrl Pts',(-9.16742973518675,0.994609589396969,
11.2485407656997));
#20700=CARTESIAN_POINT('Ctrl Pts',(-9.51644808261045,0.328213381768027,
11.2799355696399));
#20701=CARTESIAN_POINT('Ctrl Pts',(-9.51769479449051,-0.000263157468651742,
11.2954230324285));
#20702=CARTESIAN_POINT('Ctrl Pts',(-9.516475,5.04248000332732E-13,11.0545769675715));
#20703=CARTESIAN_POINT('Ctrl Pts',(-9.51647500000013,-0.265706620583474,
11.0670579008197));
#20704=CARTESIAN_POINT('Ctrl Pts',(-9.40727465387221,-0.529786878176709,
11.0795388340679));
#20705=CARTESIAN_POINT('Ctrl Pts',(-9.21961691907789,-0.717894780174535,
11.0920197673161));
#20706=CARTESIAN_POINT('Ctrl Pts',(-9.03195918428357,-0.906002682172362,
11.1045007005643));
#20707=CARTESIAN_POINT('Ctrl Pts',(-8.76814132834398,-1.01583545019904,
11.1169816338125));
#20708=CARTESIAN_POINT('Ctrl Pts',(-8.50243547044521,-1.0164720823066,11.1294625670606));
#20709=CARTESIAN_POINT('Ctrl Pts',(-8.23672961254645,-1.01710871441416,
11.1419435003088));
#20710=CARTESIAN_POINT('Ctrl Pts',(-7.97238846933348,-0.908541417082836,
11.154424433557));
#20711=CARTESIAN_POINT('Ctrl Pts',(-7.78383148002349,-0.72133492679868,
11.1669053668052));
#20712=CARTESIAN_POINT('Ctrl Pts',(-7.5952744907135,-0.534128436514524,
11.1793863000534));
#20713=CARTESIAN_POINT('Ctrl Pts',(-7.48480993131706,-0.270574496755853,
11.1918672333016));
#20714=CARTESIAN_POINT('Ctrl Pts',(-7.48353667075686,-0.00487092690835552,
11.2043481665498));
#20715=CARTESIAN_POINT('Ctrl Pts',(-7.48226341019666,0.260832642939142,
11.216829099798));
#20716=CARTESIAN_POINT('Ctrl Pts',(-7.59019703546747,0.525433154240363,
11.2293100330462));
#20717=CARTESIAN_POINT('Ctrl Pts',(-7.77695120652513,0.714438148393224,
11.2417909662944));
#20718=CARTESIAN_POINT('Ctrl Pts',(-7.9637053775828,0.903443142546086,11.2542718995426));
#20719=CARTESIAN_POINT('Ctrl Pts',(-8.22699388814824,1.01453885915658,11.2667528327907));
#20720=CARTESIAN_POINT('Ctrl Pts',(-8.49269364459155,1.01644874085988,11.2792337660389));
#20721=CARTESIAN_POINT('Ctrl Pts',(-8.75839340103487,1.01835862256319,11.2917146992871));
#20722=CARTESIAN_POINT('Ctrl Pts',(-9.02325176140387,0.911059288978991,
11.3041956325353));
#20723=CARTESIAN_POINT('Ctrl Pts',(-9.21270367535841,0.724758509267474,
11.3166765657835));
#20724=CARTESIAN_POINT('Ctrl Pts',(-9.40215558931295,0.538457729555957,
11.3291574990317));
#20725=CARTESIAN_POINT('Ctrl Pts',(-9.51388182535843,0.275436159672273,
11.3416384322799));
#20726=CARTESIAN_POINT('Ctrl Pts',(-9.51642831724057,0.00974174196416202,
11.3541193655281));
#20727=CARTESIAN_POINT('Ctrl Pts',(-9.51645943884197,0.00649459406662814,
11.3542718995426));
#20728=CARTESIAN_POINT('Ctrl Pts',(-9.516475,0.00324729703377659,11.354424433557));
#20729=CARTESIAN_POINT('Ctrl Pts',(-9.516475,4.68384518537177E-13,11.3545769675715));
#20730=CARTESIAN_POINT('Origin',(-8.5,0.,1.24542303242842));
#20731=CARTESIAN_POINT('',(-9.51589299709112,9.73851207509147E-5,10.6954230324285));
#20732=CARTESIAN_POINT('',(-9.516475,3.95661696661937E-13,10.7545769675715));
#20733=CARTESIAN_POINT('',(-9.516475,1.78524650477582E-12,1.24542303242842));
#20734=CARTESIAN_POINT('Ctrl Pts',(-9.516475,3.9760784017564E-13,10.6954230324285));
#20735=CARTESIAN_POINT('Ctrl Pts',(-9.5164750000001,-0.265706620583571,
10.7079039656767));
#20736=CARTESIAN_POINT('Ctrl Pts',(-9.40727465387216,-0.529786878176785,
10.7203848989249));
#20737=CARTESIAN_POINT('Ctrl Pts',(-9.21961691907784,-0.717894780174591,
10.732865832173));
#20738=CARTESIAN_POINT('Ctrl Pts',(-9.03195918428351,-0.906002682172396,
10.7453467654212));
#20739=CARTESIAN_POINT('Ctrl Pts',(-8.76814132834392,-1.01583545019905,
10.7578276986694));
#20740=CARTESIAN_POINT('Ctrl Pts',(-8.50243547044516,-1.0164720823066,10.7703086319176));
#20741=CARTESIAN_POINT('Ctrl Pts',(-8.23672961254641,-1.01710871441414,
10.7827895651658));
#20742=CARTESIAN_POINT('Ctrl Pts',(-7.97238846933345,-0.908541417082819,
10.795270498414));
#20743=CARTESIAN_POINT('Ctrl Pts',(-7.78383148002348,-0.721334926798666,
10.8077514316622));
#20744=CARTESIAN_POINT('Ctrl Pts',(-7.5952744907135,-0.534128436514513,
10.8202323649104));
#20745=CARTESIAN_POINT('Ctrl Pts',(-7.48480993131706,-0.270574496755852,
10.8327132981586));
#20746=CARTESIAN_POINT('Ctrl Pts',(-7.48353667075686,-0.00487092690836444,
10.8451942314068));
#20747=CARTESIAN_POINT('Ctrl Pts',(-7.48226341019665,0.260832642939124,
10.857675164655));
#20748=CARTESIAN_POINT('Ctrl Pts',(-7.59019703546746,0.525433154240336,
10.8701560979031));
#20749=CARTESIAN_POINT('Ctrl Pts',(-7.77695120652511,0.714438148393197,
10.8826370311513));
#20750=CARTESIAN_POINT('Ctrl Pts',(-7.96370537758276,0.903443142546059,
10.8951179643995));
#20751=CARTESIAN_POINT('Ctrl Pts',(-8.22699388814818,1.01453885915656,10.9075988976477));
#20752=CARTESIAN_POINT('Ctrl Pts',(-8.49269364459149,1.01644874085988,10.9200798308959));
#20753=CARTESIAN_POINT('Ctrl Pts',(-8.75839340103479,1.0183586225632,10.9325607641441));
#20754=CARTESIAN_POINT('Ctrl Pts',(-9.02325176140379,0.911059288979034,
10.9450416973923));
#20755=CARTESIAN_POINT('Ctrl Pts',(-9.21270367535834,0.724758509267541,
10.9575226306405));
#20756=CARTESIAN_POINT('Ctrl Pts',(-9.4021555893129,0.538457729556049,10.9700035638887));
#20757=CARTESIAN_POINT('Ctrl Pts',(-9.5138818253584,0.275436159672388,10.9824844971369));
#20758=CARTESIAN_POINT('Ctrl Pts',(-9.51642831724057,0.00974174196428649,
10.994965430385));
#20759=CARTESIAN_POINT('Ctrl Pts',(-9.51645943884197,0.00649459406669484,
10.9951179643995));
#20760=CARTESIAN_POINT('Ctrl Pts',(-9.516475,0.00324729703378546,10.995270498414));
#20761=CARTESIAN_POINT('Ctrl Pts',(-9.516475,4.19524272566625E-13,10.9954230324285));
#20762=CARTESIAN_POINT('Ctrl Pts',(-9.516475,4.24551653755207E-13,10.7545769675715));
#20763=CARTESIAN_POINT('Ctrl Pts',(-9.51647500000011,-0.265706620583535,
10.7670579008197));
#20764=CARTESIAN_POINT('Ctrl Pts',(-9.40727465387218,-0.529786878176742,
10.7795388340679));
#20765=CARTESIAN_POINT('Ctrl Pts',(-9.21961691907788,-0.717894780174551,
10.7920197673161));
#20766=CARTESIAN_POINT('Ctrl Pts',(-9.03195918428357,-0.90600268217236,
10.8045007005643));
#20767=CARTESIAN_POINT('Ctrl Pts',(-8.76814132834399,-1.01583545019903,
10.8169816338125));
#20768=CARTESIAN_POINT('Ctrl Pts',(-8.50243547044525,-1.0164720823066,10.8294625670606));
#20769=CARTESIAN_POINT('Ctrl Pts',(-8.2367296125465,-1.01710871441416,10.8419435003088));
#20770=CARTESIAN_POINT('Ctrl Pts',(-7.97238846933355,-0.908541417082871,
10.854424433557));
#20771=CARTESIAN_POINT('Ctrl Pts',(-7.78383148002356,-0.721334926798746,
10.8669053668052));
#20772=CARTESIAN_POINT('Ctrl Pts',(-7.59527449071357,-0.534128436514621,
10.8793863000534));
#20773=CARTESIAN_POINT('Ctrl Pts',(-7.4848099313171,-0.270574496755985,
10.8918672333016));
#20774=CARTESIAN_POINT('Ctrl Pts',(-7.48353667075686,-0.00487092690850694,
10.9043481665498));
#20775=CARTESIAN_POINT('Ctrl Pts',(-7.48226341019662,0.260832642938971,
10.916829099798));
#20776=CARTESIAN_POINT('Ctrl Pts',(-7.59019703546737,0.525433154240189,
10.9293100330462));
#20777=CARTESIAN_POINT('Ctrl Pts',(-7.77695120652499,0.714438148393076,
10.9417909662944));
#20778=CARTESIAN_POINT('Ctrl Pts',(-7.9637053775826,0.903443142545962,10.9542718995425));
#20779=CARTESIAN_POINT('Ctrl Pts',(-8.22699388814799,1.01453885915651,10.9667528327907));
#20780=CARTESIAN_POINT('Ctrl Pts',(-8.49269364459129,1.01644874085988,10.9792337660389));
#20781=CARTESIAN_POINT('Ctrl Pts',(-8.75839340103458,1.01835862256325,10.9917146992871));
#20782=CARTESIAN_POINT('Ctrl Pts',(-9.02325176140359,0.911059288979145,
11.0041956325353));
#20783=CARTESIAN_POINT('Ctrl Pts',(-9.21270367535818,0.724758509267702,
11.0166765657835));
#20784=CARTESIAN_POINT('Ctrl Pts',(-9.40215558931277,0.538457729556259,
11.0291574990317));
#20785=CARTESIAN_POINT('Ctrl Pts',(-9.51388182535833,0.275436159672636,
11.0416384322799));
#20786=CARTESIAN_POINT('Ctrl Pts',(-9.51642831724057,0.00974174196454454,
11.0541193655281));
#20787=CARTESIAN_POINT('Ctrl Pts',(-9.51645943884197,0.00649459406689512,
11.0542718995425));
#20788=CARTESIAN_POINT('Ctrl Pts',(-9.516475,0.00324729703392801,11.054424433557));
#20789=CARTESIAN_POINT('Ctrl Pts',(-9.516475,5.04248000332732E-13,11.0545769675715));
#20790=CARTESIAN_POINT('Origin',(-8.5,0.,1.24542303242842));
#20791=CARTESIAN_POINT('',(-9.51672077363507,0.000183314671464046,10.3954230324285));
#20792=CARTESIAN_POINT('',(-9.516475,3.73745264270951E-13,10.4545769675715));
#20793=CARTESIAN_POINT('',(-9.516475,1.78524650477582E-12,1.24542303242842));
#20794=CARTESIAN_POINT('Ctrl Pts',(-9.51772011037067,0.000928687888346325,
10.3954230324285));
#20795=CARTESIAN_POINT('Ctrl Pts',(-9.51551864793062,-0.297960855620615,
10.4095107700623));
#20796=CARTESIAN_POINT('Ctrl Pts',(-9.21783085496887,-0.93919810709799,
10.4395058488478));
#20797=CARTESIAN_POINT('Ctrl Pts',(-8.12901546541348,-1.14297541618665,
10.4854082687849));
#20798=CARTESIAN_POINT('Ctrl Pts',(-7.33723505164926,-0.306711207290376,
10.5331302922398));
#20799=CARTESIAN_POINT('Ctrl Pts',(-7.61417160911282,0.813407377962594,
10.5808523156946));
#20800=CARTESIAN_POINT('Ctrl Pts',(-8.52205763101126,1.12124235117773,10.6206206685737));
#20801=CARTESIAN_POINT('Ctrl Pts',(-9.1565775804327,0.82795583618433,10.6524353508769));
#20802=CARTESIAN_POINT('Ctrl Pts',(-9.45785075121687,0.442033743097962,
10.6747182486366));
#20803=CARTESIAN_POINT('Ctrl Pts',(-9.51514599649507,0.136437782201491,
10.6890474758204));
#20804=CARTESIAN_POINT('Ctrl Pts',(-9.51462354101672,0.000309800094462256,
10.6954230324285));
#20805=CARTESIAN_POINT('Ctrl Pts',(-9.516475,4.31525178457491E-13,10.4545769675715));
#20806=CARTESIAN_POINT('Ctrl Pts',(-9.51647500000011,-0.265706620583547,
10.4670579008197));
#20807=CARTESIAN_POINT('Ctrl Pts',(-9.40727465387217,-0.529786878176774,
10.4795388340679));
#20808=CARTESIAN_POINT('Ctrl Pts',(-9.21961691907784,-0.717894780174587,
10.4920197673161));
#20809=CARTESIAN_POINT('Ctrl Pts',(-9.03195918428351,-0.9060026821724,10.5045007005643));
#20810=CARTESIAN_POINT('Ctrl Pts',(-8.7681413283439,-1.01583545019906,10.5169816338125));
#20811=CARTESIAN_POINT('Ctrl Pts',(-8.50243547044514,-1.0164720823066,10.5294625670606));
#20812=CARTESIAN_POINT('Ctrl Pts',(-8.23672961254638,-1.01710871441414,
10.5419435003088));
#20813=CARTESIAN_POINT('Ctrl Pts',(-7.97238846933341,-0.908541417082798,
10.554424433557));
#20814=CARTESIAN_POINT('Ctrl Pts',(-7.78383148002344,-0.721334926798628,
10.5669053668052));
#20815=CARTESIAN_POINT('Ctrl Pts',(-7.59527449071347,-0.534128436514459,
10.5793863000534));
#20816=CARTESIAN_POINT('Ctrl Pts',(-7.48480993131704,-0.27057449675578,
10.5918672333016));
#20817=CARTESIAN_POINT('Ctrl Pts',(-7.48353667075686,-0.0048709269082828,
10.6043481665498));
#20818=CARTESIAN_POINT('Ctrl Pts',(-7.48226341019667,0.260832642939215,
10.616829099798));
#20819=CARTESIAN_POINT('Ctrl Pts',(-7.59019703546751,0.525433154240428,
10.6293100330462));
#20820=CARTESIAN_POINT('Ctrl Pts',(-7.77695120652518,0.714438148393276,
10.6417909662944));
#20821=CARTESIAN_POINT('Ctrl Pts',(-7.96370537758286,0.903443142546124,
10.6542718995426));
#20822=CARTESIAN_POINT('Ctrl Pts',(-8.22699388814831,1.0145388591566,10.6667528327907));
#20823=CARTESIAN_POINT('Ctrl Pts',(-8.49269364459163,1.01644874085989,10.6792337660389));
#20824=CARTESIAN_POINT('Ctrl Pts',(-8.75839340103494,1.01835862256317,10.6917146992871));
#20825=CARTESIAN_POINT('Ctrl Pts',(-9.02325176140394,0.911059288978954,
10.7041956325353));
#20826=CARTESIAN_POINT('Ctrl Pts',(-9.21270367535846,0.724758509267423,
10.7166765657835));
#20827=CARTESIAN_POINT('Ctrl Pts',(-9.40215558931299,0.538457729555893,
10.7291574990317));
#20828=CARTESIAN_POINT('Ctrl Pts',(-9.51388182535845,0.275436159672201,
10.7416384322799));
#20829=CARTESIAN_POINT('Ctrl Pts',(-9.51642831724057,0.0097417419640893,
10.7541193655281));
#20830=CARTESIAN_POINT('Ctrl Pts',(-9.51645943884197,0.00649459406656504,
10.7542718995426));
#20831=CARTESIAN_POINT('Ctrl Pts',(-9.516475,0.00324729703372315,10.754424433557));
#20832=CARTESIAN_POINT('Ctrl Pts',(-9.516475,4.24551653755207E-13,10.7545769675715));
#20833=CARTESIAN_POINT('Origin',(-8.5,0.,1.24542303242842));
#20834=CARTESIAN_POINT('',(-9.516475,3.248850183004E-13,10.0954230324285));
#20835=CARTESIAN_POINT('',(-9.516475,3.51828831879967E-13,10.1545769675715));
#20836=CARTESIAN_POINT('',(-9.516475,1.78524650477582E-12,1.24542303242842));
#20837=CARTESIAN_POINT('Ctrl Pts',(-9.516475,3.5377497539367E-13,10.0954230324285));
#20838=CARTESIAN_POINT('Ctrl Pts',(-9.51647500000009,-0.265706620583625,
10.1079039656767));
#20839=CARTESIAN_POINT('Ctrl Pts',(-9.40727465387213,-0.529786878176844,
10.1203848989249));
#20840=CARTESIAN_POINT('Ctrl Pts',(-9.21961691907778,-0.717894780174642,
10.1328658321731));
#20841=CARTESIAN_POINT('Ctrl Pts',(-9.03195918428344,-0.906002682172441,
10.1453467654212));
#20842=CARTESIAN_POINT('Ctrl Pts',(-8.76814132834383,-1.01583545019908,
10.1578276986694));
#20843=CARTESIAN_POINT('Ctrl Pts',(-8.50243547044506,-1.0164720823066,10.1703086319176));
#20844=CARTESIAN_POINT('Ctrl Pts',(-8.2367296125463,-1.01710871441412,10.1827895651658));
#20845=CARTESIAN_POINT('Ctrl Pts',(-7.97238846933334,-0.908541417082758,
10.195270498414));
#20846=CARTESIAN_POINT('Ctrl Pts',(-7.78383148002338,-0.721334926798574,
10.2077514316622));
#20847=CARTESIAN_POINT('Ctrl Pts',(-7.59527449071343,-0.53412843651439,
10.2202323649104));
#20848=CARTESIAN_POINT('Ctrl Pts',(-7.48480993131702,-0.270574496755703,
10.2327132981586));
#20849=CARTESIAN_POINT('Ctrl Pts',(-7.48353667075686,-0.00487092690820505,
10.2451942314068));
#20850=CARTESIAN_POINT('Ctrl Pts',(-7.48226341019669,0.260832642939293,
10.257675164655));
#20851=CARTESIAN_POINT('Ctrl Pts',(-7.59019703546755,0.525433154240497,
10.2701560979032));
#20852=CARTESIAN_POINT('Ctrl Pts',(-7.77695120652524,0.714438148393331,
10.2826370311513));
#20853=CARTESIAN_POINT('Ctrl Pts',(-7.96370537758293,0.903443142546165,
10.2951179643995));
#20854=CARTESIAN_POINT('Ctrl Pts',(-8.22699388814839,1.01453885915662,10.3075988976477));
#20855=CARTESIAN_POINT('Ctrl Pts',(-8.4926936445917,1.01644874085989,10.3200798308959));
#20856=CARTESIAN_POINT('Ctrl Pts',(-8.75839340103502,1.01835862256315,10.3325607641441));
#20857=CARTESIAN_POINT('Ctrl Pts',(-9.023251761404,0.911059288978914,10.3450416973923));
#20858=CARTESIAN_POINT('Ctrl Pts',(-9.21270367535852,0.724758509267369,
10.3575226306405));
#20859=CARTESIAN_POINT('Ctrl Pts',(-9.40215558931303,0.538457729555824,
10.3700035638887));
#20860=CARTESIAN_POINT('Ctrl Pts',(-9.51388182535847,0.275436159672123,
10.3824844971369));
#20861=CARTESIAN_POINT('Ctrl Pts',(-9.51642831724057,0.00974174196401155,
10.3949654303851));
#20862=CARTESIAN_POINT('Ctrl Pts',(-9.51645943884197,0.00649459406649692,
10.3951179643995));
#20863=CARTESIAN_POINT('Ctrl Pts',(-9.516475,0.00324729703366459,10.395270498414));
#20864=CARTESIAN_POINT('Ctrl Pts',(-9.516475,3.75691407784655E-13,10.3954230324285));
#20865=CARTESIAN_POINT('Ctrl Pts',(-9.516475,3.80718788973236E-13,10.1545769675715));
#20866=CARTESIAN_POINT('Ctrl Pts',(-9.5164750000001,-0.265706620583598,
10.1670579008197));
#20867=CARTESIAN_POINT('Ctrl Pts',(-9.40727465387214,-0.529786878176819,
10.1795388340679));
#20868=CARTESIAN_POINT('Ctrl Pts',(-9.2196169190778,-0.717894780174623,
10.1920197673161));
#20869=CARTESIAN_POINT('Ctrl Pts',(-9.03195918428346,-0.906002682172426,
10.2045007005643));
#20870=CARTESIAN_POINT('Ctrl Pts',(-8.76814132834385,-1.01583545019907,
10.2169816338125));
#20871=CARTESIAN_POINT('Ctrl Pts',(-8.50243547044509,-1.0164720823066,10.2294625670606));
#20872=CARTESIAN_POINT('Ctrl Pts',(-8.23672961254633,-1.01710871441412,
10.2419435003088));
#20873=CARTESIAN_POINT('Ctrl Pts',(-7.97238846933337,-0.908541417082772,
10.254424433557));
#20874=CARTESIAN_POINT('Ctrl Pts',(-7.7838314800234,-0.721334926798593,
10.2669053668052));
#20875=CARTESIAN_POINT('Ctrl Pts',(-7.59527449071344,-0.534128436514414,
10.2793863000534));
#20876=CARTESIAN_POINT('Ctrl Pts',(-7.48480993131703,-0.27057449675573,
10.2918672333016));
#20877=CARTESIAN_POINT('Ctrl Pts',(-7.48353667075686,-0.00487092690823199,
10.3043481665498));
#20878=CARTESIAN_POINT('Ctrl Pts',(-7.48226341019669,0.260832642939266,
10.316829099798));
#20879=CARTESIAN_POINT('Ctrl Pts',(-7.59019703546753,0.525433154240473,
10.3293100330462));
#20880=CARTESIAN_POINT('Ctrl Pts',(-7.77695120652522,0.714438148393312,
10.3417909662944));
#20881=CARTESIAN_POINT('Ctrl Pts',(-7.96370537758291,0.903443142546151,
10.3542718995426));
#20882=CARTESIAN_POINT('Ctrl Pts',(-8.22699388814836,1.01453885915662,10.3667528327907));
#20883=CARTESIAN_POINT('Ctrl Pts',(-8.49269364459168,1.01644874085989,10.3792337660389));
#20884=CARTESIAN_POINT('Ctrl Pts',(-8.75839340103499,1.01835862256316,10.3917146992871));
#20885=CARTESIAN_POINT('Ctrl Pts',(-9.02325176140398,0.911059288978928,
10.4041956325353));
#20886=CARTESIAN_POINT('Ctrl Pts',(-9.2127036753585,0.724758509267388,10.4166765657835));
#20887=CARTESIAN_POINT('Ctrl Pts',(-9.40215558931302,0.538457729555847,
10.4291574990317));
#20888=CARTESIAN_POINT('Ctrl Pts',(-9.51388182535847,0.27543615967215,10.4416384322799));
#20889=CARTESIAN_POINT('Ctrl Pts',(-9.51642831724057,0.00974174196403849,
10.4541193655281));
#20890=CARTESIAN_POINT('Ctrl Pts',(-9.51645943884197,0.0064945940665335,
10.4542718995426));
#20891=CARTESIAN_POINT('Ctrl Pts',(-9.516475,0.00324729703371082,10.454424433557));
#20892=CARTESIAN_POINT('Ctrl Pts',(-9.516475,4.31525178457491E-13,10.4545769675715));
#20893=CARTESIAN_POINT('Origin',(-8.5,0.,1.24542303242842));
#20894=CARTESIAN_POINT('',(-9.51618379816054,-4.38257510333499E-5,9.79542303242848));
#20895=CARTESIAN_POINT('',(-9.516475,3.29912399488981E-13,9.8545769675715));
#20896=CARTESIAN_POINT('',(-9.516475,1.78524650477582E-12,1.24542303242842));
#20897=CARTESIAN_POINT('Ctrl Pts',(-9.516475,3.31858543002685E-13,9.79542303242848));
#20898=CARTESIAN_POINT('Ctrl Pts',(-9.51647500000009,-0.265706620583637,
9.80790396567667));
#20899=CARTESIAN_POINT('Ctrl Pts',(-9.40727465387213,-0.529786878176844,
9.82038489892486));
#20900=CARTESIAN_POINT('Ctrl Pts',(-9.21961691907779,-0.717894780174637,
9.83286583217305));
#20901=CARTESIAN_POINT('Ctrl Pts',(-9.03195918428345,-0.90600268217243,
9.84534676542124));
#20902=CARTESIAN_POINT('Ctrl Pts',(-8.76814132834385,-1.01583545019907,
9.85782769866943));
#20903=CARTESIAN_POINT('Ctrl Pts',(-8.5024354704451,-1.0164720823066,9.87030863191762));
#20904=CARTESIAN_POINT('Ctrl Pts',(-8.23672961254634,-1.01710871441413,
9.88278956516581));
#20905=CARTESIAN_POINT('Ctrl Pts',(-7.97238846933339,-0.908541417082785,
9.895270498414));
#20906=CARTESIAN_POINT('Ctrl Pts',(-7.78383148002343,-0.721334926798619,
9.90775143166219));
#20907=CARTESIAN_POINT('Ctrl Pts',(-7.59527449071347,-0.534128436514454,
9.92023236491038));
#20908=CARTESIAN_POINT('Ctrl Pts',(-7.48480993131704,-0.270574496755787,
9.93271329815857));
#20909=CARTESIAN_POINT('Ctrl Pts',(-7.48353667075686,-0.00487092690829869,
9.94519423140676));
#20910=CARTESIAN_POINT('Ctrl Pts',(-7.48226341019667,0.260832642939189,
9.95767516465495));
#20911=CARTESIAN_POINT('Ctrl Pts',(-7.59019703546749,0.525433154240395,
9.97015609790315));
#20912=CARTESIAN_POINT('Ctrl Pts',(-7.77695120652515,0.714438148393244,
9.98263703115134));
#20913=CARTESIAN_POINT('Ctrl Pts',(-7.96370537758281,0.903443142546094,
9.99511796439953));
#20914=CARTESIAN_POINT('Ctrl Pts',(-8.22699388814825,1.01453885915658,10.0075988976477));
#20915=CARTESIAN_POINT('Ctrl Pts',(-8.49269364459155,1.01644874085988,10.0200798308959));
#20916=CARTESIAN_POINT('Ctrl Pts',(-8.75839340103486,1.01835862256319,10.0325607641441));
#20917=CARTESIAN_POINT('Ctrl Pts',(-9.02325176140385,0.911059288979,10.0450416973923));
#20918=CARTESIAN_POINT('Ctrl Pts',(-9.21270367535839,0.724758509267495,
10.0575226306405));
#20919=CARTESIAN_POINT('Ctrl Pts',(-9.40215558931293,0.53845772955599,10.0700035638887));
#20920=CARTESIAN_POINT('Ctrl Pts',(-9.51388182535842,0.275436159672322,
10.0824844971369));
#20921=CARTESIAN_POINT('Ctrl Pts',(-9.51642831724057,0.00974174196422074,
10.0949654303851));
#20922=CARTESIAN_POINT('Ctrl Pts',(-9.51645943884197,0.00649459406662909,
10.0951179643995));
#20923=CARTESIAN_POINT('Ctrl Pts',(-9.516475,0.00324729703371972,10.095270498414));
#20924=CARTESIAN_POINT('Ctrl Pts',(-9.516475,3.5377497539367E-13,10.0954230324285));
#20925=CARTESIAN_POINT('Ctrl Pts',(-9.516475,3.87692313675521E-13,9.8545769675715));
#20926=CARTESIAN_POINT('Ctrl Pts',(-9.5164750000001,-0.265706620583571,
9.86705790081969));
#20927=CARTESIAN_POINT('Ctrl Pts',(-9.40727465387216,-0.529786878176775,
9.87953883406788));
#20928=CARTESIAN_POINT('Ctrl Pts',(-9.21961691907785,-0.717894780174577,
9.89201976731607));
#20929=CARTESIAN_POINT('Ctrl Pts',(-9.03195918428353,-0.906002682172379,
9.90450070056426));
#20930=CARTESIAN_POINT('Ctrl Pts',(-8.76814132834396,-1.01583545019904,
9.91698163381245));
#20931=CARTESIAN_POINT('Ctrl Pts',(-8.50243547044521,-1.0164720823066,9.92946256706064));
#20932=CARTESIAN_POINT('Ctrl Pts',(-8.23672961254647,-1.01710871441415,
9.94194350030883));
#20933=CARTESIAN_POINT('Ctrl Pts',(-7.97238846933351,-0.908541417082852,
9.95442443355702));
#20934=CARTESIAN_POINT('Ctrl Pts',(-7.78383148002353,-0.72133492679872,
9.96690536680521));
#20935=CARTESIAN_POINT('Ctrl Pts',(-7.59527449071355,-0.534128436514588,
9.9793863000534));
#20936=CARTESIAN_POINT('Ctrl Pts',(-7.48480993131709,-0.270574496755948,
9.99186723330159));
#20937=CARTESIAN_POINT('Ctrl Pts',(-7.48353667075686,-0.00487092690847008,
10.0043481665498));
#20938=CARTESIAN_POINT('Ctrl Pts',(-7.48226341019663,0.260832642939008,
10.016829099798));
#20939=CARTESIAN_POINT('Ctrl Pts',(-7.59019703546739,0.525433154240222,
10.0293100330462));
#20940=CARTESIAN_POINT('Ctrl Pts',(-7.77695120652501,0.714438148393102,
10.0417909662944));
#20941=CARTESIAN_POINT('Ctrl Pts',(-7.96370537758263,0.903443142545981,
10.0542718995425));
#20942=CARTESIAN_POINT('Ctrl Pts',(-8.22699388814803,1.01453885915652,10.0667528327907));
#20943=CARTESIAN_POINT('Ctrl Pts',(-8.49269364459132,1.01644874085988,10.0792337660389));
#20944=CARTESIAN_POINT('Ctrl Pts',(-8.75839340103462,1.01835862256325,10.0917146992871));
#20945=CARTESIAN_POINT('Ctrl Pts',(-9.02325176140362,0.911059288979126,
10.1041956325353));
#20946=CARTESIAN_POINT('Ctrl Pts',(-9.21270367535821,0.724758509267676,
10.1166765657835));
#20947=CARTESIAN_POINT('Ctrl Pts',(-9.40215558931279,0.538457729556226,
10.1291574990317));
#20948=CARTESIAN_POINT('Ctrl Pts',(-9.51388182535834,0.275436159672599,
10.1416384322799));
#20949=CARTESIAN_POINT('Ctrl Pts',(-9.51642831724057,0.00974174196450768,
10.1541193655281));
#20950=CARTESIAN_POINT('Ctrl Pts',(-9.51645943884197,0.00649459406682937,
10.1542718995425));
#20951=CARTESIAN_POINT('Ctrl Pts',(-9.516475,0.00324729703383339,10.154424433557));
#20952=CARTESIAN_POINT('Ctrl Pts',(-9.516475,3.80718788973236E-13,10.1545769675715));
#20953=CARTESIAN_POINT('Origin',(-8.5,0.,1.24542303242842));
#20954=CARTESIAN_POINT('',(-9.51617051050046,0.000917125635492296,9.49542303242848));
#20955=CARTESIAN_POINT('',(-9.516475,3.07995967097996E-13,9.55457696757151));
#20956=CARTESIAN_POINT('',(-9.516475,1.78524650477582E-12,1.24542303242842));
#20957=CARTESIAN_POINT('Ctrl Pts',(-9.51617051050046,0.000917125635492358,
9.49542303242848));
#20958=CARTESIAN_POINT('Ctrl Pts',(-9.51399210699604,-0.251361202752491,
9.50727128818155));
#20959=CARTESIAN_POINT('Ctrl Pts',(-9.29182487903127,-0.845882765186451,
9.53502688508624));
#20960=CARTESIAN_POINT('Ctrl Pts',(-8.29189791040081,-1.18449019452684,
9.57868982314254));
#20961=CARTESIAN_POINT('Ctrl Pts',(-7.54347150337463,-0.585426497780913,
9.61845817602161));
#20962=CARTESIAN_POINT('Ctrl Pts',(-7.44875116596018,0.10714884380356,9.65027285832483));
#20963=CARTESIAN_POINT('Ctrl Pts',(-7.68125394638234,0.766371873730981,
9.6820875406281));
#20964=CARTESIAN_POINT('Ctrl Pts',(-8.5351536477378,1.20211801487063,9.72185589350713));
#20965=CARTESIAN_POINT('Ctrl Pts',(-9.37873992468116,0.708230622368606,
9.76228561429921));
#20966=CARTESIAN_POINT('Ctrl Pts',(-9.51456966231208,0.18381057644297,9.78680799393966));
#20967=CARTESIAN_POINT('Ctrl Pts',(-9.51485924948736,-0.00024316975562387,
9.79542303242848));
#20968=CARTESIAN_POINT('Ctrl Pts',(-9.516475,3.07995967097996E-13,9.55457696757151));
#20969=CARTESIAN_POINT('Ctrl Pts',(-9.51647500000008,-0.26570662058367,
9.5670579008197));
#20970=CARTESIAN_POINT('Ctrl Pts',(-9.4072746538721,-0.529786878176884,
9.57953883406789));
#20971=CARTESIAN_POINT('Ctrl Pts',(-9.21961691907775,-0.717894780174674,
9.59201976731608));
#20972=CARTESIAN_POINT('Ctrl Pts',(-9.0319591842834,-0.906002682172464,
9.60450070056427));
#20973=CARTESIAN_POINT('Ctrl Pts',(-8.76814132834378,-1.01583545019909,
9.61698163381246));
#20974=CARTESIAN_POINT('Ctrl Pts',(-8.50243547044502,-1.0164720823066,9.62946256706065));
#20975=CARTESIAN_POINT('Ctrl Pts',(-8.23672961254625,-1.0171087144141,9.64194350030884));
#20976=CARTESIAN_POINT('Ctrl Pts',(-7.9723884693333,-0.908541417082734,
9.65442443355703));
#20977=CARTESIAN_POINT('Ctrl Pts',(-7.78383148002335,-0.721334926798541,
9.66690536680522));
#20978=CARTESIAN_POINT('Ctrl Pts',(-7.5952744907134,-0.534128436514349,
9.67938630005342));
#20979=CARTESIAN_POINT('Ctrl Pts',(-7.48480993131701,-0.270574496755657,
9.6918672333016));
#20980=CARTESIAN_POINT('Ctrl Pts',(-7.48353667075686,-0.00487092690815927,
9.7043481665498));
#20981=CARTESIAN_POINT('Ctrl Pts',(-7.48226341019671,0.260832642939339,
9.71682909979799));
#20982=CARTESIAN_POINT('Ctrl Pts',(-7.59019703546757,0.525433154240539,
9.72931003304618));
#20983=CARTESIAN_POINT('Ctrl Pts',(-7.77695120652527,0.714438148393364,
9.74179096629437));
#20984=CARTESIAN_POINT('Ctrl Pts',(-7.96370537758297,0.903443142546189,
9.75427189954256));
#20985=CARTESIAN_POINT('Ctrl Pts',(-8.22699388814843,1.01453885915664,9.76675283279075));
#20986=CARTESIAN_POINT('Ctrl Pts',(-8.49269364459175,1.01644874085989,9.77923376603894));
#20987=CARTESIAN_POINT('Ctrl Pts',(-8.75839340103507,1.01835862256314,9.79171469928713));
#20988=CARTESIAN_POINT('Ctrl Pts',(-9.02325176140405,0.91105928897889,9.80419563253533));
#20989=CARTESIAN_POINT('Ctrl Pts',(-9.21270367535855,0.724758509267337,
9.81667656578352));
#20990=CARTESIAN_POINT('Ctrl Pts',(-9.40215558931306,0.538457729555783,
9.82915749903171));
#20991=CARTESIAN_POINT('Ctrl Pts',(-9.51388182535849,0.275436159672078,
9.8416384322799));
#20992=CARTESIAN_POINT('Ctrl Pts',(-9.51642831724057,0.00974174196396577,
9.85411936552809));
#20993=CARTESIAN_POINT('Ctrl Pts',(-9.51645943884197,0.0064945940664704,
9.85427189954256));
#20994=CARTESIAN_POINT('Ctrl Pts',(-9.516475,0.00324729703365738,9.85442443355703));
#20995=CARTESIAN_POINT('Ctrl Pts',(-9.516475,3.87692313675521E-13,9.8545769675715));
#20996=CARTESIAN_POINT('Origin',(-8.5,0.,1.24542303242842));
#20997=CARTESIAN_POINT('',(-9.51691224954345,-1.40868099694123E-5,9.19542303242848));
#20998=CARTESIAN_POINT('',(-9.516475,2.86079534707011E-13,9.25457696757151));
#20999=CARTESIAN_POINT('',(-9.516475,1.78524650477582E-12,1.24542303242842));
#21000=CARTESIAN_POINT('Ctrl Pts',(-9.51820343362973,-5.56847155661899E-5,
9.19542303242848));
#21001=CARTESIAN_POINT('Ctrl Pts',(-9.51823033311794,-0.0105875877906328,
9.19591990012021));
#21002=CARTESIAN_POINT('Ctrl Pts',(-9.51326527171217,-0.358286048382976,
9.21232410896355));
#21003=CARTESIAN_POINT('Ctrl Pts',(-9.11760907802098,-1.03193145478362,
9.24463565895851));
#21004=CARTESIAN_POINT('Ctrl Pts',(-8.15965436942419,-1.06856717192152,
9.28440401183757));
#21005=CARTESIAN_POINT('Ctrl Pts',(-7.63488434792032,-0.606778290914648,
9.3162186941408));
#21006=CARTESIAN_POINT('Ctrl Pts',(-7.37939961054365,0.0438829842956811,
9.34803337644406));
#21007=CARTESIAN_POINT('Ctrl Pts',(-7.74006457714768,0.932106031371996,
9.38780172932309));
#21008=CARTESIAN_POINT('Ctrl Pts',(-8.87452398480516,1.1427273841981,9.43552375277797));
#21009=CARTESIAN_POINT('Ctrl Pts',(-9.46709300437131,0.511607309487474,
9.47139752047976));
#21010=CARTESIAN_POINT('Ctrl Pts',(-9.5169168081869,0.0873449763227789,
9.49136394702993));
#21011=CARTESIAN_POINT('Ctrl Pts',(-9.51617051050046,0.000917125635492358,
9.49542303242848));
#21012=CARTESIAN_POINT('Ctrl Pts',(-9.516475,3.14969491800281E-13,9.25457696757151));
#21013=CARTESIAN_POINT('Ctrl Pts',(-9.51647500000008,-0.265706620583654,
9.2670579008197));
#21014=CARTESIAN_POINT('Ctrl Pts',(-9.40727465387212,-0.529786878176859,
9.27953883406789));
#21015=CARTESIAN_POINT('Ctrl Pts',(-9.21961691907778,-0.717894780174649,
9.29201976731608));
#21016=CARTESIAN_POINT('Ctrl Pts',(-9.03195918428344,-0.906002682172439,
9.30450070056427));
#21017=CARTESIAN_POINT('Ctrl Pts',(-8.76814132834383,-1.01583545019907,
9.31698163381246));
#21018=CARTESIAN_POINT('Ctrl Pts',(-8.50243547044508,-1.0164720823066,9.32946256706065));
#21019=CARTESIAN_POINT('Ctrl Pts',(-8.23672961254633,-1.01710871441412,
9.34194350030884));
#21020=CARTESIAN_POINT('Ctrl Pts',(-7.97238846933338,-0.908541417082776,
9.35442443355703));
#21021=CARTESIAN_POINT('Ctrl Pts',(-7.78383148002342,-0.721334926798607,
9.36690536680522));
#21022=CARTESIAN_POINT('Ctrl Pts',(-7.59527449071346,-0.534128436514439,
9.37938630005341));
#21023=CARTESIAN_POINT('Ctrl Pts',(-7.48480993131704,-0.27057449675577,
9.3918672333016));
#21024=CARTESIAN_POINT('Ctrl Pts',(-7.48353667075686,-0.0048709269082818,
9.40434816654979));
#21025=CARTESIAN_POINT('Ctrl Pts',(-7.48226341019668,0.260832642939206,
9.41682909979798));
#21026=CARTESIAN_POINT('Ctrl Pts',(-7.5901970354675,0.52543315424041,9.42931003304617));
#21027=CARTESIAN_POINT('Ctrl Pts',(-7.77695120652516,0.714438148393256,
9.44179096629436));
#21028=CARTESIAN_POINT('Ctrl Pts',(-7.96370537758283,0.903443142546102,
9.45427189954255));
#21029=CARTESIAN_POINT('Ctrl Pts',(-8.22699388814826,1.01453885915659,9.46675283279074));
#21030=CARTESIAN_POINT('Ctrl Pts',(-8.49269364459157,1.01644874085988,9.47923376603893));
#21031=CARTESIAN_POINT('Ctrl Pts',(-8.75839340103487,1.01835862256318,9.49171469928712));
#21032=CARTESIAN_POINT('Ctrl Pts',(-9.02325176140386,0.911059288978991,
9.50419563253532));
#21033=CARTESIAN_POINT('Ctrl Pts',(-9.2127036753584,0.724758509267483,9.51667656578351));
#21034=CARTESIAN_POINT('Ctrl Pts',(-9.40215558931294,0.538457729555975,
9.5291574990317));
#21035=CARTESIAN_POINT('Ctrl Pts',(-9.51388182535842,0.275436159672306,
9.54163843227989));
#21036=CARTESIAN_POINT('Ctrl Pts',(-9.51642831724057,0.00974174196420385,
9.55411936552808));
#21037=CARTESIAN_POINT('Ctrl Pts',(-9.51645943884197,0.00649459406660257,
9.55427189954255));
#21038=CARTESIAN_POINT('Ctrl Pts',(-9.516475,0.00324729703368363,9.55442443355703));
#21039=CARTESIAN_POINT('Ctrl Pts',(-9.516475,3.07995967097996E-13,9.55457696757151));
#21040=CARTESIAN_POINT('Origin',(-8.5,0.,1.24542303242842));
#21041=CARTESIAN_POINT('',(-9.516475,2.3721928873646E-13,8.89542303242848));
#21042=CARTESIAN_POINT('',(-9.516475,2.64163102316026E-13,8.95457696757151));
#21043=CARTESIAN_POINT('',(-9.516475,1.78524650477582E-12,1.24542303242842));
#21044=CARTESIAN_POINT('Ctrl Pts',(-9.516475,2.66109245829729E-13,8.89542303242848));
#21045=CARTESIAN_POINT('Ctrl Pts',(-9.51647500000007,-0.265706620583703,
8.90790396567667));
#21046=CARTESIAN_POINT('Ctrl Pts',(-9.40727465387209,-0.529786878176903,
8.92038489892486));
#21047=CARTESIAN_POINT('Ctrl Pts',(-9.21961691907774,-0.717894780174684,
8.93286583217305));
#21048=CARTESIAN_POINT('Ctrl Pts',(-9.03195918428339,-0.906002682172464,
8.94534676542124));
#21049=CARTESIAN_POINT('Ctrl Pts',(-8.76814132834379,-1.01583545019909,
8.95782769866944));
#21050=CARTESIAN_POINT('Ctrl Pts',(-8.50243547044503,-1.0164720823066,8.97030863191763));
#21051=CARTESIAN_POINT('Ctrl Pts',(-8.23672961254628,-1.01710871441411,
8.98278956516581));
#21052=CARTESIAN_POINT('Ctrl Pts',(-7.97238846933334,-0.90854141708275,
8.99527049841401));
#21053=CARTESIAN_POINT('Ctrl Pts',(-7.78383148002338,-0.721334926798573,
9.0077514316622));
#21054=CARTESIAN_POINT('Ctrl Pts',(-7.59527449071343,-0.534128436514395,
9.02023236491039));
#21055=CARTESIAN_POINT('Ctrl Pts',(-7.48480993131703,-0.270574496755721,
9.03271329815858));
#21056=CARTESIAN_POINT('Ctrl Pts',(-7.48353667075686,-0.00487092690823294,
9.04519423140677));
#21057=CARTESIAN_POINT('Ctrl Pts',(-7.48226341019669,0.260832642939255,
9.05767516465496));
#21058=CARTESIAN_POINT('Ctrl Pts',(-7.59019703546752,0.525433154240453,
9.07015609790315));
#21059=CARTESIAN_POINT('Ctrl Pts',(-7.7769512065252,0.714438148393291,9.08263703115134));
#21060=CARTESIAN_POINT('Ctrl Pts',(-7.96370537758287,0.903443142546128,
9.09511796439953));
#21061=CARTESIAN_POINT('Ctrl Pts',(-8.22699388814831,1.0145388591566,9.10759889764772));
#21062=CARTESIAN_POINT('Ctrl Pts',(-8.49269364459162,1.01644874085989,9.12007983089591));
#21063=CARTESIAN_POINT('Ctrl Pts',(-8.75839340103493,1.01835862256317,9.1325607641441));
#21064=CARTESIAN_POINT('Ctrl Pts',(-9.02325176140391,0.911059288978966,
9.14504169739229));
#21065=CARTESIAN_POINT('Ctrl Pts',(-9.21270367535844,0.724758509267449,
9.15752263064048));
#21066=CARTESIAN_POINT('Ctrl Pts',(-9.40215558931297,0.538457729555932,
9.17000356388867));
#21067=CARTESIAN_POINT('Ctrl Pts',(-9.51388182535843,0.275436159672257,
9.18248449713686));
#21068=CARTESIAN_POINT('Ctrl Pts',(-9.51642831724057,0.009741741964155,
9.19496543038505));
#21069=CARTESIAN_POINT('Ctrl Pts',(-9.51645943884197,0.00649459406656334,
9.19511796439953));
#21070=CARTESIAN_POINT('Ctrl Pts',(-9.516475,0.00324729703365397,9.19527049841401));
#21071=CARTESIAN_POINT('Ctrl Pts',(-9.516475,2.88025678220714E-13,9.19542303242848));
#21072=CARTESIAN_POINT('Ctrl Pts',(-9.516475,2.64163102316026E-13,8.95457696757151));
#21073=CARTESIAN_POINT('Ctrl Pts',(-9.51647500000007,-0.265706620583705,
8.9670579008197));
#21074=CARTESIAN_POINT('Ctrl Pts',(-9.40727465387209,-0.529786878176905,
8.97953883406789));
#21075=CARTESIAN_POINT('Ctrl Pts',(-9.21961691907774,-0.717894780174685,
8.99201976731608));
#21076=CARTESIAN_POINT('Ctrl Pts',(-9.03195918428339,-0.906002682172465,
9.00450070056427));
#21077=CARTESIAN_POINT('Ctrl Pts',(-8.76814132834378,-1.01583545019909,
9.01698163381246));
#21078=CARTESIAN_POINT('Ctrl Pts',(-8.50243547044503,-1.0164720823066,9.02946256706065));
#21079=CARTESIAN_POINT('Ctrl Pts',(-8.23672961254628,-1.01710871441411,
9.04194350030884));
#21080=CARTESIAN_POINT('Ctrl Pts',(-7.97238846933333,-0.908541417082749,
9.05442443355703));
#21081=CARTESIAN_POINT('Ctrl Pts',(-7.78383148002338,-0.721334926798572,
9.06690536680522));
#21082=CARTESIAN_POINT('Ctrl Pts',(-7.59527449071343,-0.534128436514394,
9.07938630005341));
#21083=CARTESIAN_POINT('Ctrl Pts',(-7.48480993131703,-0.270574496755719,
9.0918672333016));
#21084=CARTESIAN_POINT('Ctrl Pts',(-7.48353667075686,-0.004870926908231,
9.10434816654979));
#21085=CARTESIAN_POINT('Ctrl Pts',(-7.48226341019669,0.260832642939257,
9.11682909979798));
#21086=CARTESIAN_POINT('Ctrl Pts',(-7.59019703546753,0.525433154240455,
9.12931003304618));
#21087=CARTESIAN_POINT('Ctrl Pts',(-7.7769512065252,0.714438148393292,9.14179096629437));
#21088=CARTESIAN_POINT('Ctrl Pts',(-7.96370537758287,0.903443142546129,
9.15427189954256));
#21089=CARTESIAN_POINT('Ctrl Pts',(-8.22699388814831,1.0145388591566,9.16675283279075));
#21090=CARTESIAN_POINT('Ctrl Pts',(-8.49269364459162,1.01644874085989,9.17923376603894));
#21091=CARTESIAN_POINT('Ctrl Pts',(-8.75839340103493,1.01835862256317,9.19171469928713));
#21092=CARTESIAN_POINT('Ctrl Pts',(-9.02325176140391,0.911059288978965,
9.20419563253532));
#21093=CARTESIAN_POINT('Ctrl Pts',(-9.21270367535844,0.724758509267448,
9.21667656578351));
#21094=CARTESIAN_POINT('Ctrl Pts',(-9.40215558931297,0.53845772955593,9.2291574990317));
#21095=CARTESIAN_POINT('Ctrl Pts',(-9.51388182535844,0.275436159672255,
9.24163843227989));
#21096=CARTESIAN_POINT('Ctrl Pts',(-9.51642831724057,0.00974174196415305,
9.25411936552808));
#21097=CARTESIAN_POINT('Ctrl Pts',(-9.51645943884197,0.00649459406657102,
9.25427189954256));
#21098=CARTESIAN_POINT('Ctrl Pts',(-9.516475,0.0032472970336713,9.25442443355703));
#21099=CARTESIAN_POINT('Ctrl Pts',(-9.516475,3.14969491800281E-13,9.25457696757151));
#21100=CARTESIAN_POINT('Origin',(-8.5,0.,1.24542303242842));
#21101=CARTESIAN_POINT('',(-9.51616255555685,0.000140128590502373,8.59542303242849));
#21102=CARTESIAN_POINT('',(-9.516475,2.42246669925041E-13,8.65457696757151));
#21103=CARTESIAN_POINT('',(-9.516475,1.78524650477582E-12,1.24542303242842));
#21104=CARTESIAN_POINT('Ctrl Pts',(-9.516475,2.15302856345474E-13,8.59542303242849));
#21105=CARTESIAN_POINT('Ctrl Pts',(-9.51647500000006,-0.265706620583753,
8.60790396567667));
#21106=CARTESIAN_POINT('Ctrl Pts',(-9.40727465387207,-0.529786878176948,
8.62038489892487));
#21107=CARTESIAN_POINT('Ctrl Pts',(-9.21961691907771,-0.71789478017472,
8.63286583217306));
#21108=CARTESIAN_POINT('Ctrl Pts',(-9.03195918428335,-0.906002682172491,
8.64534676542125));
#21109=CARTESIAN_POINT('Ctrl Pts',(-8.76814132834373,-1.0158354501991,8.65782769866944));
#21110=CARTESIAN_POINT('Ctrl Pts',(-8.50243547044498,-1.0164720823066,8.67030863191763));
#21111=CARTESIAN_POINT('Ctrl Pts',(-8.23672961254623,-1.0171087144141,8.68278956516582));
#21112=CARTESIAN_POINT('Ctrl Pts',(-7.97238846933329,-0.908541417082724,
8.69527049841401));
#21113=CARTESIAN_POINT('Ctrl Pts',(-7.78383148002335,-0.721334926798537,
8.7077514316622));
#21114=CARTESIAN_POINT('Ctrl Pts',(-7.5952744907134,-0.53412843651435,8.72023236491039));
#21115=CARTESIAN_POINT('Ctrl Pts',(-7.48480993131701,-0.27057449675567,
8.73271329815858));
#21116=CARTESIAN_POINT('Ctrl Pts',(-7.48353667075686,-0.00487092690818213,
8.74519423140677));
#21117=CARTESIAN_POINT('Ctrl Pts',(-7.4822634101967,0.260832642939306,8.75767516465496));
#21118=CARTESIAN_POINT('Ctrl Pts',(-7.59019703546755,0.525433154240499,
8.77015609790315));
#21119=CARTESIAN_POINT('Ctrl Pts',(-7.77695120652523,0.714438148393327,
8.78263703115134));
#21120=CARTESIAN_POINT('Ctrl Pts',(-7.96370537758292,0.903443142546155,
8.79511796439953));
#21121=CARTESIAN_POINT('Ctrl Pts',(-8.22699388814836,1.01453885915661,8.80759889764772));
#21122=CARTESIAN_POINT('Ctrl Pts',(-8.49269364459167,1.01644874085989,8.82007983089591));
#21123=CARTESIAN_POINT('Ctrl Pts',(-8.75839340103498,1.01835862256316,8.8325607641441));
#21124=CARTESIAN_POINT('Ctrl Pts',(-9.02325176140395,0.91105928897894,8.8450416973923));
#21125=CARTESIAN_POINT('Ctrl Pts',(-9.21270367535847,0.724758509267413,
8.85752263064049));
#21126=CARTESIAN_POINT('Ctrl Pts',(-9.40215558931299,0.538457729555887,
8.87000356388867));
#21127=CARTESIAN_POINT('Ctrl Pts',(-9.51388182535845,0.275436159672206,
8.88248449713687));
#21128=CARTESIAN_POINT('Ctrl Pts',(-9.51642831724057,0.00974174196410419,
8.89496543038506));
#21129=CARTESIAN_POINT('Ctrl Pts',(-9.51645943884197,0.00649459406652216,
8.89511796439953));
#21130=CARTESIAN_POINT('Ctrl Pts',(-9.516475,0.00324729703362244,8.89527049841401));
#21131=CARTESIAN_POINT('Ctrl Pts',(-9.516475,2.66109245829729E-13,8.89542303242848));
#21132=CARTESIAN_POINT('Ctrl Pts',(-9.516475,2.71136627018311E-13,8.65457696757151));
#21133=CARTESIAN_POINT('Ctrl Pts',(-9.51647500000007,-0.265706620583707,
8.6670579008197));
#21134=CARTESIAN_POINT('Ctrl Pts',(-9.40727465387209,-0.529786878176917,
8.67953883406789));
#21135=CARTESIAN_POINT('Ctrl Pts',(-9.21961691907773,-0.717894780174701,
8.69201976731608));
#21136=CARTESIAN_POINT('Ctrl Pts',(-9.03195918428337,-0.906002682172484,
8.70450070056427));
#21137=CARTESIAN_POINT('Ctrl Pts',(-8.76814132834374,-1.0158354501991,8.71698163381246));
#21138=CARTESIAN_POINT('Ctrl Pts',(-8.50243547044498,-1.0164720823066,8.72946256706065));
#21139=CARTESIAN_POINT('Ctrl Pts',(-8.23672961254622,-1.01710871441409,
8.74194350030884));
#21140=CARTESIAN_POINT('Ctrl Pts',(-7.97238846933327,-0.908541417082715,
8.75442443355703));
#21141=CARTESIAN_POINT('Ctrl Pts',(-7.78383148002333,-0.721334926798515,
8.76690536680523));
#21142=CARTESIAN_POINT('Ctrl Pts',(-7.59527449071338,-0.534128436514316,
8.77938630005342));
#21143=CARTESIAN_POINT('Ctrl Pts',(-7.484809931317,-0.27057449675562,8.79186723330161));
#21144=CARTESIAN_POINT('Ctrl Pts',(-7.48353667075686,-0.00487092690812241,
8.8043481665498));
#21145=CARTESIAN_POINT('Ctrl Pts',(-7.48226341019672,0.260832642939375,
8.81682909979799));
#21146=CARTESIAN_POINT('Ctrl Pts',(-7.59019703546759,0.525433154240572,
8.82931003304618));
#21147=CARTESIAN_POINT('Ctrl Pts',(-7.7769512065253,0.71443814839339,8.84179096629437));
#21148=CARTESIAN_POINT('Ctrl Pts',(-7.963705377583,0.903443142546209,8.85427189954256));
#21149=CARTESIAN_POINT('Ctrl Pts',(-8.22699388814847,1.01453885915665,8.86675283279075));
#21150=CARTESIAN_POINT('Ctrl Pts',(-8.49269364459179,1.01644874085989,8.87923376603894));
#21151=CARTESIAN_POINT('Ctrl Pts',(-8.7583934010351,1.01835862256313,8.89171469928714));
#21152=CARTESIAN_POINT('Ctrl Pts',(-9.02325176140408,0.911059288978871,
8.90419563253533));
#21153=CARTESIAN_POINT('Ctrl Pts',(-9.21270367535858,0.724758509267311,
8.91667656578352));
#21154=CARTESIAN_POINT('Ctrl Pts',(-9.40215558931308,0.53845772955575,8.92915749903171));
#21155=CARTESIAN_POINT('Ctrl Pts',(-9.5138818253585,0.275436159672041,8.9416384322799));
#21156=CARTESIAN_POINT('Ctrl Pts',(-9.51642831724057,0.00974174196392891,
8.95411936552809));
#21157=CARTESIAN_POINT('Ctrl Pts',(-9.51645943884197,0.00649459406640466,
8.95427189954256));
#21158=CARTESIAN_POINT('Ctrl Pts',(-9.516475,0.00324729703356276,8.95442443355704));
#21159=CARTESIAN_POINT('Ctrl Pts',(-9.516475,2.64163102316026E-13,8.95457696757151));
#21160=CARTESIAN_POINT('Origin',(-8.5,0.,1.24542303242842));
#21161=CARTESIAN_POINT('',(-9.51660746771427,4.7561522507508E-5,8.29542303242849));
#21162=CARTESIAN_POINT('',(-9.51622101958584,6.09791478407872E-5,8.35457696757151));
#21163=CARTESIAN_POINT('',(-9.516475,1.78524650477582E-12,1.24542303242842));
#21164=CARTESIAN_POINT('Ctrl Pts',(-9.51755758975633,0.000388695593763897,
8.29542303242849));
#21165=CARTESIAN_POINT('Ctrl Pts',(-9.5169508547152,-0.131482241807455,
8.30163408881522));
#21166=CARTESIAN_POINT('Ctrl Pts',(-9.45475814244576,-0.43297838743787,
8.31579881577777));
#21167=CARTESIAN_POINT('Ctrl Pts',(-9.06669282573335,-0.967744899455822,
8.34587088389194));
#21168=CARTESIAN_POINT('Ctrl Pts',(-8.12407617387874,-1.14236805696769,
8.385639236771));
#21169=CARTESIAN_POINT('Ctrl Pts',(-7.3354977594041,-0.300047698604244,
8.43336126022585));
#21170=CARTESIAN_POINT('Ctrl Pts',(-7.61818561524077,0.816349017112872,
8.48108328368072));
#21171=CARTESIAN_POINT('Ctrl Pts',(-8.70950569765978,1.18414587464495,8.52880530713558));
#21172=CARTESIAN_POINT('Ctrl Pts',(-9.42871558275495,0.608006666036184,
8.56691855671817));
#21173=CARTESIAN_POINT('Ctrl Pts',(-9.51570104621182,0.135102786595141,
8.58912446514914));
#21174=CARTESIAN_POINT('Ctrl Pts',(-9.51489988985996,0.000706423072568199,
8.59542303242848));
#21175=CARTESIAN_POINT('Ctrl Pts',(-9.516475,2.20330237534056E-13,8.35457696757151));
#21176=CARTESIAN_POINT('Ctrl Pts',(-9.51647500000006,-0.265706620583758,
8.3670579008197));
#21177=CARTESIAN_POINT('Ctrl Pts',(-9.40727465387206,-0.529786878176963,
8.37953883406789));
#21178=CARTESIAN_POINT('Ctrl Pts',(-9.21961691907769,-0.717894780174737,
8.39201976731608));
#21179=CARTESIAN_POINT('Ctrl Pts',(-9.03195918428332,-0.90600268217251,
8.40450070056427));
#21180=CARTESIAN_POINT('Ctrl Pts',(-8.76814132834369,-1.01583545019911,
8.41698163381246));
#21181=CARTESIAN_POINT('Ctrl Pts',(-8.50243547044493,-1.0164720823066,8.42946256706066));
#21182=CARTESIAN_POINT('Ctrl Pts',(-8.23672961254617,-1.01710871441408,
8.44194350030885));
#21183=CARTESIAN_POINT('Ctrl Pts',(-7.97238846933322,-0.908541417082688,
8.45442443355704));
#21184=CARTESIAN_POINT('Ctrl Pts',(-7.78383148002329,-0.72133492679848,
8.46690536680523));
#21185=CARTESIAN_POINT('Ctrl Pts',(-7.59527449071336,-0.534128436514271,
8.47938630005342));
#21186=CARTESIAN_POINT('Ctrl Pts',(-7.48480993131698,-0.27057449675557,
8.49186723330161));
#21187=CARTESIAN_POINT('Ctrl Pts',(-7.48353667075686,-0.0048709269080716,
8.5043481665498));
#21188=CARTESIAN_POINT('Ctrl Pts',(-7.48226341019673,0.260832642939426,
8.51682909979799));
#21189=CARTESIAN_POINT('Ctrl Pts',(-7.59019703546762,0.525433154240617,
8.52931003304618));
#21190=CARTESIAN_POINT('Ctrl Pts',(-7.77695120652533,0.714438148393426,
8.54179096629437));
#21191=CARTESIAN_POINT('Ctrl Pts',(-7.96370537758305,0.903443142546235,
8.55427189954256));
#21192=CARTESIAN_POINT('Ctrl Pts',(-8.22699388814852,1.01453885915666,8.56675283279075));
#21193=CARTESIAN_POINT('Ctrl Pts',(-8.49269364459184,1.01644874085989,8.57923376603895));
#21194=CARTESIAN_POINT('Ctrl Pts',(-8.75839340103515,1.01835862256311,8.59171469928714));
#21195=CARTESIAN_POINT('Ctrl Pts',(-9.02325176140413,0.911059288978845,
8.60419563253533));
#21196=CARTESIAN_POINT('Ctrl Pts',(-9.21270367535861,0.724758509267275,
8.61667656578352));
#21197=CARTESIAN_POINT('Ctrl Pts',(-9.4021555893131,0.538457729555705,8.62915749903171));
#21198=CARTESIAN_POINT('Ctrl Pts',(-9.51388182535851,0.27543615967199,8.6416384322799));
#21199=CARTESIAN_POINT('Ctrl Pts',(-9.51642831724058,0.00974174196387811,
8.65411936552809));
#21200=CARTESIAN_POINT('Ctrl Pts',(-9.51645943884197,0.00649459406637311,
8.65427189954256));
#21201=CARTESIAN_POINT('Ctrl Pts',(-9.516475,0.00324729703355043,8.65442443355704));
#21202=CARTESIAN_POINT('Ctrl Pts',(-9.516475,2.71136627018311E-13,8.65457696757151));
#21203=CARTESIAN_POINT('Origin',(-8.5,0.,1.24542303242842));
#21204=CARTESIAN_POINT('',(-9.516475,1.71469991563504E-13,7.99542303242849));
#21205=CARTESIAN_POINT('',(-9.5164935018391,1.69134969809854E-5,8.05457696757151));
#21206=CARTESIAN_POINT('',(-9.516475,1.78524650477582E-12,1.24542303242842));
#21207=CARTESIAN_POINT('Ctrl Pts',(-9.516475,1.71469991563504E-13,7.99542303242849));
#21208=CARTESIAN_POINT('Ctrl Pts',(-9.51647500000004,-0.265706620583807,
8.00790396567668));
#21209=CARTESIAN_POINT('Ctrl Pts',(-9.40727465387203,-0.529786878177006,
8.02038489892487));
#21210=CARTESIAN_POINT('Ctrl Pts',(-9.21961691907766,-0.717894780174771,
8.03286583217306));
#21211=CARTESIAN_POINT('Ctrl Pts',(-9.03195918428328,-0.906002682172536,
8.04534676542125));
#21212=CARTESIAN_POINT('Ctrl Pts',(-8.76814132834364,-1.01583545019913,
8.05782769866944));
#21213=CARTESIAN_POINT('Ctrl Pts',(-8.50243547044488,-1.0164720823066,8.07030863191763));
#21214=CARTESIAN_POINT('Ctrl Pts',(-8.23672961254612,-1.01710871441407,
8.08278956516583));
#21215=CARTESIAN_POINT('Ctrl Pts',(-7.97238846933318,-0.908541417082663,
8.09527049841401));
#21216=CARTESIAN_POINT('Ctrl Pts',(-7.78383148002326,-0.721334926798445,
8.10775143166221));
#21217=CARTESIAN_POINT('Ctrl Pts',(-7.59527449071333,-0.534128436514227,
8.1202323649104));
#21218=CARTESIAN_POINT('Ctrl Pts',(-7.48480993131697,-0.270574496755521,
8.13271329815859));
#21219=CARTESIAN_POINT('Ctrl Pts',(-7.48353667075686,-0.00487092690802274,
8.14519423140678));
#21220=CARTESIAN_POINT('Ctrl Pts',(-7.48226341019674,0.260832642939475,
8.15767516465497));
#21221=CARTESIAN_POINT('Ctrl Pts',(-7.59019703546764,0.525433154240661,
8.17015609790316));
#21222=CARTESIAN_POINT('Ctrl Pts',(-7.77695120652537,0.714438148393461,
8.18263703115135));
#21223=CARTESIAN_POINT('Ctrl Pts',(-7.96370537758309,0.903443142546261,
8.19511796439954));
#21224=CARTESIAN_POINT('Ctrl Pts',(-8.22699388814857,1.01453885915667,8.20759889764773));
#21225=CARTESIAN_POINT('Ctrl Pts',(-8.49269364459189,1.01644874085989,8.22007983089592));
#21226=CARTESIAN_POINT('Ctrl Pts',(-8.7583934010352,1.0183586225631,8.23256076414412));
#21227=CARTESIAN_POINT('Ctrl Pts',(-9.02325176140417,0.91105928897882,8.2450416973923));
#21228=CARTESIAN_POINT('Ctrl Pts',(-9.21270367535865,0.724758509267241,
8.2575226306405));
#21229=CARTESIAN_POINT('Ctrl Pts',(-9.40215558931313,0.538457729555662,
8.27000356388869));
#21230=CARTESIAN_POINT('Ctrl Pts',(-9.51388182535852,0.275436159671942,
8.28248449713688));
#21231=CARTESIAN_POINT('Ctrl Pts',(-9.51642831724058,0.00974174196382925,
8.29496543038507));
#21232=CARTESIAN_POINT('Ctrl Pts',(-9.51645943884197,0.00649459406632425,
8.29511796439954));
#21233=CARTESIAN_POINT('Ctrl Pts',(-9.516475,0.00324729703350157,8.29527049841401));
#21234=CARTESIAN_POINT('Ctrl Pts',(-9.516475,2.22276381047759E-13,8.29542303242848));
#21235=CARTESIAN_POINT('Ctrl Pts',(-9.51728273352218,0.000738391526869241,
8.05457696757151));
#21236=CARTESIAN_POINT('Ctrl Pts',(-9.51495287138475,-0.289530015017073,
8.06824838978708));
#21237=CARTESIAN_POINT('Ctrl Pts',(-9.23304354846487,-0.921572807151517,
8.09782715315426));
#21238=CARTESIAN_POINT('Ctrl Pts',(-8.15787155631456,-1.15294042718917,
8.14331325767308));
#21239=CARTESIAN_POINT('Ctrl Pts',(-7.48282485956976,-0.472255950572485,
8.18308161055214));
#21240=CARTESIAN_POINT('Ctrl Pts',(-7.4678884532851,0.226607018726978,8.21489629285537));
#21241=CARTESIAN_POINT('Ctrl Pts',(-7.77421828515018,0.854933828755218,
8.24671097515861));
#21242=CARTESIAN_POINT('Ctrl Pts',(-8.67232841342475,1.19022116371383,8.28647932803768));
#21243=CARTESIAN_POINT('Ctrl Pts',(-9.41868698066376,0.629620601799731,
8.32508588236723));
#21244=CARTESIAN_POINT('Ctrl Pts',(-9.51557266316435,0.145416359173903,
8.34778509554518));
#21245=CARTESIAN_POINT('Ctrl Pts',(-9.51500553128436,0.000352810471975287,
8.35457696757151));
#21246=CARTESIAN_POINT('Origin',(-8.5,0.,1.24542303242842));
#21247=CARTESIAN_POINT('',(-9.516475,1.49553559172519E-13,7.69542303242849));
#21248=CARTESIAN_POINT('',(-9.516475,1.76497372752086E-13,7.75457696757151));
#21249=CARTESIAN_POINT('',(-9.516475,1.78524650477582E-12,1.24542303242842));
#21250=CARTESIAN_POINT('Ctrl Pts',(-9.516475,1.78443516265789E-13,7.69542303242849));
#21251=CARTESIAN_POINT('Ctrl Pts',(-9.51647500000005,-0.2657066205838,7.70790396567668));
#21252=CARTESIAN_POINT('Ctrl Pts',(-9.40727465387204,-0.529786878177,7.72038489892487));
#21253=CARTESIAN_POINT('Ctrl Pts',(-9.21961691907766,-0.717894780174766,
7.73286583217306));
#21254=CARTESIAN_POINT('Ctrl Pts',(-9.03195918428328,-0.906002682172532,
7.74534676542125));
#21255=CARTESIAN_POINT('Ctrl Pts',(-8.76814132834365,-1.01583545019913,
7.75782769866944));
#21256=CARTESIAN_POINT('Ctrl Pts',(-8.50243547044489,-1.0164720823066,7.77030863191763));
#21257=CARTESIAN_POINT('Ctrl Pts',(-8.23672961254612,-1.01710871441407,
7.78278956516582));
#21258=CARTESIAN_POINT('Ctrl Pts',(-7.97238846933319,-0.908541417082667,
7.79527049841401));
#21259=CARTESIAN_POINT('Ctrl Pts',(-7.78383148002326,-0.72133492679845,
7.80775143166221));
#21260=CARTESIAN_POINT('Ctrl Pts',(-7.59527449071333,-0.534128436514233,
7.8202323649104));
#21261=CARTESIAN_POINT('Ctrl Pts',(-7.48480993131697,-0.270574496755528,
7.83271329815859));
#21262=CARTESIAN_POINT('Ctrl Pts',(-7.48353667075686,-0.00487092690802972,
7.84519423140678));
#21263=CARTESIAN_POINT('Ctrl Pts',(-7.48226341019674,0.260832642939468,
7.85767516465497));
#21264=CARTESIAN_POINT('Ctrl Pts',(-7.59019703546764,0.525433154240655,
7.87015609790316));
#21265=CARTESIAN_POINT('Ctrl Pts',(-7.77695120652536,0.714438148393456,
7.88263703115135));
#21266=CARTESIAN_POINT('Ctrl Pts',(-7.96370537758309,0.903443142546258,
7.89511796439954));
#21267=CARTESIAN_POINT('Ctrl Pts',(-8.22699388814856,1.01453885915667,7.90759889764773));
#21268=CARTESIAN_POINT('Ctrl Pts',(-8.49269364459188,1.01644874085989,7.92007983089592));
#21269=CARTESIAN_POINT('Ctrl Pts',(-8.7583934010352,1.0183586225631,7.93256076414411));
#21270=CARTESIAN_POINT('Ctrl Pts',(-9.02325176140416,0.911059288978824,
7.94504169739231));
#21271=CARTESIAN_POINT('Ctrl Pts',(-9.21270367535864,0.724758509267246,
7.9575226306405));
#21272=CARTESIAN_POINT('Ctrl Pts',(-9.40215558931313,0.538457729555668,
7.97000356388869));
#21273=CARTESIAN_POINT('Ctrl Pts',(-9.51388182535852,0.275436159671948,
7.98248449713688));
#21274=CARTESIAN_POINT('Ctrl Pts',(-9.51642831724058,0.00974174196383622,
7.99496543038507));
#21275=CARTESIAN_POINT('Ctrl Pts',(-9.51645943884197,0.00649459406631196,
7.99511796439954));
#21276=CARTESIAN_POINT('Ctrl Pts',(-9.516475,0.00324729703347002,7.99527049841402));
#21277=CARTESIAN_POINT('Ctrl Pts',(-9.516475,1.71469991563504E-13,7.99542303242849));
#21278=CARTESIAN_POINT('Ctrl Pts',(-9.516475,1.76497372752086E-13,7.75457696757151));
#21279=CARTESIAN_POINT('Ctrl Pts',(-9.51647500000005,-0.265706620583783,
7.7670579008197));
#21280=CARTESIAN_POINT('Ctrl Pts',(-9.40727465387205,-0.529786878176964,
7.77953883406789));
#21281=CARTESIAN_POINT('Ctrl Pts',(-9.2196169190777,-0.717894780174727,
7.79201976731608));
#21282=CARTESIAN_POINT('Ctrl Pts',(-9.03195918428335,-0.906002682172489,
7.80450070056427));
#21283=CARTESIAN_POINT('Ctrl Pts',(-8.76814132834375,-1.0158354501991,7.81698163381246));
#21284=CARTESIAN_POINT('Ctrl Pts',(-8.502435470445,-1.0164720823066,7.82946256706065));
#21285=CARTESIAN_POINT('Ctrl Pts',(-8.23672961254626,-1.0171087144141,7.84194350030884));
#21286=CARTESIAN_POINT('Ctrl Pts',(-7.97238846933333,-0.908541417082742,
7.85442443355703));
#21287=CARTESIAN_POINT('Ctrl Pts',(-7.78383148002338,-0.721334926798571,
7.86690536680522));
#21288=CARTESIAN_POINT('Ctrl Pts',(-7.59527449071344,-0.5341284365144,7.87938630005341));
#21289=CARTESIAN_POINT('Ctrl Pts',(-7.48480993131703,-0.270574496755737,
7.8918672333016));
#21290=CARTESIAN_POINT('Ctrl Pts',(-7.48353667075686,-0.00487092690825889,
7.90434816654979));
#21291=CARTESIAN_POINT('Ctrl Pts',(-7.48226341019668,0.26083264293922,7.91682909979798));
#21292=CARTESIAN_POINT('Ctrl Pts',(-7.5901970354675,0.525433154240411,7.92931003304617));
#21293=CARTESIAN_POINT('Ctrl Pts',(-7.77695120652516,0.714438148393252,
7.94179096629436));
#21294=CARTESIAN_POINT('Ctrl Pts',(-7.96370537758282,0.903443142546093,
7.95427189954255));
#21295=CARTESIAN_POINT('Ctrl Pts',(-8.22699388814824,1.01453885915658,7.96675283279074));
#21296=CARTESIAN_POINT('Ctrl Pts',(-8.49269364459153,1.01644874085988,7.97923376603893));
#21297=CARTESIAN_POINT('Ctrl Pts',(-8.75839340103483,1.01835862256319,7.99171469928712));
#21298=CARTESIAN_POINT('Ctrl Pts',(-9.02325176140381,0.911059288979017,
8.00419563253531));
#21299=CARTESIAN_POINT('Ctrl Pts',(-9.21270367535836,0.724758509267528,
8.0166765657835));
#21300=CARTESIAN_POINT('Ctrl Pts',(-9.4021555893129,0.538457729556039,8.02915749903169));
#21301=CARTESIAN_POINT('Ctrl Pts',(-9.5138818253584,0.275436159672388,8.04163843227988));
#21302=CARTESIAN_POINT('Ctrl Pts',(-9.51642831724057,0.0097417419642965,
8.05411936552807));
#21303=CARTESIAN_POINT('Ctrl Pts',(-9.51645943884197,0.00649459406663744,
8.05427189954255));
#21304=CARTESIAN_POINT('Ctrl Pts',(-9.516475,0.00324729703366067,8.05442443355703));
#21305=CARTESIAN_POINT('Ctrl Pts',(-9.516475,2.27303762236341E-13,8.05457696757151));
#21306=CARTESIAN_POINT('Origin',(-8.5,0.,1.24542303242842));
#21307=CARTESIAN_POINT('',(-9.516475,1.27637126781534E-13,7.39542303242849));
#21308=CARTESIAN_POINT('',(-9.516475,1.54580940361101E-13,7.45457696757151));
#21309=CARTESIAN_POINT('',(-9.516475,1.78524650477582E-12,1.24542303242842));
#21310=CARTESIAN_POINT('Ctrl Pts',(-9.516475,1.56527083874804E-13,7.39542303242849));
#21311=CARTESIAN_POINT('Ctrl Pts',(-9.51647500000004,-0.265706620583803,
7.40790396567668));
#21312=CARTESIAN_POINT('Ctrl Pts',(-9.40727465387204,-0.529786878176982,
7.42038489892487));
#21313=CARTESIAN_POINT('Ctrl Pts',(-9.21961691907769,-0.717894780174741,
7.43286583217306));
#21314=CARTESIAN_POINT('Ctrl Pts',(-9.03195918428333,-0.9060026821725,7.44534676542125));
#21315=CARTESIAN_POINT('Ctrl Pts',(-8.76814132834373,-1.0158354501991,7.45782769866944));
#21316=CARTESIAN_POINT('Ctrl Pts',(-8.50243547044498,-1.0164720823066,7.47030863191763));
#21317=CARTESIAN_POINT('Ctrl Pts',(-8.23672961254624,-1.01710871441409,
7.48278956516582));
#21318=CARTESIAN_POINT('Ctrl Pts',(-7.97238846933331,-0.908541417082732,
7.49527049841401));
#21319=CARTESIAN_POINT('Ctrl Pts',(-7.78383148002337,-0.721334926798557,
7.5077514316622));
#21320=CARTESIAN_POINT('Ctrl Pts',(-7.59527449071343,-0.534128436514382,
7.52023236491039));
#21321=CARTESIAN_POINT('Ctrl Pts',(-7.48480993131703,-0.270574496755717,
7.53271329815858));
#21322=CARTESIAN_POINT('Ctrl Pts',(-7.48353667075686,-0.00487092690823892,
7.54519423140677));
#21323=CARTESIAN_POINT('Ctrl Pts',(-7.48226341019669,0.26083264293924,7.55767516465496));
#21324=CARTESIAN_POINT('Ctrl Pts',(-7.59019703546751,0.525433154240429,
7.57015609790315));
#21325=CARTESIAN_POINT('Ctrl Pts',(-7.77695120652517,0.714438148393266,
7.58263703115134));
#21326=CARTESIAN_POINT('Ctrl Pts',(-7.96370537758284,0.903443142546103,
7.59511796439953));
#21327=CARTESIAN_POINT('Ctrl Pts',(-8.22699388814826,1.01453885915658,7.60759889764772));
#21328=CARTESIAN_POINT('Ctrl Pts',(-8.49269364459155,1.01644874085988,7.62007983089591));
#21329=CARTESIAN_POINT('Ctrl Pts',(-8.75839340103485,1.01835862256319,7.6325607641441));
#21330=CARTESIAN_POINT('Ctrl Pts',(-9.02325176140383,0.911059288979007,
7.64504169739229));
#21331=CARTESIAN_POINT('Ctrl Pts',(-9.21270367535837,0.724758509267514,
7.65752263064048));
#21332=CARTESIAN_POINT('Ctrl Pts',(-9.40215558931291,0.538457729556021,
7.67000356388867));
#21333=CARTESIAN_POINT('Ctrl Pts',(-9.5138818253584,0.275436159672368,7.68248449713686));
#21334=CARTESIAN_POINT('Ctrl Pts',(-9.51642831724057,0.00974174196427653,
7.69496543038505));
#21335=CARTESIAN_POINT('Ctrl Pts',(-9.51645943884197,0.00649459406660784,
7.69511796439953));
#21336=CARTESIAN_POINT('Ctrl Pts',(-9.516475,0.00324729703362146,7.69527049841401));
#21337=CARTESIAN_POINT('Ctrl Pts',(-9.516475,1.78443516265789E-13,7.69542303242849));
#21338=CARTESIAN_POINT('Ctrl Pts',(-9.516475,1.54580940361101E-13,7.45457696757151));
#21339=CARTESIAN_POINT('Ctrl Pts',(-9.51647500000004,-0.265706620583805,
7.4670579008197));
#21340=CARTESIAN_POINT('Ctrl Pts',(-9.40727465387204,-0.529786878176983,
7.47953883406789));
#21341=CARTESIAN_POINT('Ctrl Pts',(-9.21961691907768,-0.717894780174742,
7.49201976731608));
#21342=CARTESIAN_POINT('Ctrl Pts',(-9.03195918428333,-0.906002682172501,
7.50450070056427));
#21343=CARTESIAN_POINT('Ctrl Pts',(-8.76814132834372,-1.0158354501991,7.51698163381246));
#21344=CARTESIAN_POINT('Ctrl Pts',(-8.50243547044498,-1.0164720823066,7.52946256706065));
#21345=CARTESIAN_POINT('Ctrl Pts',(-8.23672961254623,-1.01710871441409,
7.54194350030884));
#21346=CARTESIAN_POINT('Ctrl Pts',(-7.97238846933331,-0.908541417082731,
7.55442443355703));
#21347=CARTESIAN_POINT('Ctrl Pts',(-7.78383148002337,-0.721334926798555,
7.56690536680522));
#21348=CARTESIAN_POINT('Ctrl Pts',(-7.59527449071343,-0.53412843651438,
7.57938630005341));
#21349=CARTESIAN_POINT('Ctrl Pts',(-7.48480993131703,-0.270574496755715,
7.5918672333016));
#21350=CARTESIAN_POINT('Ctrl Pts',(-7.48353667075686,-0.00487092690823697,
7.60434816654979));
#21351=CARTESIAN_POINT('Ctrl Pts',(-7.48226341019669,0.260832642939241,
7.61682909979798));
#21352=CARTESIAN_POINT('Ctrl Pts',(-7.59019703546752,0.525433154240431,
7.62931003304617));
#21353=CARTESIAN_POINT('Ctrl Pts',(-7.77695120652518,0.714438148393268,
7.64179096629436));
#21354=CARTESIAN_POINT('Ctrl Pts',(-7.96370537758284,0.903443142546104,
7.65427189954255));
#21355=CARTESIAN_POINT('Ctrl Pts',(-8.22699388814826,1.01453885915658,7.66675283279074));
#21356=CARTESIAN_POINT('Ctrl Pts',(-8.49269364459156,1.01644874085988,7.67923376603893));
#21357=CARTESIAN_POINT('Ctrl Pts',(-8.75839340103485,1.01835862256319,7.69171469928712));
#21358=CARTESIAN_POINT('Ctrl Pts',(-9.02325176140384,0.911059288979006,
7.70419563253531));
#21359=CARTESIAN_POINT('Ctrl Pts',(-9.21270367535837,0.724758509267513,
7.7166765657835));
#21360=CARTESIAN_POINT('Ctrl Pts',(-9.40215558931291,0.538457729556019,
7.72915749903169));
#21361=CARTESIAN_POINT('Ctrl Pts',(-9.5138818253584,0.275436159672367,7.74163843227988));
#21362=CARTESIAN_POINT('Ctrl Pts',(-9.51642831724057,0.00974174196427458,
7.75411936552807));
#21363=CARTESIAN_POINT('Ctrl Pts',(-9.51645943884197,0.00649459406660589,
7.75427189954255));
#21364=CARTESIAN_POINT('Ctrl Pts',(-9.516475,0.00324729703361952,7.75442443355703));
#21365=CARTESIAN_POINT('Ctrl Pts',(-9.516475,1.76497372752086E-13,7.75457696757151));
#21366=CARTESIAN_POINT('Origin',(-8.5,0.,1.24542303242842));
#21367=CARTESIAN_POINT('',(-9.51687640138522,-8.48276715981014E-5,7.09542303242849));
#21368=CARTESIAN_POINT('',(-9.516475,1.61554465063385E-13,7.15457696757151));
#21369=CARTESIAN_POINT('',(-9.516475,1.78524650477582E-12,1.24542303242842));
#21370=CARTESIAN_POINT('Ctrl Pts',(-9.516475,1.34610651483819E-13,7.09542303242849));
#21371=CARTESIAN_POINT('Ctrl Pts',(-9.51647500000004,-0.265706620583844,
7.10790396567668));
#21372=CARTESIAN_POINT('Ctrl Pts',(-9.40727465387201,-0.529786878177039,
7.12038489892487));
#21373=CARTESIAN_POINT('Ctrl Pts',(-9.21961691907763,-0.717894780174797,
7.13286583217306));
#21374=CARTESIAN_POINT('Ctrl Pts',(-9.03195918428324,-0.906002682172555,
7.14534676542125));
#21375=CARTESIAN_POINT('Ctrl Pts',(-8.76814132834361,-1.01583545019914,
7.15782769866944));
#21376=CARTESIAN_POINT('Ctrl Pts',(-8.50243547044484,-1.0164720823066,7.17030863191764));
#21377=CARTESIAN_POINT('Ctrl Pts',(-8.23672961254608,-1.01710871441406,
7.18278956516583));
#21378=CARTESIAN_POINT('Ctrl Pts',(-7.97238846933315,-0.908541417082644,
7.19527049841402));
#21379=CARTESIAN_POINT('Ctrl Pts',(-7.78383148002323,-0.721334926798419,
7.20775143166221));
#21380=CARTESIAN_POINT('Ctrl Pts',(-7.59527449071331,-0.534128436514195,
7.2202323649104));
#21381=CARTESIAN_POINT('Ctrl Pts',(-7.48480993131696,-0.270574496755484,
7.23271329815859));
#21382=CARTESIAN_POINT('Ctrl Pts',(-7.48353667075686,-0.00487092690798588,
7.24519423140678));
#21383=CARTESIAN_POINT('Ctrl Pts',(-7.48226341019675,0.260832642939512,
7.25767516465497));
#21384=CARTESIAN_POINT('Ctrl Pts',(-7.59019703546766,0.525433154240694,
7.27015609790316));
#21385=CARTESIAN_POINT('Ctrl Pts',(-7.77695120652539,0.714438148393487,
7.28263703115135));
#21386=CARTESIAN_POINT('Ctrl Pts',(-7.96370537758312,0.903443142546281,
7.29511796439954));
#21387=CARTESIAN_POINT('Ctrl Pts',(-8.22699388814861,1.01453885915668,7.30759889764774));
#21388=CARTESIAN_POINT('Ctrl Pts',(-8.49269364459192,1.01644874085989,7.32007983089593));
#21389=CARTESIAN_POINT('Ctrl Pts',(-8.75839340103524,1.01835862256309,7.33256076414412));
#21390=CARTESIAN_POINT('Ctrl Pts',(-9.0232517614042,0.911059288978801,7.34504169739231));
#21391=CARTESIAN_POINT('Ctrl Pts',(-9.21270367535868,0.724758509267215,
7.3575226306405));
#21392=CARTESIAN_POINT('Ctrl Pts',(-9.40215558931315,0.538457729555629,
7.37000356388869));
#21393=CARTESIAN_POINT('Ctrl Pts',(-9.51388182535853,0.275436159671905,
7.38248449713688));
#21394=CARTESIAN_POINT('Ctrl Pts',(-9.51642831724058,0.00974174196379239,
7.39496543038507));
#21395=CARTESIAN_POINT('Ctrl Pts',(-9.51645943884197,0.00649459406627776,
7.39511796439954));
#21396=CARTESIAN_POINT('Ctrl Pts',(-9.516475,0.00324729703344547,7.39527049841402));
#21397=CARTESIAN_POINT('Ctrl Pts',(-9.516475,1.56527083874804E-13,7.39542303242849));
#21398=CARTESIAN_POINT('Ctrl Pts',(-9.516475,1.61554465063385E-13,7.15457696757151));
#21399=CARTESIAN_POINT('Ctrl Pts',(-9.51647500000004,-0.265706620583822,
7.1670579008197));
#21400=CARTESIAN_POINT('Ctrl Pts',(-9.40727465387202,-0.529786878177025,
7.17953883406789));
#21401=CARTESIAN_POINT('Ctrl Pts',(-9.21961691907764,-0.717894780174788,
7.19201976731609));
#21402=CARTESIAN_POINT('Ctrl Pts',(-9.03195918428325,-0.906002682172552,
7.20450070056428));
#21403=CARTESIAN_POINT('Ctrl Pts',(-8.76814132834361,-1.01583545019914,
7.21698163381247));
#21404=CARTESIAN_POINT('Ctrl Pts',(-8.50243547044484,-1.0164720823066,7.22946256706066));
#21405=CARTESIAN_POINT('Ctrl Pts',(-8.23672961254607,-1.01710871441406,
7.24194350030885));
#21406=CARTESIAN_POINT('Ctrl Pts',(-7.97238846933314,-0.908541417082639,
7.25442443355704));
#21407=CARTESIAN_POINT('Ctrl Pts',(-7.78383148002322,-0.721334926798408,
7.26690536680523));
#21408=CARTESIAN_POINT('Ctrl Pts',(-7.5952744907133,-0.534128436514177,
7.27938630005342));
#21409=CARTESIAN_POINT('Ctrl Pts',(-7.48480993131695,-0.270574496755458,
7.29186723330162));
#21410=CARTESIAN_POINT('Ctrl Pts',(-7.48353667075686,-0.00487092690795505,
7.30434816654981));
#21411=CARTESIAN_POINT('Ctrl Pts',(-7.48226341019676,0.260832642939548,
7.316829099798));
#21412=CARTESIAN_POINT('Ctrl Pts',(-7.59019703546768,0.525433154240731,
7.32931003304619));
#21413=CARTESIAN_POINT('Ctrl Pts',(-7.77695120652542,0.714438148393519,
7.34179096629438));
#21414=CARTESIAN_POINT('Ctrl Pts',(-7.96370537758317,0.903443142546308,
7.35427189954257));
#21415=CARTESIAN_POINT('Ctrl Pts',(-8.22699388814866,1.0145388591567,7.36675283279076));
#21416=CARTESIAN_POINT('Ctrl Pts',(-8.49269364459198,1.01644874085989,7.37923376603895));
#21417=CARTESIAN_POINT('Ctrl Pts',(-8.75839340103531,1.01835862256308,7.39171469928714));
#21418=CARTESIAN_POINT('Ctrl Pts',(-9.02325176140427,0.911059288978762,
7.40419563253534));
#21419=CARTESIAN_POINT('Ctrl Pts',(-9.21270367535874,0.724758509267153,
7.41667656578353));
#21420=CARTESIAN_POINT('Ctrl Pts',(-9.4021555893132,0.538457729555544,7.42915749903172));
#21421=CARTESIAN_POINT('Ctrl Pts',(-9.51388182535857,0.275436159671797,
7.44163843227991));
#21422=CARTESIAN_POINT('Ctrl Pts',(-9.51642831724058,0.0097417419636749,
7.4541193655281));
#21423=CARTESIAN_POINT('Ctrl Pts',(-9.51645943884197,0.00649459406619878,
7.45427189954257));
#21424=CARTESIAN_POINT('Ctrl Pts',(-9.516475,0.00324729703340501,7.45442443355704));
#21425=CARTESIAN_POINT('Ctrl Pts',(-9.516475,1.54580940361101E-13,7.45457696757151));
#21426=CARTESIAN_POINT('Origin',(-8.5,0.,1.24542303242842));
#21427=CARTESIAN_POINT('',(-9.51556541541323,-0.000810312451272878,6.79542303242848));
#21428=CARTESIAN_POINT('',(-9.516475,1.6852798976567E-13,6.85457696757151));
#21429=CARTESIAN_POINT('',(-9.516475,1.78524650477582E-12,1.24542303242842));
#21430=CARTESIAN_POINT('Ctrl Pts',(-9.51556541541323,-0.000810312451272902,
6.79542303242848));
#21431=CARTESIAN_POINT('Ctrl Pts',(-9.51634597973439,-0.110204889627698,
6.80055284253917));
#21432=CARTESIAN_POINT('Ctrl Pts',(-9.44942527604987,-0.557857220545352,
6.82158999380147));
#21433=CARTESIAN_POINT('Ctrl Pts',(-8.7968570426639,-1.16531969262148,6.85853448621541));
#21434=CARTESIAN_POINT('Ctrl Pts',(-7.67912294882438,-0.878910898486879,
6.90625650967025));
#21435=CARTESIAN_POINT('Ctrl Pts',(-7.37898454940943,0.0315485133979244,
6.94602486254932));
#21436=CARTESIAN_POINT('Ctrl Pts',(-7.67763196849479,0.663562963521021,
6.97783954485255));
#21437=CARTESIAN_POINT('Ctrl Pts',(-8.23225858352771,1.08902960614752,7.0096542271558));
#21438=CARTESIAN_POINT('Ctrl Pts',(-9.17182695227493,0.989535098804095,
7.04884872301444));
#21439=CARTESIAN_POINT('Ctrl Pts',(-9.51713519569878,0.324724529807011,
7.08008954829728));
#21440=CARTESIAN_POINT('Ctrl Pts',(-9.51817020583245,-0.000358245808598775,
7.09542303242849));
#21441=CARTESIAN_POINT('Ctrl Pts',(-9.516475,1.6852798976567E-13,6.85457696757151));
#21442=CARTESIAN_POINT('Ctrl Pts',(-9.51647500000004,-0.26570662058381,
6.8670579008197));
#21443=CARTESIAN_POINT('Ctrl Pts',(-9.40727465387203,-0.529786878177009,
6.87953883406789));
#21444=CARTESIAN_POINT('Ctrl Pts',(-9.21961691907765,-0.717894780174773,
6.89201976731608));
#21445=CARTESIAN_POINT('Ctrl Pts',(-9.03195918428327,-0.906002682172537,
6.90450070056428));
#21446=CARTESIAN_POINT('Ctrl Pts',(-8.76814132834364,-1.01583545019913,
6.91698163381247));
#21447=CARTESIAN_POINT('Ctrl Pts',(-8.50243547044488,-1.0164720823066,6.92946256706066));
#21448=CARTESIAN_POINT('Ctrl Pts',(-8.23672961254611,-1.01710871441407,
6.94194350030885));
#21449=CARTESIAN_POINT('Ctrl Pts',(-7.97238846933318,-0.908541417082661,
6.95442443355704));
#21450=CARTESIAN_POINT('Ctrl Pts',(-7.78383148002325,-0.721334926798443,
6.96690536680523));
#21451=CARTESIAN_POINT('Ctrl Pts',(-7.59527449071333,-0.534128436514225,
6.97938630005342));
#21452=CARTESIAN_POINT('Ctrl Pts',(-7.48480993131697,-0.270574496755518,
6.99186723330161));
#21453=CARTESIAN_POINT('Ctrl Pts',(-7.48353667075686,-0.0048709269080198,
7.0043481665498));
#21454=CARTESIAN_POINT('Ctrl Pts',(-7.48226341019674,0.260832642939478,
7.01682909979799));
#21455=CARTESIAN_POINT('Ctrl Pts',(-7.59019703546764,0.525433154240663,
7.02931003304619));
#21456=CARTESIAN_POINT('Ctrl Pts',(-7.77695120652537,0.714438148393463,
7.04179096629438));
#21457=CARTESIAN_POINT('Ctrl Pts',(-7.96370537758309,0.903443142546263,
7.05427189954257));
#21458=CARTESIAN_POINT('Ctrl Pts',(-8.22699388814857,1.01453885915667,7.06675283279076));
#21459=CARTESIAN_POINT('Ctrl Pts',(-8.49269364459189,1.01644874085989,7.07923376603895));
#21460=CARTESIAN_POINT('Ctrl Pts',(-8.7583934010352,1.0183586225631,7.09171469928714));
#21461=CARTESIAN_POINT('Ctrl Pts',(-9.02325176140417,0.911059288978819,
7.10419563253533));
#21462=CARTESIAN_POINT('Ctrl Pts',(-9.21270367535865,0.724758509267239,
7.11667656578352));
#21463=CARTESIAN_POINT('Ctrl Pts',(-9.40215558931313,0.538457729555659,
7.12915749903171));
#21464=CARTESIAN_POINT('Ctrl Pts',(-9.51388182535852,0.275436159671939,
7.1416384322799));
#21465=CARTESIAN_POINT('Ctrl Pts',(-9.51642831724058,0.00974174196382631,
7.15411936552809));
#21466=CARTESIAN_POINT('Ctrl Pts',(-9.51645943884197,0.00649459406630205,
7.15427189954257));
#21467=CARTESIAN_POINT('Ctrl Pts',(-9.516475,0.00324729703346011,7.15442443355704));
#21468=CARTESIAN_POINT('Ctrl Pts',(-9.516475,1.61554465063385E-13,7.15457696757151));
#21469=CARTESIAN_POINT('Origin',(-8.5,0.,1.24542303242842));
#21470=CARTESIAN_POINT('',(-9.51625672877642,9.02772980376447E-5,6.49542303242849));
#21471=CARTESIAN_POINT('',(-9.516475,1.75501514467955E-13,6.55457696757151));
#21472=CARTESIAN_POINT('',(-9.516475,1.78524650477582E-12,1.24542303242842));
#21473=CARTESIAN_POINT('Ctrl Pts',(-9.51510181470517,0.000567951450037713,
6.49542303242849));
#21474=CARTESIAN_POINT('Ctrl Pts',(-9.51414510430117,-0.206228520727224,
6.50510879562945));
#21475=CARTESIAN_POINT('Ctrl Pts',(-9.35231132463273,-0.754153240087441,
6.53070189998202));
#21476=CARTESIAN_POINT('Ctrl Pts',(-8.45426188445871,-1.20176184221855,
6.57220234548622));
#21477=CARTESIAN_POINT('Ctrl Pts',(-7.63158681559905,-0.709598118880692,
6.61197069836528));
#21478=CARTESIAN_POINT('Ctrl Pts',(-7.44392618126472,-0.0362363792399661,
6.64378538066852));
#21479=CARTESIAN_POINT('Ctrl Pts',(-7.58499054185306,0.648404688957481,
6.67560006297176));
#21480=CARTESIAN_POINT('Ctrl Pts',(-8.37199588104198,1.19580033707788,6.71536841585081));
#21481=CARTESIAN_POINT('Ctrl Pts',(-9.32299097508662,0.800672039024471,
6.75796062919499));
#21482=CARTESIAN_POINT('Ctrl Pts',(-9.5139254802072,0.229023429108448,6.78464550138755));
#21483=CARTESIAN_POINT('Ctrl Pts',(-9.51556541541323,-0.000810312451272902,
6.79542303242848));
#21484=CARTESIAN_POINT('Ctrl Pts',(-9.516475,1.75501514467955E-13,6.55457696757151));
#21485=CARTESIAN_POINT('Ctrl Pts',(-9.51647500000005,-0.265706620583793,
6.5670579008197));
#21486=CARTESIAN_POINT('Ctrl Pts',(-9.40727465387204,-0.529786878176984,
6.57953883406789));
#21487=CARTESIAN_POINT('Ctrl Pts',(-9.21961691907768,-0.717894780174748,
6.59201976731608));
#21488=CARTESIAN_POINT('Ctrl Pts',(-9.03195918428331,-0.906002682172512,
6.60450070056427));
#21489=CARTESIAN_POINT('Ctrl Pts',(-8.7681413283437,-1.01583545019911,6.61698163381246));
#21490=CARTESIAN_POINT('Ctrl Pts',(-8.50243547044494,-1.0164720823066,6.62946256706065));
#21491=CARTESIAN_POINT('Ctrl Pts',(-8.23672961254619,-1.01710871441409,
6.64194350030885));
#21492=CARTESIAN_POINT('Ctrl Pts',(-7.97238846933326,-0.908541417082703,
6.65442443355704));
#21493=CARTESIAN_POINT('Ctrl Pts',(-7.78383148002332,-0.721334926798509,
6.66690536680523));
#21494=CARTESIAN_POINT('Ctrl Pts',(-7.59527449071338,-0.534128436514315,
6.67938630005342));
#21495=CARTESIAN_POINT('Ctrl Pts',(-7.484809931317,-0.270574496755631,6.69186723330161));
#21496=CARTESIAN_POINT('Ctrl Pts',(-7.48353667075686,-0.00487092690814233,
6.7043481665498));
#21497=CARTESIAN_POINT('Ctrl Pts',(-7.48226341019671,0.260832642939346,
6.71682909979799));
#21498=CARTESIAN_POINT('Ctrl Pts',(-7.59019703546757,0.525433154240535,
6.72931003304618));
#21499=CARTESIAN_POINT('Ctrl Pts',(-7.77695120652526,0.714438148393355,
6.74179096629437));
#21500=CARTESIAN_POINT('Ctrl Pts',(-7.96370537758295,0.903443142546176,
6.75427189954256));
#21501=CARTESIAN_POINT('Ctrl Pts',(-8.2269938881484,1.01453885915662,6.76675283279075));
#21502=CARTESIAN_POINT('Ctrl Pts',(-8.49269364459171,1.01644874085989,6.77923376603894));
#21503=CARTESIAN_POINT('Ctrl Pts',(-8.75839340103502,1.01835862256315,6.79171469928713));
#21504=CARTESIAN_POINT('Ctrl Pts',(-9.02325176140399,0.91105928897892,6.80419563253532));
#21505=CARTESIAN_POINT('Ctrl Pts',(-9.2127036753585,0.724758509267386,6.81667656578351));
#21506=CARTESIAN_POINT('Ctrl Pts',(-9.40215558931301,0.538457729555852,
6.8291574990317));
#21507=CARTESIAN_POINT('Ctrl Pts',(-9.51388182535846,0.275436159672167,
6.84163843227989));
#21508=CARTESIAN_POINT('Ctrl Pts',(-9.51642831724057,0.00974174196406439,
6.85411936552808));
#21509=CARTESIAN_POINT('Ctrl Pts',(-9.51645943884197,0.0064945940664631,
6.85427189954256));
#21510=CARTESIAN_POINT('Ctrl Pts',(-9.516475,0.00324729703354412,6.85442443355704));
#21511=CARTESIAN_POINT('Ctrl Pts',(-9.516475,1.6852798976567E-13,6.85457696757151));
#21512=CARTESIAN_POINT('Origin',(-8.5,0.,1.24542303242842));
#21513=CARTESIAN_POINT('',(-9.516475,1.55531225590673E-13,6.19542303242849));
#21514=CARTESIAN_POINT('',(-9.516475,1.8247503917024E-13,6.25457696757151));
#21515=CARTESIAN_POINT('',(-9.516475,1.78524650477582E-12,1.24542303242842));
#21516=CARTESIAN_POINT('Ctrl Pts',(-9.516475,1.55531225590673E-13,6.19542303242849));
#21517=CARTESIAN_POINT('Ctrl Pts',(-9.51647500000004,-0.265706620583813,
6.20790396567668));
#21518=CARTESIAN_POINT('Ctrl Pts',(-9.40727465387203,-0.529786878177001,
6.22038489892487));
#21519=CARTESIAN_POINT('Ctrl Pts',(-9.21961691907766,-0.717894780174762,
6.23286583217306));
#21520=CARTESIAN_POINT('Ctrl Pts',(-9.03195918428329,-0.906002682172522,
6.24534676542125));
#21521=CARTESIAN_POINT('Ctrl Pts',(-8.76814132834368,-1.01583545019912,
6.25782769866944));
#21522=CARTESIAN_POINT('Ctrl Pts',(-8.50243547044492,-1.0164720823066,6.27030863191763));
#21523=CARTESIAN_POINT('Ctrl Pts',(-8.23672961254617,-1.01710871441408,
6.28278956516582));
#21524=CARTESIAN_POINT('Ctrl Pts',(-7.97238846933324,-0.908541417082693,
6.29527049841401));
#21525=CARTESIAN_POINT('Ctrl Pts',(-7.78383148002331,-0.721334926798495,
6.3077514316622));
#21526=CARTESIAN_POINT('Ctrl Pts',(-7.59527449071337,-0.534128436514297,
6.32023236491039));
#21527=CARTESIAN_POINT('Ctrl Pts',(-7.484809931317,-0.270574496755611,6.33271329815858));
#21528=CARTESIAN_POINT('Ctrl Pts',(-7.48353667075686,-0.00487092690812236,
6.34519423140677));
#21529=CARTESIAN_POINT('Ctrl Pts',(-7.48226341019672,0.260832642939366,
6.35767516465496));
#21530=CARTESIAN_POINT('Ctrl Pts',(-7.59019703546758,0.525433154240553,
6.37015609790315));
#21531=CARTESIAN_POINT('Ctrl Pts',(-7.77695120652528,0.71443814839337,6.38263703115135));
#21532=CARTESIAN_POINT('Ctrl Pts',(-7.96370537758297,0.903443142546187,
6.39511796439954));
#21533=CARTESIAN_POINT('Ctrl Pts',(-8.22699388814842,1.01453885915663,6.40759889764773));
#21534=CARTESIAN_POINT('Ctrl Pts',(-8.49269364459173,1.01644874085989,6.42007983089592));
#21535=CARTESIAN_POINT('Ctrl Pts',(-8.75839340103504,1.01835862256314,6.43256076414411));
#21536=CARTESIAN_POINT('Ctrl Pts',(-9.02325176140401,0.911059288978909,
6.4450416973923));
#21537=CARTESIAN_POINT('Ctrl Pts',(-9.21270367535852,0.724758509267372,
6.45752263064049));
#21538=CARTESIAN_POINT('Ctrl Pts',(-9.40215558931302,0.538457729555834,
6.47000356388868));
#21539=CARTESIAN_POINT('Ctrl Pts',(-9.51388182535847,0.275436159672147,
6.48248449713687));
#21540=CARTESIAN_POINT('Ctrl Pts',(-9.51642831724057,0.00974174196404442,
6.49496543038506));
#21541=CARTESIAN_POINT('Ctrl Pts',(-9.51645943884197,0.00649459406644795,
6.49511796439954));
#21542=CARTESIAN_POINT('Ctrl Pts',(-9.516475,0.00324729703353379,6.49527049841401));
#21543=CARTESIAN_POINT('Ctrl Pts',(-9.516475,1.63002679435024E-13,6.49542303242849));
#21544=CARTESIAN_POINT('Ctrl Pts',(-9.516475,1.8247503917024E-13,6.25457696757151));
#21545=CARTESIAN_POINT('Ctrl Pts',(-9.51647500000005,-0.265706620583796,
6.2670579008197));
#21546=CARTESIAN_POINT('Ctrl Pts',(-9.40727465387204,-0.529786878176997,
6.27953883406789));
#21547=CARTESIAN_POINT('Ctrl Pts',(-9.21961691907766,-0.717894780174763,
6.29201976731608));
#21548=CARTESIAN_POINT('Ctrl Pts',(-9.03195918428329,-0.90600268217253,
6.30450070056427));
#21549=CARTESIAN_POINT('Ctrl Pts',(-8.76814132834365,-1.01583545019912,
6.31698163381247));
#21550=CARTESIAN_POINT('Ctrl Pts',(-8.50243547044489,-1.0164720823066,6.32946256706066));
#21551=CARTESIAN_POINT('Ctrl Pts',(-8.23672961254613,-1.01710871441407,
6.34194350030885));
#21552=CARTESIAN_POINT('Ctrl Pts',(-7.97238846933319,-0.908541417082669,
6.35442443355704));
#21553=CARTESIAN_POINT('Ctrl Pts',(-7.78383148002326,-0.721334926798453,
6.36690536680523));
#21554=CARTESIAN_POINT('Ctrl Pts',(-7.59527449071334,-0.534128436514237,
6.37938630005342));
#21555=CARTESIAN_POINT('Ctrl Pts',(-7.48480993131697,-0.270574496755532,
6.39186723330161));
#21556=CARTESIAN_POINT('Ctrl Pts',(-7.48353667075686,-0.00487092690803375,
6.4043481665498));
#21557=CARTESIAN_POINT('Ctrl Pts',(-7.48226341019674,0.260832642939464,
6.41682909979799));
#21558=CARTESIAN_POINT('Ctrl Pts',(-7.59019703546764,0.525433154240651,
6.42931003304618));
#21559=CARTESIAN_POINT('Ctrl Pts',(-7.77695120652536,0.714438148393453,
6.44179096629438));
#21560=CARTESIAN_POINT('Ctrl Pts',(-7.96370537758308,0.903443142546255,
6.45427189954257));
#21561=CARTESIAN_POINT('Ctrl Pts',(-8.22699388814856,1.01453885915667,6.46675283279076));
#21562=CARTESIAN_POINT('Ctrl Pts',(-8.49269364459187,1.01644874085989,6.47923376603895));
#21563=CARTESIAN_POINT('Ctrl Pts',(-8.75839340103519,1.0183586225631,6.49171469928714));
#21564=CARTESIAN_POINT('Ctrl Pts',(-9.02325176140416,0.911059288978826,
6.50419563253533));
#21565=CARTESIAN_POINT('Ctrl Pts',(-9.21270367535864,0.724758509267249,
6.51667656578352));
#21566=CARTESIAN_POINT('Ctrl Pts',(-9.40215558931312,0.538457729555672,
6.52915749903171));
#21567=CARTESIAN_POINT('Ctrl Pts',(-9.51388182535852,0.275436159671953,
6.5416384322799));
#21568=CARTESIAN_POINT('Ctrl Pts',(-9.51642831724058,0.00974174196384026,
6.55411936552809));
#21569=CARTESIAN_POINT('Ctrl Pts',(-9.51645943884197,0.006494594066316,
6.55427189954257));
#21570=CARTESIAN_POINT('Ctrl Pts',(-9.516475,0.00324729703347406,6.55442443355704));
#21571=CARTESIAN_POINT('Ctrl Pts',(-9.516475,1.75501514467955E-13,6.55457696757151));
#21572=CARTESIAN_POINT('Origin',(-8.5,0.,1.24542303242842));
#21573=CARTESIAN_POINT('',(-9.516475,1.62504750292958E-13,5.89542303242849));
#21574=CARTESIAN_POINT('',(-9.516475,1.89448563872525E-13,5.95457696757151));
#21575=CARTESIAN_POINT('',(-9.516475,1.78524650477582E-12,1.24542303242842));
#21576=CARTESIAN_POINT('Ctrl Pts',(-9.516475,1.62504750292958E-13,5.89542303242849));
#21577=CARTESIAN_POINT('Ctrl Pts',(-9.51647500000004,-0.265706620583806,
5.90790396567668));
#21578=CARTESIAN_POINT('Ctrl Pts',(-9.40727465387204,-0.529786878176995,
5.92038489892487));
#21579=CARTESIAN_POINT('Ctrl Pts',(-9.21961691907767,-0.717894780174757,
5.93286583217306));
#21580=CARTESIAN_POINT('Ctrl Pts',(-9.0319591842833,-0.906002682172519,
5.94534676542125));
#21581=CARTESIAN_POINT('Ctrl Pts',(-8.76814132834368,-1.01583545019911,
5.95782769866944));
#21582=CARTESIAN_POINT('Ctrl Pts',(-8.50243547044493,-1.0164720823066,5.97030863191763));
#21583=CARTESIAN_POINT('Ctrl Pts',(-8.23672961254618,-1.01710871441408,
5.98278956516582));
#21584=CARTESIAN_POINT('Ctrl Pts',(-7.97238846933324,-0.908541417082697,
5.99527049841401));
#21585=CARTESIAN_POINT('Ctrl Pts',(-7.78383148002331,-0.7213349267985,6.0077514316622));
#21586=CARTESIAN_POINT('Ctrl Pts',(-7.59527449071338,-0.534128436514303,
6.02023236491039));
#21587=CARTESIAN_POINT('Ctrl Pts',(-7.484809931317,-0.270574496755618,6.03271329815858));
#21588=CARTESIAN_POINT('Ctrl Pts',(-7.48353667075686,-0.00487092690812934,
6.04519423140677));
#21589=CARTESIAN_POINT('Ctrl Pts',(-7.48226341019671,0.260832642939359,
6.05767516465496));
#21590=CARTESIAN_POINT('Ctrl Pts',(-7.59019703546758,0.525433154240546,
6.07015609790315));
#21591=CARTESIAN_POINT('Ctrl Pts',(-7.77695120652527,0.714438148393365,
6.08263703115134));
#21592=CARTESIAN_POINT('Ctrl Pts',(-7.96370537758296,0.903443142546183,
6.09511796439954));
#21593=CARTESIAN_POINT('Ctrl Pts',(-8.22699388814841,1.01453885915663,6.10759889764773));
#21594=CARTESIAN_POINT('Ctrl Pts',(-8.49269364459172,1.01644874085989,6.12007983089592));
#21595=CARTESIAN_POINT('Ctrl Pts',(-8.75839340103503,1.01835862256314,6.13256076414411));
#21596=CARTESIAN_POINT('Ctrl Pts',(-9.023251761404,0.911059288978913,6.1450416973923));
#21597=CARTESIAN_POINT('Ctrl Pts',(-9.21270367535851,0.724758509267377,
6.15752263064049));
#21598=CARTESIAN_POINT('Ctrl Pts',(-9.40215558931302,0.53845772955584,6.17000356388868));
#21599=CARTESIAN_POINT('Ctrl Pts',(-9.51388182535846,0.275436159672154,
6.18248449713687));
#21600=CARTESIAN_POINT('Ctrl Pts',(-9.51642831724057,0.0097417419640514,
6.19496543038506));
#21601=CARTESIAN_POINT('Ctrl Pts',(-9.51645943884197,0.00649459406645011,
6.19511796439954));
#21602=CARTESIAN_POINT('Ctrl Pts',(-9.516475,0.00324729703353112,6.19527049841401));
#21603=CARTESIAN_POINT('Ctrl Pts',(-9.516475,1.55531225590673E-13,6.19542303242849));
#21604=CARTESIAN_POINT('Ctrl Pts',(-9.516475,2.0389354241916E-13,5.95457696757151));
#21605=CARTESIAN_POINT('Ctrl Pts',(-9.51647500000005,-0.265706620583774,
5.9670579008197));
#21606=CARTESIAN_POINT('Ctrl Pts',(-9.40727465387205,-0.529786878176977,
5.97953883406789));
#21607=CARTESIAN_POINT('Ctrl Pts',(-9.21961691907768,-0.717894780174748,
5.99201976731608));
#21608=CARTESIAN_POINT('Ctrl Pts',(-9.03195918428331,-0.906002682172519,
6.00450070056427));
#21609=CARTESIAN_POINT('Ctrl Pts',(-8.76814132834368,-1.01583545019912,
6.01698163381247));
#21610=CARTESIAN_POINT('Ctrl Pts',(-8.50243547044491,-1.0164720823066,6.02946256706066));
#21611=CARTESIAN_POINT('Ctrl Pts',(-8.23672961254615,-1.01710871441408,
6.04194350030885));
#21612=CARTESIAN_POINT('Ctrl Pts',(-7.97238846933321,-0.90854141708268,
6.05442443355704));
#21613=CARTESIAN_POINT('Ctrl Pts',(-7.78383148002328,-0.721334926798468,
6.06690536680523));
#21614=CARTESIAN_POINT('Ctrl Pts',(-7.59527449071335,-0.534128436514256,
6.07938630005342));
#21615=CARTESIAN_POINT('Ctrl Pts',(-7.48480993131698,-0.270574496755553,
6.09186723330161));
#21616=CARTESIAN_POINT('Ctrl Pts',(-7.48353667075686,-0.00487092690805517,
6.1043481665498));
#21617=CARTESIAN_POINT('Ctrl Pts',(-7.48226341019673,0.260832642939443,
6.11682909979799));
#21618=CARTESIAN_POINT('Ctrl Pts',(-7.59019703546762,0.525433154240632,
6.12931003304618));
#21619=CARTESIAN_POINT('Ctrl Pts',(-7.77695120652534,0.714438148393438,
6.14179096629437));
#21620=CARTESIAN_POINT('Ctrl Pts',(-7.96370537758306,0.903443142546244,
6.15427189954256));
#21621=CARTESIAN_POINT('Ctrl Pts',(-8.22699388814854,1.01453885915666,6.16675283279076));
#21622=CARTESIAN_POINT('Ctrl Pts',(-8.49269364459185,1.01644874085989,6.17923376603895));
#21623=CARTESIAN_POINT('Ctrl Pts',(-8.75839340103517,1.01835862256311,6.19171469928714));
#21624=CARTESIAN_POINT('Ctrl Pts',(-9.02325176140414,0.911059288978837,
6.20419563253533));
#21625=CARTESIAN_POINT('Ctrl Pts',(-9.21270367535863,0.724758509267264,
6.21667656578352));
#21626=CARTESIAN_POINT('Ctrl Pts',(-9.40215558931311,0.53845772955569,6.22915749903171));
#21627=CARTESIAN_POINT('Ctrl Pts',(-9.51388182535852,0.275436159671974,
6.2416384322799));
#21628=CARTESIAN_POINT('Ctrl Pts',(-9.51642831724058,0.00974174196386167,
6.25411936552809));
#21629=CARTESIAN_POINT('Ctrl Pts',(-9.51645943884197,0.0064945940663326,
6.25427189954257));
#21630=CARTESIAN_POINT('Ctrl Pts',(-9.516475,0.00324729703348583,6.25442443355704));
#21631=CARTESIAN_POINT('Ctrl Pts',(-9.516475,1.8247503917024E-13,6.25457696757151));
#21632=CARTESIAN_POINT('Origin',(-8.5,0.,1.24542303242842));
#21633=CARTESIAN_POINT('',(-9.516475,1.69478274995243E-13,5.59542303242849));
#21634=CARTESIAN_POINT('',(-9.516475,1.9642208857481E-13,5.65457696757151));
#21635=CARTESIAN_POINT('',(-9.516475,1.78524650477582E-12,1.24542303242842));
#21636=CARTESIAN_POINT('Ctrl Pts',(-9.516475,1.83923253541878E-13,5.59542303242849));
#21637=CARTESIAN_POINT('Ctrl Pts',(-9.51647500000005,-0.26570662058379,
5.60790396567668));
#21638=CARTESIAN_POINT('Ctrl Pts',(-9.40727465387205,-0.529786878176986,
5.62038489892487));
#21639=CARTESIAN_POINT('Ctrl Pts',(-9.21961691907767,-0.717894780174752,
5.63286583217306));
#21640=CARTESIAN_POINT('Ctrl Pts',(-9.0319591842833,-0.906002682172518,
5.64534676542125));
#21641=CARTESIAN_POINT('Ctrl Pts',(-8.76814132834368,-1.01583545019912,
5.65782769866944));
#21642=CARTESIAN_POINT('Ctrl Pts',(-8.50243547044492,-1.0164720823066,5.67030863191763));
#21643=CARTESIAN_POINT('Ctrl Pts',(-8.23672961254616,-1.01710871441408,
5.68278956516582));
#21644=CARTESIAN_POINT('Ctrl Pts',(-7.97238846933323,-0.908541417082689,
5.69527049841401));
#21645=CARTESIAN_POINT('Ctrl Pts',(-7.7838314800233,-0.721334926798484,
5.7077514316622));
#21646=CARTESIAN_POINT('Ctrl Pts',(-7.59527449071336,-0.53412843651428,
5.72023236491039));
#21647=CARTESIAN_POINT('Ctrl Pts',(-7.48480993131699,-0.270574496755586,
5.73271329815858));
#21648=CARTESIAN_POINT('Ctrl Pts',(-7.48353667075686,-0.00487092690809298,
5.74519423140678));
#21649=CARTESIAN_POINT('Ctrl Pts',(-7.48226341019672,0.2608326429394,5.75767516465497));
#21650=CARTESIAN_POINT('Ctrl Pts',(-7.5901970354676,0.525433154240588,5.77015609790316));
#21651=CARTESIAN_POINT('Ctrl Pts',(-7.77695120652531,0.714438148393401,
5.78263703115135));
#21652=CARTESIAN_POINT('Ctrl Pts',(-7.96370537758301,0.903443142546213,
5.79511796439954));
#21653=CARTESIAN_POINT('Ctrl Pts',(-8.22699388814848,1.01453885915665,5.80759889764773));
#21654=CARTESIAN_POINT('Ctrl Pts',(-8.49269364459179,1.01644874085989,5.82007983089592));
#21655=CARTESIAN_POINT('Ctrl Pts',(-8.7583934010351,1.01835862256313,5.83256076414411));
#21656=CARTESIAN_POINT('Ctrl Pts',(-9.02325176140407,0.911059288978875,
5.8450416973923));
#21657=CARTESIAN_POINT('Ctrl Pts',(-9.21270367535857,0.724758509267321,
5.85752263064049));
#21658=CARTESIAN_POINT('Ctrl Pts',(-9.40215558931307,0.538457729555766,
5.87000356388868));
#21659=CARTESIAN_POINT('Ctrl Pts',(-9.51388182535849,0.275436159672064,
5.88248449713687));
#21660=CARTESIAN_POINT('Ctrl Pts',(-9.51642831724057,0.00974174196395726,
5.89496543038506));
#21661=CARTESIAN_POINT('Ctrl Pts',(-9.51645943884197,0.00649459406638967,
5.89511796439954));
#21662=CARTESIAN_POINT('Ctrl Pts',(-9.516475,0.00324729703350438,5.89527049841401));
#21663=CARTESIAN_POINT('Ctrl Pts',(-9.516475,1.62504750292958E-13,5.89542303242849));
#21664=CARTESIAN_POINT('Ctrl Pts',(-9.516475,1.9642208857481E-13,5.65457696757151));
#21665=CARTESIAN_POINT('Ctrl Pts',(-9.51647500000005,-0.265706620583782,
5.6670579008197));
#21666=CARTESIAN_POINT('Ctrl Pts',(-9.40727465387205,-0.529786878176984,
5.67953883406789));
#21667=CARTESIAN_POINT('Ctrl Pts',(-9.21961691907767,-0.717894780174753,
5.69201976731608));
#21668=CARTESIAN_POINT('Ctrl Pts',(-9.0319591842833,-0.906002682172523,
5.70450070056427));
#21669=CARTESIAN_POINT('Ctrl Pts',(-8.76814132834367,-1.01583545019912,
5.71698163381247));
#21670=CARTESIAN_POINT('Ctrl Pts',(-8.5024354704449,-1.0164720823066,5.72946256706066));
#21671=CARTESIAN_POINT('Ctrl Pts',(-8.23672961254614,-1.01710871441408,
5.74194350030885));
#21672=CARTESIAN_POINT('Ctrl Pts',(-7.9723884693332,-0.908541417082676,
5.75442443355704));
#21673=CARTESIAN_POINT('Ctrl Pts',(-7.78383148002327,-0.721334926798463,
5.76690536680523));
#21674=CARTESIAN_POINT('Ctrl Pts',(-7.59527449071334,-0.53412843651425,
5.77938630005342));
#21675=CARTESIAN_POINT('Ctrl Pts',(-7.48480993131698,-0.270574496755546,
5.79186723330161));
#21676=CARTESIAN_POINT('Ctrl Pts',(-7.48353667075686,-0.0048709269080477,
5.8043481665498));
#21677=CARTESIAN_POINT('Ctrl Pts',(-7.48226341019673,0.26083264293945,5.81682909979799));
#21678=CARTESIAN_POINT('Ctrl Pts',(-7.59019703546763,0.525433154240638,
5.82931003304618));
#21679=CARTESIAN_POINT('Ctrl Pts',(-7.77695120652535,0.714438148393443,
5.84179096629437));
#21680=CARTESIAN_POINT('Ctrl Pts',(-7.96370537758307,0.903443142546248,
5.85427189954256));
#21681=CARTESIAN_POINT('Ctrl Pts',(-8.22699388814855,1.01453885915667,5.86675283279076));
#21682=CARTESIAN_POINT('Ctrl Pts',(-8.49269364459186,1.01644874085989,5.87923376603895));
#21683=CARTESIAN_POINT('Ctrl Pts',(-8.75839340103518,1.01835862256311,5.89171469928714));
#21684=CARTESIAN_POINT('Ctrl Pts',(-9.02325176140415,0.911059288978833,
5.90419563253533));
#21685=CARTESIAN_POINT('Ctrl Pts',(-9.21270367535863,0.724758509267258,
5.91667656578352));
#21686=CARTESIAN_POINT('Ctrl Pts',(-9.40215558931312,0.538457729555684,
5.92915749903171));
#21687=CARTESIAN_POINT('Ctrl Pts',(-9.51388182535852,0.275436159671966,
5.9416384322799));
#21688=CARTESIAN_POINT('Ctrl Pts',(-9.51642831724058,0.0097417419638542,
5.95411936552809));
#21689=CARTESIAN_POINT('Ctrl Pts',(-9.51645943884197,0.00649459406633476,
5.95427189954257));
#21690=CARTESIAN_POINT('Ctrl Pts',(-9.516475,0.00324729703349764,5.95442443355704));
#21691=CARTESIAN_POINT('Ctrl Pts',(-9.516475,2.0389354241916E-13,5.95457696757151));
#21692=CARTESIAN_POINT('Origin',(-8.5,0.,1.24542303242842));
#21693=CARTESIAN_POINT('',(-9.516475,1.76451799697528E-13,5.29542303242849));
#21694=CARTESIAN_POINT('',(-9.51597631883388,-0.000112310372824663,5.35457696757151));
#21695=CARTESIAN_POINT('',(-9.516475,1.78524650477582E-12,1.24542303242842));
#21696=CARTESIAN_POINT('Ctrl Pts',(-9.516475,1.76451799697528E-13,5.29542303242849));
#21697=CARTESIAN_POINT('Ctrl Pts',(-9.51647500000005,-0.265706620583792,
5.30790396567668));
#21698=CARTESIAN_POINT('Ctrl Pts',(-9.40727465387205,-0.529786878176983,
5.32038489892487));
#21699=CARTESIAN_POINT('Ctrl Pts',(-9.21961691907768,-0.717894780174747,
5.33286583217306));
#21700=CARTESIAN_POINT('Ctrl Pts',(-9.03195918428331,-0.906002682172511,
5.34534676542125));
#21701=CARTESIAN_POINT('Ctrl Pts',(-8.7681413283437,-1.01583545019911,5.35782769866944));
#21702=CARTESIAN_POINT('Ctrl Pts',(-8.50243547044494,-1.0164720823066,5.37030863191763));
#21703=CARTESIAN_POINT('Ctrl Pts',(-8.23672961254619,-1.01710871441409,
5.38278956516582));
#21704=CARTESIAN_POINT('Ctrl Pts',(-7.97238846933326,-0.908541417082704,
5.39527049841401));
#21705=CARTESIAN_POINT('Ctrl Pts',(-7.78383148002332,-0.72133492679851,
5.4077514316622));
#21706=CARTESIAN_POINT('Ctrl Pts',(-7.59527449071338,-0.534128436514316,
5.42023236491039));
#21707=CARTESIAN_POINT('Ctrl Pts',(-7.484809931317,-0.270574496755632,5.43271329815858));
#21708=CARTESIAN_POINT('Ctrl Pts',(-7.48353667075686,-0.00487092690814328,
5.44519423140677));
#21709=CARTESIAN_POINT('Ctrl Pts',(-7.48226341019671,0.260832642939345,
5.45767516465496));
#21710=CARTESIAN_POINT('Ctrl Pts',(-7.59019703546757,0.525433154240534,
5.47015609790315));
#21711=CARTESIAN_POINT('Ctrl Pts',(-7.77695120652526,0.714438148393355,
5.48263703115134));
#21712=CARTESIAN_POINT('Ctrl Pts',(-7.96370537758295,0.903443142546176,
5.49511796439953));
#21713=CARTESIAN_POINT('Ctrl Pts',(-8.2269938881484,1.01453885915662,5.50759889764772));
#21714=CARTESIAN_POINT('Ctrl Pts',(-8.49269364459171,1.01644874085989,5.52007983089592));
#21715=CARTESIAN_POINT('Ctrl Pts',(-8.75839340103501,1.01835862256315,5.53256076414411));
#21716=CARTESIAN_POINT('Ctrl Pts',(-9.02325176140399,0.91105928897892,5.5450416973923));
#21717=CARTESIAN_POINT('Ctrl Pts',(-9.2127036753585,0.724758509267386,5.55752263064049));
#21718=CARTESIAN_POINT('Ctrl Pts',(-9.40215558931301,0.538457729555853,
5.57000356388868));
#21719=CARTESIAN_POINT('Ctrl Pts',(-9.51388182535846,0.275436159672167,
5.58248449713687));
#21720=CARTESIAN_POINT('Ctrl Pts',(-9.51642831724057,0.00974174196406534,
5.59496543038506));
#21721=CARTESIAN_POINT('Ctrl Pts',(-9.51645943884197,0.00649459406646887,
5.59511796439953));
#21722=CARTESIAN_POINT('Ctrl Pts',(-9.516475,0.00324729703355471,5.59527049841401));
#21723=CARTESIAN_POINT('Ctrl Pts',(-9.516475,1.83923253541878E-13,5.59542303242849));
#21724=CARTESIAN_POINT('Ctrl Pts',(-9.516475,2.17840591823729E-13,5.35457696757151));
#21725=CARTESIAN_POINT('Ctrl Pts',(-9.51647500000006,-0.265706620583756,
5.3670579008197));
#21726=CARTESIAN_POINT('Ctrl Pts',(-9.40727465387206,-0.529786878176955,
5.37953883406789));
#21727=CARTESIAN_POINT('Ctrl Pts',(-9.2196169190777,-0.717894780174728,
5.39201976731608));
#21728=CARTESIAN_POINT('Ctrl Pts',(-9.03195918428333,-0.906002682172501,
5.40450070056427));
#21729=CARTESIAN_POINT('Ctrl Pts',(-8.76814132834371,-1.01583545019911,
5.41698163381246));
#21730=CARTESIAN_POINT('Ctrl Pts',(-8.50243547044496,-1.0164720823066,5.42946256706065));
#21731=CARTESIAN_POINT('Ctrl Pts',(-8.2367296125462,-1.01710871441409,5.44194350030884));
#21732=CARTESIAN_POINT('Ctrl Pts',(-7.97238846933326,-0.908541417082706,
5.45442443355703));
#21733=CARTESIAN_POINT('Ctrl Pts',(-7.78383148002332,-0.721334926798508,
5.46690536680522));
#21734=CARTESIAN_POINT('Ctrl Pts',(-7.59527449071338,-0.534128436514311,
5.47938630005342));
#21735=CARTESIAN_POINT('Ctrl Pts',(-7.484809931317,-0.27057449675562,5.49186723330161));
#21736=CARTESIAN_POINT('Ctrl Pts',(-7.48353667075686,-0.00487092690812689,
5.5043481665498));
#21737=CARTESIAN_POINT('Ctrl Pts',(-7.48226341019671,0.260832642939366,
5.51682909979799));
#21738=CARTESIAN_POINT('Ctrl Pts',(-7.59019703546758,0.525433154240558,
5.52931003304618));
#21739=CARTESIAN_POINT('Ctrl Pts',(-7.77695120652528,0.714438148393377,
5.54179096629437));
#21740=CARTESIAN_POINT('Ctrl Pts',(-7.96370537758298,0.903443142546195,
5.55427189954256));
#21741=CARTESIAN_POINT('Ctrl Pts',(-8.22699388814844,1.01453885915664,5.56675283279075));
#21742=CARTESIAN_POINT('Ctrl Pts',(-8.49269364459175,1.01644874085989,5.57923376603894));
#21743=CARTESIAN_POINT('Ctrl Pts',(-8.75839340103506,1.01835862256314,5.59171469928713));
#21744=CARTESIAN_POINT('Ctrl Pts',(-9.02325176140404,0.911059288978893,
5.60419563253532));
#21745=CARTESIAN_POINT('Ctrl Pts',(-9.21270367535854,0.724758509267344,
5.61667656578351));
#21746=CARTESIAN_POINT('Ctrl Pts',(-9.40215558931305,0.538457729555796,
5.62915749903171));
#21747=CARTESIAN_POINT('Ctrl Pts',(-9.51388182535848,0.275436159672098,
5.64163843227989));
#21748=CARTESIAN_POINT('Ctrl Pts',(-9.51642831724057,0.00974174196399118,
5.65411936552809));
#21749=CARTESIAN_POINT('Ctrl Pts',(-9.51645943884197,0.00649459406642359,
5.65427189954256));
#21750=CARTESIAN_POINT('Ctrl Pts',(-9.516475,0.0032472970335383,5.65442443355704));
#21751=CARTESIAN_POINT('Ctrl Pts',(-9.516475,1.9642208857481E-13,5.65457696757151));
#21752=CARTESIAN_POINT('Origin',(-8.5,0.,1.24542303242842));
#21753=CARTESIAN_POINT('',(-9.51651055362945,-2.20920755512588E-6,4.99542303242849));
#21754=CARTESIAN_POINT('',(-9.51596748085183,0.000899308347576677,5.05457696757151));
#21755=CARTESIAN_POINT('',(-9.516475,1.78524650477582E-12,1.24542303242842));
#21756=CARTESIAN_POINT('Ctrl Pts',(-9.516475,1.83425324399812E-13,4.99542303242849));
#21757=CARTESIAN_POINT('Ctrl Pts',(-9.51647500000005,-0.265706620583785,
5.00790396567668));
#21758=CARTESIAN_POINT('Ctrl Pts',(-9.40727465387205,-0.529786878176977,
5.02038489892487));
#21759=CARTESIAN_POINT('Ctrl Pts',(-9.21961691907768,-0.717894780174742,
5.03286583217306));
#21760=CARTESIAN_POINT('Ctrl Pts',(-9.03195918428332,-0.906002682172508,
5.04534676542125));
#21761=CARTESIAN_POINT('Ctrl Pts',(-8.7681413283437,-1.01583545019911,5.05782769866944));
#21762=CARTESIAN_POINT('Ctrl Pts',(-8.50243547044495,-1.0164720823066,5.07030863191763));
#21763=CARTESIAN_POINT('Ctrl Pts',(-8.2367296125462,-1.01710871441409,5.08278956516582));
#21764=CARTESIAN_POINT('Ctrl Pts',(-7.97238846933326,-0.908541417082708,
5.09527049841401));
#21765=CARTESIAN_POINT('Ctrl Pts',(-7.78383148002333,-0.721334926798515,
5.1077514316622));
#21766=CARTESIAN_POINT('Ctrl Pts',(-7.59527449071339,-0.534128436514322,
5.12023236491039));
#21767=CARTESIAN_POINT('Ctrl Pts',(-7.484809931317,-0.270574496755639,5.13271329815858));
#21768=CARTESIAN_POINT('Ctrl Pts',(-7.48353667075686,-0.00487092690815026,
5.14519423140677));
#21769=CARTESIAN_POINT('Ctrl Pts',(-7.48226341019671,0.260832642939338,
5.15767516465496));
#21770=CARTESIAN_POINT('Ctrl Pts',(-7.59019703546757,0.525433154240528,
5.17015609790315));
#21771=CARTESIAN_POINT('Ctrl Pts',(-7.77695120652526,0.71443814839335,5.18263703115134));
#21772=CARTESIAN_POINT('Ctrl Pts',(-7.96370537758295,0.903443142546172,
5.19511796439953));
#21773=CARTESIAN_POINT('Ctrl Pts',(-8.22699388814839,1.01453885915662,5.20759889764772));
#21774=CARTESIAN_POINT('Ctrl Pts',(-8.4926936445917,1.01644874085989,5.22007983089591));
#21775=CARTESIAN_POINT('Ctrl Pts',(-8.75839340103501,1.01835862256315,5.23256076414411));
#21776=CARTESIAN_POINT('Ctrl Pts',(-9.02325176140398,0.911059288978924,
5.2450416973923));
#21777=CARTESIAN_POINT('Ctrl Pts',(-9.2127036753585,0.724758509267391,5.25752263064049));
#21778=CARTESIAN_POINT('Ctrl Pts',(-9.40215558931301,0.538457729555859,
5.27000356388868));
#21779=CARTESIAN_POINT('Ctrl Pts',(-9.51388182535846,0.275436159672174,
5.28248449713687));
#21780=CARTESIAN_POINT('Ctrl Pts',(-9.51642831724057,0.00974174196407231,
5.29496543038506));
#21781=CARTESIAN_POINT('Ctrl Pts',(-9.51645943884197,0.00649459406647103,
5.29511796439953));
#21782=CARTESIAN_POINT('Ctrl Pts',(-9.516475,0.00324729703355204,5.29527049841401));
#21783=CARTESIAN_POINT('Ctrl Pts',(-9.516475,1.76451799697528E-13,5.29542303242849));
#21784=CARTESIAN_POINT('Ctrl Pts',(-9.51596748085183,0.000899308347576649,
5.05457696757151));
#21785=CARTESIAN_POINT('Ctrl Pts',(-9.51393632712024,-0.244280703320957,
5.06608589723497));
#21786=CARTESIAN_POINT('Ctrl Pts',(-9.30196512874467,-0.831606259329029,
5.09350216805006));
#21787=CARTESIAN_POINT('Ctrl Pts',(-8.31719720097595,-1.18865749368552,
5.13682578001674));
#21788=CARTESIAN_POINT('Ctrl Pts',(-7.55616952889954,-0.605685554543534,
5.17659413289581));
#21789=CARTESIAN_POINT('Ctrl Pts',(-7.44670579394524,0.0847130526542142,
5.20840881519905));
#21790=CARTESIAN_POINT('Ctrl Pts',(-7.66510184151263,0.748742955970089,
5.2402234975023));
#21791=CARTESIAN_POINT('Ctrl Pts',(-8.50951785842748,1.20259424204374,5.27999185038134));
#21792=CARTESIAN_POINT('Ctrl Pts',(-9.37060850264513,0.722810098535887,
5.32076089726302));
#21793=CARTESIAN_POINT('Ctrl Pts',(-9.51441702760733,0.190923916089248,
5.34562260299307));
#21794=CARTESIAN_POINT('Ctrl Pts',(-9.51491083301307,-0.000352273535940736,
5.35457696757151));
#21795=CARTESIAN_POINT('Origin',(-8.5,0.,1.24542303242842));
#21796=CARTESIAN_POINT('',(-9.51625559736582,-0.000198078035846429,4.69542303242848));
#21797=CARTESIAN_POINT('',(-9.5168797764423,1.75559250602679E-5,4.75457696757151));
#21798=CARTESIAN_POINT('',(-9.516475,1.78524650477582E-12,1.24542303242842));
#21799=CARTESIAN_POINT('Ctrl Pts',(-9.51546470589177,-0.000912099681457321,
4.69542303242849));
#21800=CARTESIAN_POINT('Ctrl Pts',(-9.51640331012323,-0.11186706289642,
4.70062983186786));
#21801=CARTESIAN_POINT('Ctrl Pts',(-9.44878420264641,-0.560795848238884,
4.72174397245884));
#21802=CARTESIAN_POINT('Ctrl Pts',(-8.79017906601008,-1.16700051389882,
4.75876545420146));
#21803=CARTESIAN_POINT('Ctrl Pts',(-7.6762153949145,-0.874872134276515,
4.80648747765633));
#21804=CARTESIAN_POINT('Ctrl Pts',(-7.3176700873064,0.219522361823356,4.85420950111118));
#21805=CARTESIAN_POINT('Ctrl Pts',(-8.04665782451571,1.11391398795103,4.90193152456605));
#21806=CARTESIAN_POINT('Ctrl Pts',(-8.99902690165246,1.00431225253282,4.9416998774451));
#21807=CARTESIAN_POINT('Ctrl Pts',(-9.43822092306757,0.478999650422338,
4.97286371339925));
#21808=CARTESIAN_POINT('Ctrl Pts',(-9.51760254656266,0.154825683554372,
4.98812020820177));
#21809=CARTESIAN_POINT('Ctrl Pts',(-9.51778639424793,-8.14865418414124E-5,
4.99542303242849));
#21810=CARTESIAN_POINT('Ctrl Pts',(-9.51823949807117,7.65296501495289E-5,
4.75457696757151));
#21811=CARTESIAN_POINT('Ctrl Pts',(-9.51824207547116,-0.0032626182231765,
4.75473450917363));
#21812=CARTESIAN_POINT('Ctrl Pts',(-9.51666993996602,-0.343764340190618,
4.77079939192736));
#21813=CARTESIAN_POINT('Ctrl Pts',(-9.13946832655052,-1.01853019590215,
4.80277161583271));
#21814=CARTESIAN_POINT('Ctrl Pts',(-8.18251236732564,-1.0755801003455,4.84253996871177));
#21815=CARTESIAN_POINT('Ctrl Pts',(-7.64801679391654,-0.625083676278862,
4.87435465101502));
#21816=CARTESIAN_POINT('Ctrl Pts',(-7.37871875701052,0.0199830748479729,
4.90616933331825));
#21817=CARTESIAN_POINT('Ctrl Pts',(-7.72036584095294,0.915693223013455,
4.94593768619731));
#21818=CARTESIAN_POINT('Ctrl Pts',(-8.85007720703,1.15045210196194,4.99365970965217));
#21819=CARTESIAN_POINT('Ctrl Pts',(-9.46169735923061,0.526259520213707,
5.02987280344356));
#21820=CARTESIAN_POINT('Ctrl Pts',(-9.5167437346103,0.0946006873223545,
5.05017855608335));
#21821=CARTESIAN_POINT('Ctrl Pts',(-9.51596748085183,0.000899308347576649,
5.05457696757151));
#21822=CARTESIAN_POINT('Origin',(-8.5,0.,1.24542303242842));
#21823=CARTESIAN_POINT('',(-9.51614091975708,0.000208621397402929,4.39542303242849));
#21824=CARTESIAN_POINT('',(-9.516475,2.24316187383949E-13,4.45457696757151));
#21825=CARTESIAN_POINT('',(-9.516475,1.78524650477582E-12,1.24542303242842));
#21826=CARTESIAN_POINT('Ctrl Pts',(-9.516475,1.97372373804382E-13,4.39542303242849));
#21827=CARTESIAN_POINT('Ctrl Pts',(-9.51647500000005,-0.265706620583771,
4.40790396567668));
#21828=CARTESIAN_POINT('Ctrl Pts',(-9.40727465387206,-0.529786878176964,
4.42038489892487));
#21829=CARTESIAN_POINT('Ctrl Pts',(-9.21961691907769,-0.717894780174732,
4.43286583217306));
#21830=CARTESIAN_POINT('Ctrl Pts',(-9.03195918428333,-0.9060026821725,4.44534676542125));
#21831=CARTESIAN_POINT('Ctrl Pts',(-8.76814132834372,-1.01583545019911,
4.45782769866944));
#21832=CARTESIAN_POINT('Ctrl Pts',(-8.50243547044496,-1.0164720823066,4.47030863191763));
#21833=CARTESIAN_POINT('Ctrl Pts',(-8.23672961254621,-1.01710871441409,
4.48278956516582));
#21834=CARTESIAN_POINT('Ctrl Pts',(-7.97238846933327,-0.908541417082715,
4.49527049841401));
#21835=CARTESIAN_POINT('Ctrl Pts',(-7.78383148002334,-0.721334926798525,
4.5077514316622));
#21836=CARTESIAN_POINT('Ctrl Pts',(-7.5952744907134,-0.534128436514334,
4.52023236491039));
#21837=CARTESIAN_POINT('Ctrl Pts',(-7.48480993131701,-0.270574496755652,
4.53271329815858));
#21838=CARTESIAN_POINT('Ctrl Pts',(-7.48353667075686,-0.0048709269081642,
4.54519423140677));
#21839=CARTESIAN_POINT('Ctrl Pts',(-7.48226341019671,0.260832642939324,
4.55767516465496));
#21840=CARTESIAN_POINT('Ctrl Pts',(-7.59019703546756,0.525433154240515,
4.57015609790315));
#21841=CARTESIAN_POINT('Ctrl Pts',(-7.77695120652525,0.71443814839334,4.58263703115134));
#21842=CARTESIAN_POINT('Ctrl Pts',(-7.96370537758293,0.903443142546165,
4.59511796439953));
#21843=CARTESIAN_POINT('Ctrl Pts',(-8.22699388814838,1.01453885915662,4.60759889764772));
#21844=CARTESIAN_POINT('Ctrl Pts',(-8.49269364459169,1.01644874085989,4.62007983089591));
#21845=CARTESIAN_POINT('Ctrl Pts',(-8.75839340103499,1.01835862256315,4.63256076414411));
#21846=CARTESIAN_POINT('Ctrl Pts',(-9.02325176140397,0.911059288978931,
4.64504169739229));
#21847=CARTESIAN_POINT('Ctrl Pts',(-9.21270367535849,0.724758509267401,
4.65752263064049));
#21848=CARTESIAN_POINT('Ctrl Pts',(-9.402155589313,0.538457729555871,4.67000356388868));
#21849=CARTESIAN_POINT('Ctrl Pts',(-9.51388182535845,0.275436159672188,
4.68248449713687));
#21850=CARTESIAN_POINT('Ctrl Pts',(-9.51642831724057,0.00974174196408626,
4.69496543038506));
#21851=CARTESIAN_POINT('Ctrl Pts',(-9.51645943884197,0.00649459406648979,
4.69511796439953));
#21852=CARTESIAN_POINT('Ctrl Pts',(-9.516475,0.00324729703357563,4.69527049841401));
#21853=CARTESIAN_POINT('Ctrl Pts',(-9.516475,2.04843827648732E-13,4.69542303242848));
#21854=CARTESIAN_POINT('Ctrl Pts',(-9.516475,2.24316187383949E-13,4.45457696757151));
#21855=CARTESIAN_POINT('Ctrl Pts',(-9.51647500000006,-0.265706620583744,
4.4670579008197));
#21856=CARTESIAN_POINT('Ctrl Pts',(-9.40727465387207,-0.52978687817694,
4.47953883406789));
#21857=CARTESIAN_POINT('Ctrl Pts',(-9.21961691907771,-0.717894780174713,
4.49201976731608));
#21858=CARTESIAN_POINT('Ctrl Pts',(-9.03195918428336,-0.906002682172486,
4.50450070056427));
#21859=CARTESIAN_POINT('Ctrl Pts',(-8.76814132834374,-1.0158354501991,4.51698163381246));
#21860=CARTESIAN_POINT('Ctrl Pts',(-8.50243547044499,-1.0164720823066,4.52946256706065));
#21861=CARTESIAN_POINT('Ctrl Pts',(-8.23672961254624,-1.0171087144141,4.54194350030884));
#21862=CARTESIAN_POINT('Ctrl Pts',(-7.9723884693333,-0.908541417082729,
4.55442443355703));
#21863=CARTESIAN_POINT('Ctrl Pts',(-7.78383148002335,-0.721334926798543,
4.56690536680522));
#21864=CARTESIAN_POINT('Ctrl Pts',(-7.59527449071341,-0.534128436514358,
4.57938630005341));
#21865=CARTESIAN_POINT('Ctrl Pts',(-7.48480993131702,-0.270574496755679,
4.5918672333016));
#21866=CARTESIAN_POINT('Ctrl Pts',(-7.48353667075686,-0.00487092690819115,
4.60434816654979));
#21867=CARTESIAN_POINT('Ctrl Pts',(-7.4822634101967,0.260832642939297,4.61682909979799));
#21868=CARTESIAN_POINT('Ctrl Pts',(-7.59019703546755,0.525433154240491,
4.62931003304617));
#21869=CARTESIAN_POINT('Ctrl Pts',(-7.77695120652523,0.714438148393321,
4.64179096629437));
#21870=CARTESIAN_POINT('Ctrl Pts',(-7.96370537758291,0.90344314254615,4.65427189954256));
#21871=CARTESIAN_POINT('Ctrl Pts',(-8.22699388814835,1.01453885915661,4.66675283279075));
#21872=CARTESIAN_POINT('Ctrl Pts',(-8.49269364459166,1.01644874085989,4.67923376603894));
#21873=CARTESIAN_POINT('Ctrl Pts',(-8.75839340103497,1.01835862256316,4.69171469928713));
#21874=CARTESIAN_POINT('Ctrl Pts',(-9.02325176140395,0.911059288978945,
4.70419563253532));
#21875=CARTESIAN_POINT('Ctrl Pts',(-9.21270367535847,0.72475850926742,4.71667656578351));
#21876=CARTESIAN_POINT('Ctrl Pts',(-9.40215558931299,0.538457729555895,
4.7291574990317));
#21877=CARTESIAN_POINT('Ctrl Pts',(-9.51388182535845,0.275436159672215,
4.74163843227989));
#21878=CARTESIAN_POINT('Ctrl Pts',(-9.51642831724057,0.00974174196411321,
4.75411936552808));
#21879=CARTESIAN_POINT('Ctrl Pts',(-9.51645943884197,0.00649459406651192,
4.75427189954256));
#21880=CARTESIAN_POINT('Ctrl Pts',(-9.516475,0.00324729703359293,4.75442443355703));
#21881=CARTESIAN_POINT('Ctrl Pts',(-9.516475,2.17342662681664E-13,4.75457696757151));
#21882=CARTESIAN_POINT('Origin',(-8.5,0.,1.24542303242842));
#21883=CARTESIAN_POINT('',(-9.51670427207195,7.39794657305722E-5,4.09542303242849));
#21884=CARTESIAN_POINT('',(-9.51599658147032,0.000173149125154374,4.15457696757151));
#21885=CARTESIAN_POINT('',(-9.516475,1.78524650477582E-12,1.24542303242842));
#21886=CARTESIAN_POINT('Ctrl Pts',(-9.51784765822069,0.000442917101461892,
4.09542303242849));
#21887=CARTESIAN_POINT('Ctrl Pts',(-9.51577594300805,-0.303314166886826,
4.10974173804841));
#21888=CARTESIAN_POINT('Ctrl Pts',(-9.20951320363247,-0.947629617697905,
4.13996778481995));
#21889=CARTESIAN_POINT('Ctrl Pts',(-8.11269623164964,-1.13845943309904,
4.18610117274311));
#21890=CARTESIAN_POINT('Ctrl Pts',(-7.3324614462396,-0.288404622204439,
4.23382319619797));
#21891=CARTESIAN_POINT('Ctrl Pts',(-7.57791048256601,0.638296068450016,
4.27359154907703));
#21892=CARTESIAN_POINT('Ctrl Pts',(-8.17310957881519,1.0048619996478,4.30540623138027));
#21893=CARTESIAN_POINT('Ctrl Pts',(-8.87006013423126,1.05864368236586,4.33722091368351));
#21894=CARTESIAN_POINT('Ctrl Pts',(-9.43118836112104,0.602224246389519,
4.36722651403292));
#21895=CARTESIAN_POINT('Ctrl Pts',(-9.51585152810173,0.132104578598546,
4.38927844380651));
#21896=CARTESIAN_POINT('Ctrl Pts',(-9.5151537803744,0.000825055327915034,
4.39542303242849));
#21897=CARTESIAN_POINT('Ctrl Pts',(-9.516475,2.38512201359551E-13,4.15457696757151));
#21898=CARTESIAN_POINT('Ctrl Pts',(-9.51647500000006,-0.26570662058373,
4.1670579008197));
#21899=CARTESIAN_POINT('Ctrl Pts',(-9.40727465387208,-0.529786878176927,
4.17953883406789));
#21900=CARTESIAN_POINT('Ctrl Pts',(-9.21961691907772,-0.717894780174703,
4.19201976731608));
#21901=CARTESIAN_POINT('Ctrl Pts',(-9.03195918428337,-0.906002682172479,
4.20450070056427));
#21902=CARTESIAN_POINT('Ctrl Pts',(-8.76814132834376,-1.01583545019909,
4.21698163381246));
#21903=CARTESIAN_POINT('Ctrl Pts',(-8.502435470445,-1.0164720823066,4.22946256706065));
#21904=CARTESIAN_POINT('Ctrl Pts',(-8.23672961254625,-1.0171087144141,4.24194350030884));
#21905=CARTESIAN_POINT('Ctrl Pts',(-7.97238846933331,-0.908541417082736,
4.25442443355703));
#21906=CARTESIAN_POINT('Ctrl Pts',(-7.78383148002336,-0.721334926798554,
4.26690536680522));
#21907=CARTESIAN_POINT('Ctrl Pts',(-7.59527449071342,-0.534128436514371,
4.27938630005341));
#21908=CARTESIAN_POINT('Ctrl Pts',(-7.48480993131702,-0.270574496755694,
4.2918672333016));
#21909=CARTESIAN_POINT('Ctrl Pts',(-7.48353667075686,-0.00487092690820534,
4.30434816654979));
#21910=CARTESIAN_POINT('Ctrl Pts',(-7.48226341019669,0.260832642939283,
4.31682909979798));
#21911=CARTESIAN_POINT('Ctrl Pts',(-7.59019703546754,0.525433154240478,
4.32931003304617));
#21912=CARTESIAN_POINT('Ctrl Pts',(-7.77695120652522,0.714438148393311,
4.34179096629437));
#21913=CARTESIAN_POINT('Ctrl Pts',(-7.9637053775829,0.903443142546145,4.35427189954256));
#21914=CARTESIAN_POINT('Ctrl Pts',(-8.22699388814834,1.01453885915661,4.36675283279075));
#21915=CARTESIAN_POINT('Ctrl Pts',(-8.49269364459165,1.01644874085989,4.37923376603894));
#21916=CARTESIAN_POINT('Ctrl Pts',(-8.75839340103496,1.01835862256316,4.39171469928713));
#21917=CARTESIAN_POINT('Ctrl Pts',(-9.02325176140394,0.911059288978948,
4.40419563253532));
#21918=CARTESIAN_POINT('Ctrl Pts',(-9.21270367535846,0.724758509267425,
4.41667656578351));
#21919=CARTESIAN_POINT('Ctrl Pts',(-9.40215558931298,0.538457729555901,
4.4291574990317));
#21920=CARTESIAN_POINT('Ctrl Pts',(-9.51388182535844,0.275436159672222,
4.44163843227989));
#21921=CARTESIAN_POINT('Ctrl Pts',(-9.51642831724057,0.00974174196412018,
4.45411936552808));
#21922=CARTESIAN_POINT('Ctrl Pts',(-9.51645943884197,0.00649459406651889,
4.45427189954256));
#21923=CARTESIAN_POINT('Ctrl Pts',(-9.516475,0.00324729703359991,4.45442443355703));
#21924=CARTESIAN_POINT('Ctrl Pts',(-9.516475,2.24316187383949E-13,4.45457696757151));
#21925=CARTESIAN_POINT('Origin',(-8.5,0.,1.24542303242842));
#21926=CARTESIAN_POINT('',(-9.516475,2.11319423208952E-13,3.79542303242848));
#21927=CARTESIAN_POINT('',(-9.51647837596764,1.62386119748113E-6,3.85457696757151));
#21928=CARTESIAN_POINT('',(-9.516475,1.78524650477582E-12,1.24542303242842));
#21929=CARTESIAN_POINT('Ctrl Pts',(-9.516475,2.25764401755587E-13,3.79542303242848));
#21930=CARTESIAN_POINT('Ctrl Pts',(-9.51647500000006,-0.265706620583743,
3.80790396567667));
#21931=CARTESIAN_POINT('Ctrl Pts',(-9.40727465387207,-0.529786878176939,
3.82038489892486));
#21932=CARTESIAN_POINT('Ctrl Pts',(-9.21961691907771,-0.717894780174712,
3.83286583217305));
#21933=CARTESIAN_POINT('Ctrl Pts',(-9.03195918428336,-0.906002682172486,
3.84534676542125));
#21934=CARTESIAN_POINT('Ctrl Pts',(-8.76814132834375,-1.0158354501991,3.85782769866944));
#21935=CARTESIAN_POINT('Ctrl Pts',(-8.50243547044499,-1.0164720823066,3.87030863191763));
#21936=CARTESIAN_POINT('Ctrl Pts',(-8.23672961254624,-1.0171087144141,3.88278956516582));
#21937=CARTESIAN_POINT('Ctrl Pts',(-7.9723884693333,-0.908541417082729,
3.89527049841401));
#21938=CARTESIAN_POINT('Ctrl Pts',(-7.78383148002336,-0.721334926798544,
3.9077514316622));
#21939=CARTESIAN_POINT('Ctrl Pts',(-7.59527449071341,-0.53412843651436,
3.92023236491039));
#21940=CARTESIAN_POINT('Ctrl Pts',(-7.48480993131702,-0.270574496755681,
3.93271329815858));
#21941=CARTESIAN_POINT('Ctrl Pts',(-7.48353667075686,-0.0048709269081926,
3.94519423140677));
#21942=CARTESIAN_POINT('Ctrl Pts',(-7.4822634101967,0.260832642939296,3.95767516465496));
#21943=CARTESIAN_POINT('Ctrl Pts',(-7.59019703546755,0.52543315424049,3.97015609790315));
#21944=CARTESIAN_POINT('Ctrl Pts',(-7.77695120652523,0.71443814839332,3.98263703115134));
#21945=CARTESIAN_POINT('Ctrl Pts',(-7.96370537758291,0.90344314254615,3.99511796439953));
#21946=CARTESIAN_POINT('Ctrl Pts',(-8.22699388814835,1.01453885915661,4.00759889764772));
#21947=CARTESIAN_POINT('Ctrl Pts',(-8.49269364459166,1.01644874085989,4.02007983089591));
#21948=CARTESIAN_POINT('Ctrl Pts',(-8.75839340103497,1.01835862256316,4.0325607641441));
#21949=CARTESIAN_POINT('Ctrl Pts',(-9.02325176140394,0.911059288978945,
4.04504169739229));
#21950=CARTESIAN_POINT('Ctrl Pts',(-9.21270367535847,0.724758509267421,
4.05752263064048));
#21951=CARTESIAN_POINT('Ctrl Pts',(-9.40215558931299,0.538457729555896,
4.07000356388867));
#21952=CARTESIAN_POINT('Ctrl Pts',(-9.51388182535845,0.275436159672217,
4.08248449713686));
#21953=CARTESIAN_POINT('Ctrl Pts',(-9.51642831724057,0.00974174196411465,
4.09496543038505));
#21954=CARTESIAN_POINT('Ctrl Pts',(-9.51645943884197,0.00649459406651096,
4.09511796439953));
#21955=CARTESIAN_POINT('Ctrl Pts',(-9.516475,0.00324729703358956,4.09527049841401));
#21956=CARTESIAN_POINT('Ctrl Pts',(-9.516475,2.11568387779985E-13,4.09542303242848));
#21957=CARTESIAN_POINT('Ctrl Pts',(-9.5174412885927,0.000464791732992929,
3.85457696757151));
#21958=CARTESIAN_POINT('Ctrl Pts',(-9.51678187338335,-0.124250478191715,
3.86044869786864));
#21959=CARTESIAN_POINT('Ctrl Pts',(-9.45952256246098,-0.418651775766005,
3.87427409874159));
#21960=CARTESIAN_POINT('Ctrl Pts',(-9.08719526120723,-0.955443705498223,
3.90400684076614));
#21961=CARTESIAN_POINT('Ctrl Pts',(-8.14851560934884,-1.15012269943444,
3.9437751936452));
#21962=CARTESIAN_POINT('Ctrl Pts',(-7.34215909770885,-0.324805379838734,
3.99149721710006));
#21963=CARTESIAN_POINT('Ctrl Pts',(-7.60098238778599,0.797364195232309,
4.03921924055492));
#21964=CARTESIAN_POINT('Ctrl Pts',(-8.68421342859387,1.18834317539854,4.08694126400978));
#21965=CARTESIAN_POINT('Ctrl Pts',(-9.42205359078049,0.622675900476843,
4.12539383968198));
#21966=CARTESIAN_POINT('Ctrl Pts',(-9.51547907546729,0.142299165762317,
4.14793907420255));
#21967=CARTESIAN_POINT('Ctrl Pts',(-9.51476624073027,0.000618433764589824,
4.15457696757151));
#21968=CARTESIAN_POINT('Origin',(-8.5,0.,1.24542303242842));
#21969=CARTESIAN_POINT('',(-9.51608842318713,-2.89235217017741E-5,3.49542303242848));
#21970=CARTESIAN_POINT('',(-9.516475,2.45236761490803E-13,3.55457696757151));
#21971=CARTESIAN_POINT('',(-9.516475,1.78524650477582E-12,1.24542303242842));
#21972=CARTESIAN_POINT('Ctrl Pts',(-9.51486126663803,-0.000120738881975849,
3.49542303242848));
#21973=CARTESIAN_POINT('Ctrl Pts',(-9.51514336021873,-0.160856911785796,
3.50294630307734));
#21974=CARTESIAN_POINT('Ctrl Pts',(-9.40340564418365,-0.6611996367537,3.52637691487781));
#21975=CARTESIAN_POINT('Ctrl Pts',(-8.61746895833269,-1.19688117390714,
3.5657148678299));
#21976=CARTESIAN_POINT('Ctrl Pts',(-7.73570976145469,-0.820689576164182,
3.60548322070896));
#21977=CARTESIAN_POINT('Ctrl Pts',(-7.4585680161445,-0.178953649869286,
3.6372979030122));
#21978=CARTESIAN_POINT('Ctrl Pts',(-7.50559368937304,0.518485331080344,
3.66911258531544));
#21979=CARTESIAN_POINT('Ctrl Pts',(-8.21119763983049,1.1674402328969,3.70888093819449));
#21980=CARTESIAN_POINT('Ctrl Pts',(-9.25750654792175,0.891435180077196,
3.75363564409078));
#21981=CARTESIAN_POINT('Ctrl Pts',(-9.51442267342405,0.274180741296169,
3.78248300883544));
#21982=CARTESIAN_POINT('Ctrl Pts',(-9.51684974171157,-0.000865705360034545,
3.79542303242848));
#21983=CARTESIAN_POINT('Ctrl Pts',(-9.516475,2.45236761490803E-13,3.55457696757151));
#21984=CARTESIAN_POINT('Ctrl Pts',(-9.51647500000006,-0.265706620583731,
3.5670579008197));
#21985=CARTESIAN_POINT('Ctrl Pts',(-9.40727465387207,-0.529786878176936,
3.57953883406789));
#21986=CARTESIAN_POINT('Ctrl Pts',(-9.21961691907771,-0.717894780174714,
3.59201976731608));
#21987=CARTESIAN_POINT('Ctrl Pts',(-9.03195918428335,-0.906002682172492,
3.60450070056427));
#21988=CARTESIAN_POINT('Ctrl Pts',(-8.76814132834373,-1.0158354501991,3.61698163381246));
#21989=CARTESIAN_POINT('Ctrl Pts',(-8.50243547044497,-1.0164720823066,3.62946256706065));
#21990=CARTESIAN_POINT('Ctrl Pts',(-8.23672961254621,-1.01710871441409,
3.64194350030884));
#21991=CARTESIAN_POINT('Ctrl Pts',(-7.97238846933326,-0.908541417082711,
3.65442443355703));
#21992=CARTESIAN_POINT('Ctrl Pts',(-7.78383148002332,-0.721334926798513,
3.66690536680522));
#21993=CARTESIAN_POINT('Ctrl Pts',(-7.59527449071338,-0.534128436514314,
3.67938630005342));
#21994=CARTESIAN_POINT('Ctrl Pts',(-7.484809931317,-0.270574496755621,3.69186723330161));
#21995=CARTESIAN_POINT('Ctrl Pts',(-7.48353667075686,-0.0048709269081254,
3.7043481665498));
#21996=CARTESIAN_POINT('Ctrl Pts',(-7.48226341019672,0.26083264293937,3.71682909979799));
#21997=CARTESIAN_POINT('Ctrl Pts',(-7.59019703546759,0.525433154240564,
3.72931003304618));
#21998=CARTESIAN_POINT('Ctrl Pts',(-7.77695120652529,0.714438148393383,
3.74179096629437));
#21999=CARTESIAN_POINT('Ctrl Pts',(-7.96370537758299,0.903443142546202,
3.75427189954256));
#22000=CARTESIAN_POINT('Ctrl Pts',(-8.22699388814845,1.01453885915664,3.76675283279075));
#22001=CARTESIAN_POINT('Ctrl Pts',(-8.49269364459177,1.01644874085989,3.77923376603894));
#22002=CARTESIAN_POINT('Ctrl Pts',(-8.75839340103508,1.01835862256313,3.79171469928713));
#22003=CARTESIAN_POINT('Ctrl Pts',(-9.02325176140406,0.911059288978882,
3.80419563253532));
#22004=CARTESIAN_POINT('Ctrl Pts',(-9.21270367535856,0.724758509267328,
3.81667656578351));
#22005=CARTESIAN_POINT('Ctrl Pts',(-9.40215558931306,0.538457729555774,
3.82915749903171));
#22006=CARTESIAN_POINT('Ctrl Pts',(-9.51388182535849,0.27543615967207,3.8416384322799));
#22007=CARTESIAN_POINT('Ctrl Pts',(-9.51642831724057,0.00974174196396079,
3.85411936552809));
#22008=CARTESIAN_POINT('Ctrl Pts',(-9.51645943884197,0.00649459406641969,
3.85427189954256));
#22009=CARTESIAN_POINT('Ctrl Pts',(-9.516475,0.0032472970335609,3.85442443355703));
#22010=CARTESIAN_POINT('Ctrl Pts',(-9.516475,2.45485726061836E-13,3.85457696757151));
#22011=CARTESIAN_POINT('Origin',(-8.5,0.,1.24542303242842));
#22012=CARTESIAN_POINT('',(-9.516475,2.25266472613521E-13,3.19542303242848));
#22013=CARTESIAN_POINT('',(-9.51601909668223,-0.000125713479535779,3.25457696757151));
#22014=CARTESIAN_POINT('',(-9.516475,1.78524650477582E-12,1.24542303242842));
#22015=CARTESIAN_POINT('Ctrl Pts',(-9.516475,2.32488961886839E-13,3.19542303242848));
#22016=CARTESIAN_POINT('Ctrl Pts',(-9.51647500000006,-0.265706620583743,
3.20790396567667));
#22017=CARTESIAN_POINT('Ctrl Pts',(-9.40727465387207,-0.529786878176947,
3.22038489892487));
#22018=CARTESIAN_POINT('Ctrl Pts',(-9.2196169190777,-0.717894780174723,
3.23286583217306));
#22019=CARTESIAN_POINT('Ctrl Pts',(-9.03195918428334,-0.906002682172499,
3.24534676542125));
#22020=CARTESIAN_POINT('Ctrl Pts',(-8.76814132834372,-1.01583545019911,
3.25782769866944));
#22021=CARTESIAN_POINT('Ctrl Pts',(-8.50243547044496,-1.0164720823066,3.27030863191763));
#22022=CARTESIAN_POINT('Ctrl Pts',(-8.2367296125462,-1.01710871441409,3.28278956516582));
#22023=CARTESIAN_POINT('Ctrl Pts',(-7.97238846933325,-0.908541417082704,
3.29527049841401));
#22024=CARTESIAN_POINT('Ctrl Pts',(-7.78383148002331,-0.721334926798503,
3.3077514316622));
#22025=CARTESIAN_POINT('Ctrl Pts',(-7.59527449071337,-0.534128436514303,
3.32023236491039));
#22026=CARTESIAN_POINT('Ctrl Pts',(-7.48480993131699,-0.270574496755608,
3.33271329815858));
#22027=CARTESIAN_POINT('Ctrl Pts',(-7.48353667075686,-0.00487092690811265,
3.34519423140677));
#22028=CARTESIAN_POINT('Ctrl Pts',(-7.48226341019672,0.260832642939383,
3.35767516465496));
#22029=CARTESIAN_POINT('Ctrl Pts',(-7.59019703546759,0.525433154240575,
3.37015609790315));
#22030=CARTESIAN_POINT('Ctrl Pts',(-7.7769512065253,0.714438148393392,3.38263703115135));
#22031=CARTESIAN_POINT('Ctrl Pts',(-7.963705377583,0.903443142546208,3.39511796439954));
#22032=CARTESIAN_POINT('Ctrl Pts',(-8.22699388814847,1.01453885915664,3.40759889764773));
#22033=CARTESIAN_POINT('Ctrl Pts',(-8.49269364459178,1.01644874085989,3.42007983089592));
#22034=CARTESIAN_POINT('Ctrl Pts',(-8.7583934010351,1.01835862256313,3.43256076414411));
#22035=CARTESIAN_POINT('Ctrl Pts',(-9.02325176140407,0.911059288978876,
3.4450416973923));
#22036=CARTESIAN_POINT('Ctrl Pts',(-9.21270367535857,0.724758509267319,
3.45752263064049));
#22037=CARTESIAN_POINT('Ctrl Pts',(-9.40215558931307,0.538457729555763,
3.47000356388868));
#22038=CARTESIAN_POINT('Ctrl Pts',(-9.51388182535849,0.275436159672058,
3.48248449713687));
#22039=CARTESIAN_POINT('Ctrl Pts',(-9.51642831724057,0.00974174196394805,
3.49496543038506));
#22040=CARTESIAN_POINT('Ctrl Pts',(-9.51645943884197,0.00649459406640212,
3.49511796439954));
#22041=CARTESIAN_POINT('Ctrl Pts',(-9.516475,0.00324729703353853,3.49527049841401));
#22042=CARTESIAN_POINT('Ctrl Pts',(-9.516475,2.18292947911237E-13,3.49542303242848));
#22043=CARTESIAN_POINT('Ctrl Pts',(-9.51464021331442,-0.000505934934279403,
3.25457696757151));
#22044=CARTESIAN_POINT('Ctrl Pts',(-9.51522438392244,-0.150599077304496,
3.26160693347338));
#22045=CARTESIAN_POINT('Ctrl Pts',(-9.41409897557488,-0.639618505323573,
3.28454424052688));
#22046=CARTESIAN_POINT('Ctrl Pts',(-8.65488608504732,-1.19252018450271,
3.32338888873198));
#22047=CARTESIAN_POINT('Ctrl Pts',(-7.58161436923836,-0.774977522330395,
3.37111091218686));
#22048=CARTESIAN_POINT('Ctrl Pts',(-7.35051106244356,0.353226941538064,
3.41883293564171));
#22049=CARTESIAN_POINT('Ctrl Pts',(-8.17695225324716,1.15843154909689,3.46655495909658));
#22050=CARTESIAN_POINT('Ctrl Pts',(-9.11055173066928,0.9406899241179,3.50632331197563));
#22051=CARTESIAN_POINT('Ctrl Pts',(-9.46480985202421,0.402086870851785,
3.53566398146727));
#22052=CARTESIAN_POINT('Ctrl Pts',(-9.51660454730387,0.115906227021547,
3.54909730980729));
#22053=CARTESIAN_POINT('Ctrl Pts',(-9.5172889590067,-0.000538403642920175,
3.55457696757151));
#22054=CARTESIAN_POINT('Origin',(-8.5,0.,1.24542303242842));
#22055=CARTESIAN_POINT('',(-9.516475,2.32239997315806E-13,2.89542303242848));
#22056=CARTESIAN_POINT('',(-9.516475,2.59183810895373E-13,2.95457696757151));
#22057=CARTESIAN_POINT('',(-9.516475,1.78524650477582E-12,1.24542303242842));
#22058=CARTESIAN_POINT('Ctrl Pts',(-9.516475,2.39462486589124E-13,2.89542303242848));
#22059=CARTESIAN_POINT('Ctrl Pts',(-9.51647500000006,-0.265706620583729,
2.90790396567667));
#22060=CARTESIAN_POINT('Ctrl Pts',(-9.40727465387208,-0.529786878176927,
2.92038489892486));
#22061=CARTESIAN_POINT('Ctrl Pts',(-9.21961691907772,-0.717894780174703,
2.93286583217305));
#22062=CARTESIAN_POINT('Ctrl Pts',(-9.03195918428337,-0.906002682172478,
2.94534676542124));
#22063=CARTESIAN_POINT('Ctrl Pts',(-8.76814132834376,-1.01583545019909,
2.95782769866944));
#22064=CARTESIAN_POINT('Ctrl Pts',(-8.50243547044501,-1.0164720823066,2.97030863191763));
#22065=CARTESIAN_POINT('Ctrl Pts',(-8.23672961254625,-1.0171087144141,2.98278956516582));
#22066=CARTESIAN_POINT('Ctrl Pts',(-7.97238846933331,-0.908541417082737,
2.99527049841401));
#22067=CARTESIAN_POINT('Ctrl Pts',(-7.78383148002336,-0.721334926798554,
3.0077514316622));
#22068=CARTESIAN_POINT('Ctrl Pts',(-7.59527449071342,-0.534128436514372,
3.02023236491039));
#22069=CARTESIAN_POINT('Ctrl Pts',(-7.48480993131702,-0.270574496755695,
3.03271329815858));
#22070=CARTESIAN_POINT('Ctrl Pts',(-7.48353667075686,-0.00487092690820629,
3.04519423140677));
#22071=CARTESIAN_POINT('Ctrl Pts',(-7.48226341019669,0.260832642939282,
3.05767516465496));
#22072=CARTESIAN_POINT('Ctrl Pts',(-7.59019703546754,0.525433154240477,
3.07015609790315));
#22073=CARTESIAN_POINT('Ctrl Pts',(-7.77695120652522,0.71443814839331,3.08263703115134));
#22074=CARTESIAN_POINT('Ctrl Pts',(-7.9637053775829,0.903443142546142,3.09511796439953));
#22075=CARTESIAN_POINT('Ctrl Pts',(-8.22699388814834,1.01453885915661,3.10759889764772));
#22076=CARTESIAN_POINT('Ctrl Pts',(-8.49269364459164,1.01644874085989,3.12007983089591));
#22077=CARTESIAN_POINT('Ctrl Pts',(-8.75839340103495,1.01835862256316,3.1325607641441));
#22078=CARTESIAN_POINT('Ctrl Pts',(-9.02325176140393,0.911059288978952,
3.14504169739229));
#22079=CARTESIAN_POINT('Ctrl Pts',(-9.21270367535846,0.72475850926743,3.15752263064048));
#22080=CARTESIAN_POINT('Ctrl Pts',(-9.40215558931298,0.538457729555908,
3.17000356388867));
#22081=CARTESIAN_POINT('Ctrl Pts',(-9.51388182535844,0.27543615967223,3.18248449713686));
#22082=CARTESIAN_POINT('Ctrl Pts',(-9.51642831724057,0.00974174196412835,
3.19496543038505));
#22083=CARTESIAN_POINT('Ctrl Pts',(-9.51645943884197,0.00649459406652706,
3.19511796439953));
#22084=CARTESIAN_POINT('Ctrl Pts',(-9.516475,0.00324729703360808,3.19527049841401));
#22085=CARTESIAN_POINT('Ctrl Pts',(-9.516475,2.32488961886839E-13,3.19542303242848));
#22086=CARTESIAN_POINT('Ctrl Pts',(-9.516475,2.59183810895373E-13,2.95457696757151));
#22087=CARTESIAN_POINT('Ctrl Pts',(-9.51647500000007,-0.26570662058371,
2.9670579008197));
#22088=CARTESIAN_POINT('Ctrl Pts',(-9.40727465387209,-0.529786878176909,
2.97953883406789));
#22089=CARTESIAN_POINT('Ctrl Pts',(-9.21961691907774,-0.717894780174689,
2.99201976731608));
#22090=CARTESIAN_POINT('Ctrl Pts',(-9.03195918428339,-0.906002682172468,
3.00450070056427));
#22091=CARTESIAN_POINT('Ctrl Pts',(-8.76814132834378,-1.01583545019909,
3.01698163381246));
#22092=CARTESIAN_POINT('Ctrl Pts',(-8.50243547044503,-1.0164720823066,3.02946256706065));
#22093=CARTESIAN_POINT('Ctrl Pts',(-8.23672961254627,-1.01710871441411,
3.04194350030884));
#22094=CARTESIAN_POINT('Ctrl Pts',(-7.97238846933333,-0.908541417082747,
3.05442443355703));
#22095=CARTESIAN_POINT('Ctrl Pts',(-7.78383148002338,-0.721334926798568,
3.06690536680522));
#22096=CARTESIAN_POINT('Ctrl Pts',(-7.59527449071343,-0.534128436514389,
3.07938630005341));
#22097=CARTESIAN_POINT('Ctrl Pts',(-7.48480993131702,-0.270574496755714,
3.0918672333016));
#22098=CARTESIAN_POINT('Ctrl Pts',(-7.48353667075686,-0.00487092690822602,
3.10434816654979));
#22099=CARTESIAN_POINT('Ctrl Pts',(-7.48226341019669,0.260832642939262,
3.11682909979798));
#22100=CARTESIAN_POINT('Ctrl Pts',(-7.59019703546753,0.52543315424046,3.12931003304617));
#22101=CARTESIAN_POINT('Ctrl Pts',(-7.7769512065252,0.714438148393296,3.14179096629436));
#22102=CARTESIAN_POINT('Ctrl Pts',(-7.96370537758288,0.903443142546132,
3.15427189954255));
#22103=CARTESIAN_POINT('Ctrl Pts',(-8.22699388814832,1.0145388591566,3.16675283279075));
#22104=CARTESIAN_POINT('Ctrl Pts',(-8.49269364459163,1.01644874085989,3.17923376603894));
#22105=CARTESIAN_POINT('Ctrl Pts',(-8.75839340103493,1.01835862256317,3.19171469928713));
#22106=CARTESIAN_POINT('Ctrl Pts',(-9.02325176140392,0.911059288978963,
3.20419563253532));
#22107=CARTESIAN_POINT('Ctrl Pts',(-9.21270367535844,0.724758509267444,
3.21667656578351));
#22108=CARTESIAN_POINT('Ctrl Pts',(-9.40215558931297,0.538457729555926,
3.2291574990317));
#22109=CARTESIAN_POINT('Ctrl Pts',(-9.51388182535844,0.27543615967225,3.24163843227989));
#22110=CARTESIAN_POINT('Ctrl Pts',(-9.51642831724057,0.00974174196414807,
3.25411936552808));
#22111=CARTESIAN_POINT('Ctrl Pts',(-9.51645943884197,0.00649459406654679,
3.25427189954255));
#22112=CARTESIAN_POINT('Ctrl Pts',(-9.516475,0.0032472970336278,3.25442443355703));
#22113=CARTESIAN_POINT('Ctrl Pts',(-9.516475,2.52210286193088E-13,3.25457696757151));
#22114=CARTESIAN_POINT('Origin',(-8.5,0.,1.24542303242842));
#22115=CARTESIAN_POINT('',(-9.516475,2.31991032744774E-13,2.59542303242848));
#22116=CARTESIAN_POINT('',(-9.51688605890966,-5.38497483190686E-5,2.65457696757151));
#22117=CARTESIAN_POINT('',(-9.516475,1.78524650477582E-12,1.24542303242842));
#22118=CARTESIAN_POINT('Ctrl Pts',(-9.516475,2.35602277381432E-13,2.59542303242848));
#22119=CARTESIAN_POINT('Ctrl Pts',(-9.51647500000006,-0.265706620583739,
2.60790396567667));
#22120=CARTESIAN_POINT('Ctrl Pts',(-9.40727465387207,-0.529786878176942,
2.62038489892486));
#22121=CARTESIAN_POINT('Ctrl Pts',(-9.21961691907771,-0.717894780174718,
2.63286583217306));
#22122=CARTESIAN_POINT('Ctrl Pts',(-9.03195918428335,-0.906002682172494,
2.64534676542125));
#22123=CARTESIAN_POINT('Ctrl Pts',(-8.76814132834373,-1.0158354501991,2.65782769866944));
#22124=CARTESIAN_POINT('Ctrl Pts',(-8.50243547044496,-1.0164720823066,2.67030863191763));
#22125=CARTESIAN_POINT('Ctrl Pts',(-8.2367296125462,-1.01710871441409,2.68278956516582));
#22126=CARTESIAN_POINT('Ctrl Pts',(-7.97238846933326,-0.908541417082711,
2.69527049841401));
#22127=CARTESIAN_POINT('Ctrl Pts',(-7.78383148002332,-0.721334926798513,
2.7077514316622));
#22128=CARTESIAN_POINT('Ctrl Pts',(-7.59527449071338,-0.534128436514316,
2.72023236491039));
#22129=CARTESIAN_POINT('Ctrl Pts',(-7.484809931317,-0.270574496755625,2.73271329815858));
#22130=CARTESIAN_POINT('Ctrl Pts',(-7.48353667075686,-0.00487092690813021,
2.74519423140677));
#22131=CARTESIAN_POINT('Ctrl Pts',(-7.48226341019671,0.260832642939364,
2.75767516465496));
#22132=CARTESIAN_POINT('Ctrl Pts',(-7.59019703546758,0.525433154240557,
2.77015609790315));
#22133=CARTESIAN_POINT('Ctrl Pts',(-7.77695120652528,0.714438148393377,
2.78263703115134));
#22134=CARTESIAN_POINT('Ctrl Pts',(-7.96370537758299,0.903443142546197,
2.79511796439954));
#22135=CARTESIAN_POINT('Ctrl Pts',(-8.22699388814845,1.01453885915664,2.80759889764773));
#22136=CARTESIAN_POINT('Ctrl Pts',(-8.49269364459176,1.01644874085989,2.82007983089592));
#22137=CARTESIAN_POINT('Ctrl Pts',(-8.75839340103507,1.01835862256313,2.83256076414411));
#22138=CARTESIAN_POINT('Ctrl Pts',(-9.02325176140405,0.911059288978889,
2.8450416973923));
#22139=CARTESIAN_POINT('Ctrl Pts',(-9.21270367535855,0.724758509267339,
2.85752263064049));
#22140=CARTESIAN_POINT('Ctrl Pts',(-9.40215558931305,0.53845772955579,2.87000356388868));
#22141=CARTESIAN_POINT('Ctrl Pts',(-9.51388182535848,0.275436159672091,
2.88248449713687));
#22142=CARTESIAN_POINT('Ctrl Pts',(-9.51642831724057,0.00974174196398366,
2.89496543038506));
#22143=CARTESIAN_POINT('Ctrl Pts',(-9.51645943884197,0.00649459406643292,
2.89511796439953));
#22144=CARTESIAN_POINT('Ctrl Pts',(-9.516475,0.0032472970335645,2.89527049841401));
#22145=CARTESIAN_POINT('Ctrl Pts',(-9.516475,2.39462486589124E-13,2.89542303242848));
#22146=CARTESIAN_POINT('Ctrl Pts',(-9.516475,2.62546090960999E-13,2.65457696757151));
#22147=CARTESIAN_POINT('Ctrl Pts',(-9.51647500000007,-0.265706620583709,
2.6670579008197));
#22148=CARTESIAN_POINT('Ctrl Pts',(-9.40727465387209,-0.529786878176911,
2.67953883406789));
#22149=CARTESIAN_POINT('Ctrl Pts',(-9.21961691907774,-0.717894780174691,
2.69201976731608));
#22150=CARTESIAN_POINT('Ctrl Pts',(-9.03195918428338,-0.906002682172472,
2.70450070056427));
#22151=CARTESIAN_POINT('Ctrl Pts',(-8.76814132834377,-1.01583545019909,
2.71698163381246));
#22152=CARTESIAN_POINT('Ctrl Pts',(-8.50243547044501,-1.0164720823066,2.72946256706065));
#22153=CARTESIAN_POINT('Ctrl Pts',(-8.23672961254626,-1.0171087144141,2.74194350030884));
#22154=CARTESIAN_POINT('Ctrl Pts',(-7.97238846933331,-0.908541417082739,
2.75442443355703));
#22155=CARTESIAN_POINT('Ctrl Pts',(-7.78383148002337,-0.721334926798555,
2.76690536680522));
#22156=CARTESIAN_POINT('Ctrl Pts',(-7.59527449071342,-0.534128436514371,
2.77938630005341));
#22157=CARTESIAN_POINT('Ctrl Pts',(-7.48480993131702,-0.270574496755691,
2.7918672333016));
#22158=CARTESIAN_POINT('Ctrl Pts',(-7.48353667075686,-0.00487092690820049,
2.80434816654979));
#22159=CARTESIAN_POINT('Ctrl Pts',(-7.4822634101967,0.260832642939291,2.81682909979798));
#22160=CARTESIAN_POINT('Ctrl Pts',(-7.59019703546754,0.52543315424049,2.82931003304617));
#22161=CARTESIAN_POINT('Ctrl Pts',(-7.77695120652523,0.714438148393322,
2.84179096629437));
#22162=CARTESIAN_POINT('Ctrl Pts',(-7.96370537758291,0.903443142546153,
2.85427189954256));
#22163=CARTESIAN_POINT('Ctrl Pts',(-8.22699388814836,1.01453885915661,2.86675283279075));
#22164=CARTESIAN_POINT('Ctrl Pts',(-8.49269364459167,1.01644874085989,2.87923376603894));
#22165=CARTESIAN_POINT('Ctrl Pts',(-8.75839340103498,1.01835862256316,2.89171469928713));
#22166=CARTESIAN_POINT('Ctrl Pts',(-9.02325176140396,0.911059288978938,
2.90419563253532));
#22167=CARTESIAN_POINT('Ctrl Pts',(-9.21270367535848,0.724758509267409,
2.91667656578351));
#22168=CARTESIAN_POINT('Ctrl Pts',(-9.402155589313,0.538457729555879,2.9291574990317));
#22169=CARTESIAN_POINT('Ctrl Pts',(-9.51388182535845,0.275436159672194,
2.94163843227989));
#22170=CARTESIAN_POINT('Ctrl Pts',(-9.51642831724057,0.00974174196409005,
2.95411936552808));
#22171=CARTESIAN_POINT('Ctrl Pts',(-9.51645943884197,0.00649459406651043,
2.95427189954256));
#22172=CARTESIAN_POINT('Ctrl Pts',(-9.516475,0.00324729703361311,2.95442443355703));
#22173=CARTESIAN_POINT('Ctrl Pts',(-9.516475,2.59183810895373E-13,2.95457696757151));
#22174=CARTESIAN_POINT('Origin',(-8.5,0.,1.24542303242842));
#22175=CARTESIAN_POINT('',(-9.516475,2.31742068173741E-13,2.29542303242848));
#22176=CARTESIAN_POINT('',(-9.51574434509424,-0.000859751719978319,2.3545769675715));
#22177=CARTESIAN_POINT('',(-9.516475,1.78524650477582E-12,1.24542303242842));
#22178=CARTESIAN_POINT('Ctrl Pts',(-9.516475,2.28130823537082E-13,2.29542303242848));
#22179=CARTESIAN_POINT('Ctrl Pts',(-9.51647500000006,-0.265706620583739,
2.30790396567667));
#22180=CARTESIAN_POINT('Ctrl Pts',(-9.40727465387207,-0.529786878176934,
2.32038489892486));
#22181=CARTESIAN_POINT('Ctrl Pts',(-9.21961691907772,-0.717894780174708,
2.33286583217305));
#22182=CARTESIAN_POINT('Ctrl Pts',(-9.03195918428336,-0.906002682172482,
2.34534676542125));
#22183=CARTESIAN_POINT('Ctrl Pts',(-8.76814132834376,-1.0158354501991,2.35782769866944));
#22184=CARTESIAN_POINT('Ctrl Pts',(-8.502435470445,-1.0164720823066,2.37030863191763));
#22185=CARTESIAN_POINT('Ctrl Pts',(-8.23672961254625,-1.0171087144141,2.38278956516582));
#22186=CARTESIAN_POINT('Ctrl Pts',(-7.97238846933331,-0.908541417082736,
2.39527049841401));
#22187=CARTESIAN_POINT('Ctrl Pts',(-7.78383148002336,-0.721334926798554,
2.4077514316622));
#22188=CARTESIAN_POINT('Ctrl Pts',(-7.59527449071342,-0.534128436514372,
2.42023236491039));
#22189=CARTESIAN_POINT('Ctrl Pts',(-7.48480993131702,-0.270574496755696,
2.43271329815858));
#22190=CARTESIAN_POINT('Ctrl Pts',(-7.48353667075686,-0.00487092690820941,
2.44519423140677));
#22191=CARTESIAN_POINT('Ctrl Pts',(-7.48226341019669,0.260832642939278,
2.45767516465496));
#22192=CARTESIAN_POINT('Ctrl Pts',(-7.59019703546754,0.525433154240472,
2.47015609790315));
#22193=CARTESIAN_POINT('Ctrl Pts',(-7.77695120652521,0.714438148393305,
2.48263703115134));
#22194=CARTESIAN_POINT('Ctrl Pts',(-7.96370537758289,0.903443142546138,
2.49511796439953));
#22195=CARTESIAN_POINT('Ctrl Pts',(-8.22699388814833,1.0145388591566,2.50759889764772));
#22196=CARTESIAN_POINT('Ctrl Pts',(-8.49269364459163,1.01644874085989,2.52007983089591));
#22197=CARTESIAN_POINT('Ctrl Pts',(-8.75839340103494,1.01835862256317,2.5325607641441));
#22198=CARTESIAN_POINT('Ctrl Pts',(-9.02325176140392,0.911059288978959,
2.54504169739229));
#22199=CARTESIAN_POINT('Ctrl Pts',(-9.21270367535845,0.72475850926744,2.55752263064048));
#22200=CARTESIAN_POINT('Ctrl Pts',(-9.40215558931297,0.538457729555922,
2.57000356388867));
#22201=CARTESIAN_POINT('Ctrl Pts',(-9.51388182535844,0.275436159672246,
2.58248449713686));
#22202=CARTESIAN_POINT('Ctrl Pts',(-9.51642831724057,0.00974174196414591,
2.59496543038505));
#22203=CARTESIAN_POINT('Ctrl Pts',(-9.51645943884197,0.00649459406653981,
2.59511796439953));
#22204=CARTESIAN_POINT('Ctrl Pts',(-9.516475,0.00324729703361602,2.59527049841401));
#22205=CARTESIAN_POINT('Ctrl Pts',(-9.516475,2.35602277381432E-13,2.59542303242848));
#22206=CARTESIAN_POINT('Ctrl Pts',(-9.51574434509424,-0.000859751719978263,
2.35457696757151));
#22207=CARTESIAN_POINT('Ctrl Pts',(-9.51653441684081,-0.102971653508649,
2.35936745159258));
#22208=CARTESIAN_POINT('Ctrl Pts',(-9.45523207179823,-0.543196375581154,
2.38006527676528));
#22209=CARTESIAN_POINT('Ctrl Pts',(-8.8216302613637,-1.1587255804458,2.41667044308961));
#22210=CARTESIAN_POINT('Ctrl Pts',(-7.69804845902684,-0.896211681489087,
2.46439246654446));
#22211=CARTESIAN_POINT('Ctrl Pts',(-7.3785660134251,0.00764272958311676,
2.50416081942352));
#22212=CARTESIAN_POINT('Ctrl Pts',(-7.66367275817319,0.645880124738109,
2.53597550172676));
#22213=CARTESIAN_POINT('Ctrl Pts',(-8.2091023256041,1.0830742068233,2.56779018403));
#22214=CARTESIAN_POINT('Ctrl Pts',(-9.15872944113482,1.00294500423365,2.60732400597825));
#22215=CARTESIAN_POINT('Ctrl Pts',(-9.51774253405965,0.331986183950199,
2.63890415735069));
#22216=CARTESIAN_POINT('Ctrl Pts',(-9.51822696116145,-0.000229511307854096,
2.65457696757151));
#22217=CARTESIAN_POINT('Origin',(-8.5,0.,1.24542303242842));
#22218=CARTESIAN_POINT('',(-9.51753882530083,0.000269776910017053,1.99542303242848));
#22219=CARTESIAN_POINT('',(-9.51515984464674,0.00043457310919498,2.05457696757151));
#22220=CARTESIAN_POINT('',(-9.516475,1.78524650477582E-12,1.24542303242842));
#22221=CARTESIAN_POINT('Ctrl Pts',(-9.51753882530083,0.000269776910017103,
1.99542303242848));
#22222=CARTESIAN_POINT('Ctrl Pts',(-9.51701027049666,-0.136447844912708,
2.00186505680128));
#22223=CARTESIAN_POINT('Ctrl Pts',(-9.45149622815346,-0.44263766423451,
2.01626075174989));
#22224=CARTESIAN_POINT('Ctrl Pts',(-9.05259577107697,-0.975943072842501,
2.04656378785012));
#22225=CARTESIAN_POINT('Ctrl Pts',(-8.10737674978987,-1.1367365362355,2.08633214072917));
#22226=CARTESIAN_POINT('Ctrl Pts',(-7.33160128421964,-0.283165032011243,
2.13405416418404));
#22227=CARTESIAN_POINT('Ctrl Pts',(-7.62947585871493,0.829120622165689,
2.1817761876389));
#22228=CARTESIAN_POINT('Ctrl Pts',(-8.72792114609409,1.18088449447148,2.22949821109376));
#22229=CARTESIAN_POINT('Ctrl Pts',(-9.43137564348633,0.598121868949659,
2.26738049269029));
#22230=CARTESIAN_POINT('Ctrl Pts',(-9.51633032956077,0.129919845406597,
2.2893554331352));
#22231=CARTESIAN_POINT('Ctrl Pts',(-9.51583204610243,0.000442755438962029,
2.29542303242848));
#22232=CARTESIAN_POINT('Ctrl Pts',(-9.51515984464673,0.000434573109195022,
2.05457696757151));
#22233=CARTESIAN_POINT('Ctrl Pts',(-9.51434573427704,-0.199152432567874,
2.06392340468286));
#22234=CARTESIAN_POINT('Ctrl Pts',(-9.36064838525821,-0.739560899199373,
2.08917718294584));
#22235=CARTESIAN_POINT('Ctrl Pts',(-8.48010907733479,-1.20251427821691,
2.13033830236043));
#22236=CARTESIAN_POINT('Ctrl Pts',(-7.64681002815554,-0.727926671585552,
2.17010665523948));
#22237=CARTESIAN_POINT('Ctrl Pts',(-7.44498060597373,-0.0587522064326047,
2.20192133754272));
#22238=CARTESIAN_POINT('Ctrl Pts',(-7.57134386518546,0.628757665817628,
2.23373601984597));
#22239=CARTESIAN_POINT('Ctrl Pts',(-8.34654981722532,1.19279547618219,2.27350437272501));
#22240=CARTESIAN_POINT('Ctrl Pts',(-9.31336999826338,0.815051089939519,
2.3164359121588));
#22241=CARTESIAN_POINT('Ctrl Pts',(-9.51391089471827,0.236102404612829,
2.34346011044096));
#22242=CARTESIAN_POINT('Ctrl Pts',(-9.51574434509424,-0.000859751719978263,
2.35457696757151));
#22243=CARTESIAN_POINT('Origin',(-6.3,-1.5,1.1));
#22244=CARTESIAN_POINT('',(-6.45,-1.5,1.2));
#22245=CARTESIAN_POINT('Origin',(-6.3,-1.5,1.2));
#22246=CARTESIAN_POINT('',(-6.45,-1.5,1.8));
#22247=CARTESIAN_POINT('',(-6.45,-1.5,1.1));
#22248=CARTESIAN_POINT('Origin',(-6.3,-1.5,1.8));
#22249=CARTESIAN_POINT('Origin',(-10.7,1.5,1.1));
#22250=CARTESIAN_POINT('',(-10.85,1.5,1.2));
#22251=CARTESIAN_POINT('Origin',(-10.7,1.5,1.2));
#22252=CARTESIAN_POINT('',(-10.85,1.5,1.8));
#22253=CARTESIAN_POINT('',(-10.85,1.5,1.1));
#22254=CARTESIAN_POINT('Origin',(-10.7,1.5,1.8));
#22255=CARTESIAN_POINT('Origin',(-11.5,3.67394039744206E-16,1.1));
#22256=CARTESIAN_POINT('',(-11.83,3.26980695372343E-16,1.2));
#22257=CARTESIAN_POINT('Origin',(-11.5,3.67394039744206E-16,1.2));
#22258=CARTESIAN_POINT('',(-11.83,4.07807384116069E-16,1.8));
#22259=CARTESIAN_POINT('',(-11.83,3.26980695372343E-16,1.1));
#22260=CARTESIAN_POINT('Origin',(-11.5,3.67394039744206E-16,1.8));
#22261=CARTESIAN_POINT('Origin',(-8.5,3.,1.1));
#22262=CARTESIAN_POINT('',(-8.83,3.,1.2));
#22263=CARTESIAN_POINT('Origin',(-8.5,3.,1.2));
#22264=CARTESIAN_POINT('',(-8.83,3.,1.8));
#22265=CARTESIAN_POINT('',(-8.83,3.,1.1));
#22266=CARTESIAN_POINT('Origin',(-8.5,3.,1.8));
#22267=CARTESIAN_POINT('Origin',(-5.5,0.,1.1));
#22268=CARTESIAN_POINT('',(-5.83,-4.04133443718627E-17,1.2));
#22269=CARTESIAN_POINT('Origin',(-5.5,0.,1.2));
#22270=CARTESIAN_POINT('',(-5.83,4.04133443718627E-17,1.8));
#22271=CARTESIAN_POINT('',(-5.83,-4.04133443718627E-17,1.1));
#22272=CARTESIAN_POINT('Origin',(-5.5,0.,1.8));
#22273=CARTESIAN_POINT('Origin',(-8.5,-3.,1.1));
#22274=CARTESIAN_POINT('',(-8.83,-3.,1.2));
#22275=CARTESIAN_POINT('Origin',(-8.5,-3.,1.2));
#22276=CARTESIAN_POINT('',(-8.83,-3.,1.8));
#22277=CARTESIAN_POINT('',(-8.83,-3.,1.1));
#22278=CARTESIAN_POINT('Origin',(-8.5,-3.,1.8));
#22279=CARTESIAN_POINT('Origin',(-8.5,0.,1.8));
#22280=CARTESIAN_POINT('',(-12.3,-4.65365783675994E-16,1.8));
#22281=CARTESIAN_POINT('Origin',(-8.5,0.,1.8));
#22282=CARTESIAN_POINT('',(-9.09015970213932,-0.827606761448836,1.8));
#22283=CARTESIAN_POINT('Ctrl Pts',(-9.09015970213932,-0.827606761448836,
1.8));
#22284=CARTESIAN_POINT('Ctrl Pts',(-9.20517234022333,-0.758933651578936,
1.8));
#22285=CARTESIAN_POINT('Ctrl Pts',(-9.30543470625733,-0.668153006100454,
1.8));
#22286=CARTESIAN_POINT('Ctrl Pts',(-9.46867195483753,-0.450356182127565,
1.8));
#22287=CARTESIAN_POINT('Ctrl Pts',(-9.52880163313116,-0.3245091067028,1.8));
#22288=CARTESIAN_POINT('Ctrl Pts',(-9.59924924228391,-0.0529555869675627,
1.8));
#22289=CARTESIAN_POINT('Ctrl Pts',(-9.60735796710477,0.0905106217815908,
1.8));
#22290=CARTESIAN_POINT('Ctrl Pts',(-9.5683236154275,0.376768385137387,1.8));
#22291=CARTESIAN_POINT('Ctrl Pts',(-9.51999775237459,0.516568235234083,
1.8));
#22292=CARTESIAN_POINT('Ctrl Pts',(-9.39534294737136,0.731837239747713,
1.8));
#22293=CARTESIAN_POINT('Ctrl Pts',(-9.33251138248444,0.812979534739196,
1.8));
#22294=CARTESIAN_POINT('Ctrl Pts',(-9.18591685672465,0.958099062268399,
1.8));
#22295=CARTESIAN_POINT('Ctrl Pts',(-9.10245313248508,1.02107277613405,1.8));
#22296=CARTESIAN_POINT('Ctrl Pts',(-9.01183881116721,1.07233375495132,1.8));
#22297=CARTESIAN_POINT('',(-7.9098402978609,-0.827606761448988,1.8));
#22298=CARTESIAN_POINT('Ctrl Pts',(-7.98643053267018,1.07334645743582,1.8));
#22299=CARTESIAN_POINT('Ctrl Pts',(-7.95959869951212,1.05836761542859,1.8));
#22300=CARTESIAN_POINT('Ctrl Pts',(-7.93346058196618,1.04232411727427,1.8));
#22301=CARTESIAN_POINT('Ctrl Pts',(-7.90808767262475,1.02521683657119,1.8));
#22302=CARTESIAN_POINT('Ctrl Pts',(-7.86702659414781,0.997532057264915,
1.8));
#22303=CARTESIAN_POINT('Ctrl Pts',(-7.82796733446846,0.967063261293895,
1.8));
#22304=CARTESIAN_POINT('Ctrl Pts',(-7.79102854878543,0.934112112848264,
1.8));
#22305=CARTESIAN_POINT('Ctrl Pts',(-7.76028338488381,0.906685968729699,
1.8));
#22306=CARTESIAN_POINT('Ctrl Pts',(-7.7310076966407,0.877538967785464,1.8));
#22307=CARTESIAN_POINT('Ctrl Pts',(-7.70329177854206,0.846828311810782,
1.8));
#22308=CARTESIAN_POINT('Ctrl Pts',(-7.69029826921053,0.832430838360168,
1.8));
#22309=CARTESIAN_POINT('Ctrl Pts',(-7.67764787552771,0.817689530032765,
1.8));
#22310=CARTESIAN_POINT('Ctrl Pts',(-7.66535160389364,0.80261988762452,1.8));
#22311=CARTESIAN_POINT('Ctrl Pts',(-7.65904048382196,0.794885321773502,
1.8));
#22312=CARTESIAN_POINT('Ctrl Pts',(-7.65282266864073,0.787064257278584,
1.8));
#22313=CARTESIAN_POINT('Ctrl Pts',(-7.64669976589258,0.779158762650024,
1.8));
#22314=CARTESIAN_POINT('Ctrl Pts',(-7.64099494666391,0.771793070326609,
1.8));
#22315=CARTESIAN_POINT('Ctrl Pts',(-7.63537812199093,0.764361279600661,
1.8));
#22316=CARTESIAN_POINT('Ctrl Pts',(-7.62985175793421,0.75686774204179,1.8));
#22317=CARTESIAN_POINT('Ctrl Pts',(-7.60064975503062,0.717270946878432,
1.8));
#22318=CARTESIAN_POINT('Ctrl Pts',(-7.5739537660649,0.675931375403578,1.8));
#22319=CARTESIAN_POINT('Ctrl Pts',(-7.54988948683275,0.63313208044777,1.8));
#22320=CARTESIAN_POINT('Ctrl Pts',(-7.52509818071933,0.589039738746947,
1.8));
#22321=CARTESIAN_POINT('Ctrl Pts',(-7.5030992363447,0.543396988416792,1.8));
#22322=CARTESIAN_POINT('Ctrl Pts',(-7.48408397360475,0.496493124613758,
1.8));
#22323=CARTESIAN_POINT('Ctrl Pts',(-7.47536611429351,0.47498927839399,1.8));
#22324=CARTESIAN_POINT('Ctrl Pts',(-7.46727620351496,0.453220191275412,
1.8));
#22325=CARTESIAN_POINT('Ctrl Pts',(-7.4598369859861,0.4312134286592,1.8));
#22326=CARTESIAN_POINT('Ctrl Pts',(-7.45507728472205,0.417133236026627,
1.8));
#22327=CARTESIAN_POINT('Ctrl Pts',(-7.45058400712676,0.40295574861723,1.8));
#22328=CARTESIAN_POINT('Ctrl Pts',(-7.44636373622635,0.388688247459145,
1.8));
#22329=CARTESIAN_POINT('Ctrl Pts',(-7.44358828645132,0.379305263803885,
1.8));
#22330=CARTESIAN_POINT('Ctrl Pts',(-7.44093298062382,0.369890069488065,
1.8));
#22331=CARTESIAN_POINT('Ctrl Pts',(-7.43840114103695,0.360452578629106,
1.8));
#22332=CARTESIAN_POINT('Ctrl Pts',(-7.42603564356865,0.314359899642265,
1.8));
#22333=CARTESIAN_POINT('Ctrl Pts',(-7.41659412508323,0.267678796341731,
1.8));
#22334=CARTESIAN_POINT('Ctrl Pts',(-7.41022570586029,0.220657430426334,
1.8));
#22335=CARTESIAN_POINT('Ctrl Pts',(-7.40404692106448,0.175036234549352,
1.8));
#22336=CARTESIAN_POINT('Ctrl Pts',(-7.40076084230852,0.129093821696145,
1.8));
#22337=CARTESIAN_POINT('Ctrl Pts',(-7.40055260530635,0.0830577787951491,
1.8));
#22338=CARTESIAN_POINT('Ctrl Pts',(-7.40050727015443,0.0730352997103088,
1.8));
#22339=CARTESIAN_POINT('Ctrl Pts',(-7.40060800915348,0.0630084152029981,
1.8));
#22340=CARTESIAN_POINT('Ctrl Pts',(-7.40085706028656,0.0529795432811744,
1.8));
#22341=CARTESIAN_POINT('Ctrl Pts',(-7.40145499029249,0.028901903587719,
1.8));
#22342=CARTESIAN_POINT('Ctrl Pts',(-7.40290759789421,0.0048126866985071,
1.8));
#22343=CARTESIAN_POINT('Ctrl Pts',(-7.40520170800736,-0.0192454360660064,
1.8));
#22344=CARTESIAN_POINT('Ctrl Pts',(-7.4064626542103,-0.0324688634750262,
1.8));
#22345=CARTESIAN_POINT('Ctrl Pts',(-7.40797894405252,-0.0456892794148736,
1.8));
#22346=CARTESIAN_POINT('Ctrl Pts',(-7.40974342485787,-0.0588641207172785,
1.8));
#22347=CARTESIAN_POINT('Ctrl Pts',(-7.41592575380453,-0.105025689890607,
1.8));
#22348=CARTESIAN_POINT('Ctrl Pts',(-7.42515413053941,-0.15069465683366,
1.8));
#22349=CARTESIAN_POINT('Ctrl Pts',(-7.43727039345037,-0.195579452638668,
1.8));
#22350=CARTESIAN_POINT('Ctrl Pts',(-7.44982841714008,-0.24210075488916,
1.8));
#22351=CARTESIAN_POINT('Ctrl Pts',(-7.46548913747226,-0.28778107330993,
1.8));
#22352=CARTESIAN_POINT('Ctrl Pts',(-7.4841298525239,-0.332272113546041,
1.8));
#22353=CARTESIAN_POINT('Ctrl Pts',(-7.49345021004971,-0.354517633664097,
1.8));
#22354=CARTESIAN_POINT('Ctrl Pts',(-7.50351634802847,-0.376465335519361,
1.8));
#22355=CARTESIAN_POINT('Ctrl Pts',(-7.51431717419396,-0.398067850985725,
1.8));
#22356=CARTESIAN_POINT('Ctrl Pts',(-7.51944823894934,-0.408330390539524,
1.8));
#22357=CARTESIAN_POINT('Ctrl Pts',(-7.52474514890817,-0.418514983219543,
1.8));
#22358=CARTESIAN_POINT('Ctrl Pts',(-7.53020690911777,-0.428616292379385,
1.8));
#22359=CARTESIAN_POINT('Ctrl Pts',(-7.53477770122808,-0.437069791332064,
1.8));
#22360=CARTESIAN_POINT('Ctrl Pts',(-7.53946374370851,-0.445464327647487,
1.8));
#22361=CARTESIAN_POINT('Ctrl Pts',(-7.5442575312461,-0.453785376671825,
1.8));
#22362=CARTESIAN_POINT('Ctrl Pts',(-7.54579335776759,-0.456451261982339,
1.8));
#22363=CARTESIAN_POINT('Ctrl Pts',(-7.54734041244253,-0.459109920914666,
1.8));
#22364=CARTESIAN_POINT('Ctrl Pts',(-7.54889865802203,-0.46176126431195,
1.8));
#22365=CARTESIAN_POINT('Ctrl Pts',(-7.57089648080573,-0.499190398050156,
1.8));
#22366=CARTESIAN_POINT('Ctrl Pts',(-7.59512201376794,-0.535163961610055,
1.8));
#22367=CARTESIAN_POINT('Ctrl Pts',(-7.62143687104016,-0.569509970333361,
1.8));
#22368=CARTESIAN_POINT('Ctrl Pts',(-7.64356266939663,-0.598388442122134,
1.8));
#22369=CARTESIAN_POINT('Ctrl Pts',(-7.66716630710452,-0.626116038796084,
1.8));
#22370=CARTESIAN_POINT('Ctrl Pts',(-7.69217958561781,-0.652572448486006,
1.8));
#22371=CARTESIAN_POINT('Ctrl Pts',(-7.69935390340502,-0.660160685690626,
1.8));
#22372=CARTESIAN_POINT('Ctrl Pts',(-7.70664357687587,-0.667643328511889,
1.8));
#22373=CARTESIAN_POINT('Ctrl Pts',(-7.71403777996775,-0.675008595727681,
1.8));
#22374=CARTESIAN_POINT('Ctrl Pts',(-7.74554705316012,-0.706394563079876,
1.8));
#22375=CARTESIAN_POINT('Ctrl Pts',(-7.77899495328555,-0.735698182477585,
1.8));
#22376=CARTESIAN_POINT('Ctrl Pts',(-7.81424354574822,-0.762712471628142,
1.8));
#22377=CARTESIAN_POINT('Ctrl Pts',(-7.8447822258534,-0.786117114962801,
1.8));
#22378=CARTESIAN_POINT('Ctrl Pts',(-7.87667330535679,-0.807803020240834,
1.8));
#22379=CARTESIAN_POINT('Ctrl Pts',(-7.90984029786111,-0.827606761449139,
1.8));
#22380=CARTESIAN_POINT('Origin',(-8.5,0.,1.8));
#22381=CARTESIAN_POINT('Origin',(-8.5,0.,1.2));
#22382=CARTESIAN_POINT('',(-12.3,-4.65365783675994E-16,1.2));
#22383=CARTESIAN_POINT('',(-12.3,-4.65365783675994E-16,1.2));
#22384=CARTESIAN_POINT('Origin',(-8.5,0.,1.2));
#22385=CARTESIAN_POINT('Origin',(-8.5,0.,1.2));
#22386=CARTESIAN_POINT('Ctrl Pts',(-8.9378559242407,0.917335061595449,1.70084009126667));
#22387=CARTESIAN_POINT('Ctrl Pts',(-9.09066677941173,0.844396458214744,
1.70879376184248));
#22388=CARTESIAN_POINT('Ctrl Pts',(-9.35678627449763,0.62069223278216,1.7247011029941));
#22389=CARTESIAN_POINT('Ctrl Pts',(-9.62072521198725,-0.0294746800758685,
1.75651578529734));
#22390=CARTESIAN_POINT('Ctrl Pts',(-9.27358190662816,-0.920473928894871,
1.79628413817639));
#22391=CARTESIAN_POINT('Ctrl Pts',(-8.14062118033065,-1.14844262332258,
1.84400616163126));
#22392=CARTESIAN_POINT('Ctrl Pts',(-7.47631525146516,-0.457174338716646,
1.88377451451031));
#22393=CARTESIAN_POINT('Ctrl Pts',(-7.47121748055022,0.241452561832278,
1.91558919681355));
#22394=CARTESIAN_POINT('Ctrl Pts',(-7.78668186971636,0.865450294731047,
1.94740387911679));
#22395=CARTESIAN_POINT('Ctrl Pts',(-8.6897509574811,1.18756791113319,1.98717223199585));
#22396=CARTESIAN_POINT('Ctrl Pts',(-9.60167357547127,0.481303778812772,
2.0348942554507));
#22397=CARTESIAN_POINT('Ctrl Pts',(-9.50100253463832,-0.665768137047856,
2.08261627890557));
#22398=CARTESIAN_POINT('Ctrl Pts',(-8.48010907733479,-1.20251427821691,
2.13033830236043));
#22399=CARTESIAN_POINT('Ctrl Pts',(-7.64681002815554,-0.727926671585552,
2.17010665523948));
#22400=CARTESIAN_POINT('Ctrl Pts',(-7.44498060597373,-0.0587522064326047,
2.20192133754272));
#22401=CARTESIAN_POINT('Ctrl Pts',(-7.57134386518546,0.628757665817628,
2.23373601984597));
#22402=CARTESIAN_POINT('Ctrl Pts',(-8.34654981722532,1.19279547618219,2.27350437272501));
#22403=CARTESIAN_POINT('Ctrl Pts',(-9.42125191187756,0.77290076245968,2.32122639617988));
#22404=CARTESIAN_POINT('Ctrl Pts',(-9.64765465886824,-0.356262373710212,
2.36894841963474));
#22405=CARTESIAN_POINT('Ctrl Pts',(-8.8216302613637,-1.1587255804458,2.41667044308961));
#22406=CARTESIAN_POINT('Ctrl Pts',(-7.69804845902684,-0.896211681489087,
2.46439246654446));
#22407=CARTESIAN_POINT('Ctrl Pts',(-7.3785660134251,0.00764272958311676,
2.50416081942352));
#22408=CARTESIAN_POINT('Ctrl Pts',(-7.66367275817319,0.645880124738109,
2.53597550172676));
#22409=CARTESIAN_POINT('Ctrl Pts',(-8.2091023256041,1.0830742068233,2.56779018403));
#22410=CARTESIAN_POINT('Ctrl Pts',(-9.16436302069646,1.00246964476821,2.60755853690905));
#22411=CARTESIAN_POINT('Ctrl Pts',(-9.70239789912868,-0.0182544462211632,
2.65528056036392));
#22412=CARTESIAN_POINT('Ctrl Pts',(-9.1348198302806,-1.02030689992064,2.70300258381878));
#22413=CARTESIAN_POINT('Ctrl Pts',(-7.98510578295691,-1.08672813752691,
2.75072460727364));
#22414=CARTESIAN_POINT('Ctrl Pts',(-7.30714813663279,-0.153061774256481,
2.7984466307285));
#22415=CARTESIAN_POINT('Ctrl Pts',(-7.65691273858533,0.739509857623706,
2.83821498360756));
#22416=CARTESIAN_POINT('Ctrl Pts',(-8.29011032190256,1.03564052975431,2.87002966591079));
#22417=CARTESIAN_POINT('Ctrl Pts',(-8.98864043310205,1.00940649664784,2.90184434821404));
#22418=CARTESIAN_POINT('Ctrl Pts',(-9.65832142754127,0.323442379935309,
2.94161270109309));
#22419=CARTESIAN_POINT('Ctrl Pts',(-9.39737394317918,-0.800508647597189,
2.98933472454795));
#22420=CARTESIAN_POINT('Ctrl Pts',(-8.31251927971242,-1.18695969033239,
3.03705674800282));
#22421=CARTESIAN_POINT('Ctrl Pts',(-7.39958622938631,-0.484957341940189,
3.08477877145768));
#22422=CARTESIAN_POINT('Ctrl Pts',(-7.49775671720164,0.664704372277363,
3.13250079491254));
#22423=CARTESIAN_POINT('Ctrl Pts',(-8.3462581788356,1.11087101034135,3.17226914779159));
#22424=CARTESIAN_POINT('Ctrl Pts',(-9.01886800794062,0.920532984821174,
3.20408383009483));
#22425=CARTESIAN_POINT('Ctrl Pts',(-9.52996935124643,0.443659874939959,
3.23589851239807));
#22426=CARTESIAN_POINT('Ctrl Pts',(-9.58760595877808,-0.513260926890344,
3.27566686527713));
#22427=CARTESIAN_POINT('Ctrl Pts',(-8.65488608504732,-1.19252018450271,
3.32338888873198));
#22428=CARTESIAN_POINT('Ctrl Pts',(-7.58161436923836,-0.774977522330395,
3.37111091218686));
#22429=CARTESIAN_POINT('Ctrl Pts',(-7.35051106244356,0.353226941538064,
3.41883293564171));
#22430=CARTESIAN_POINT('Ctrl Pts',(-8.17695225324716,1.15843154909689,3.46655495909658));
#22431=CARTESIAN_POINT('Ctrl Pts',(-9.11055173066928,0.9406899241179,3.50632331197563));
#22432=CARTESIAN_POINT('Ctrl Pts',(-9.49468098809675,0.356671722621264,
3.53813799427887));
#22433=CARTESIAN_POINT('Ctrl Pts',(-9.56919504916044,-0.338367989045958,
3.56995267658211));
#22434=CARTESIAN_POINT('Ctrl Pts',(-8.98668980890861,-1.0997529406782,3.60972102946116));
#22435=CARTESIAN_POINT('Ctrl Pts',(-7.8368922886023,-1.00318605097734,3.65744305291603));
#22436=CARTESIAN_POINT('Ctrl Pts',(-7.29841635493286,0.01480104106276,3.70516507637089));
#22437=CARTESIAN_POINT('Ctrl Pts',(-7.86180411857744,1.01921543685616,3.75288709982575));
#22438=CARTESIAN_POINT('Ctrl Pts',(-9.01363142052853,1.08743103894989,3.80060912328061));
#22439=CARTESIAN_POINT('Ctrl Pts',(-9.57720536848709,0.311928747092948,
3.84037747615966));
#22440=CARTESIAN_POINT('Ctrl Pts',(-9.48559359232736,-0.381064635674599,
3.87219215846291));
#22441=CARTESIAN_POINT('Ctrl Pts',(-9.08719526120723,-0.955443705498223,
3.90400684076614));
#22442=CARTESIAN_POINT('Ctrl Pts',(-8.14851560934884,-1.15012269943444,
3.9437751936452));
#22443=CARTESIAN_POINT('Ctrl Pts',(-7.34215909770885,-0.324805379838734,
3.99149721710006));
#22444=CARTESIAN_POINT('Ctrl Pts',(-7.60098238778599,0.797364195232309,
4.03921924055492));
#22445=CARTESIAN_POINT('Ctrl Pts',(-8.68421342859387,1.18834317539854,4.08694126400978));
#22446=CARTESIAN_POINT('Ctrl Pts',(-9.59991868137022,0.486315119031409,
4.13466328746464));
#22447=CARTESIAN_POINT('Ctrl Pts',(-9.51872854297443,-0.468895622595936,
4.1744316403437));
#22448=CARTESIAN_POINT('Ctrl Pts',(-8.99603586570454,-0.933034514759925,
4.20624632264694));
#22449=CARTESIAN_POINT('Ctrl Pts',(-8.31894168302622,-1.10674696069834,
4.23806100495018));
#22450=CARTESIAN_POINT('Ctrl Pts',(-7.48168771599556,-0.639815280273472,
4.27782935782924));
#22451=CARTESIAN_POINT('Ctrl Pts',(-7.41186565736802,0.511915756912677,
4.32555138128409));
#22452=CARTESIAN_POINT('Ctrl Pts',(-8.34181353614544,1.19121759958566,4.37327340473896));
#22453=CARTESIAN_POINT('Ctrl Pts',(-9.41681991554689,0.778161507816451,
4.42099542819382));
#22454=CARTESIAN_POINT('Ctrl Pts',(-9.65000288969214,-0.351876191757177,
4.46871745164868));
#22455=CARTESIAN_POINT('Ctrl Pts',(-8.96362831821964,-1.02113649024273,
4.50848580452775));
#22456=CARTESIAN_POINT('Ctrl Pts',(-8.26466394876474,-1.03015626425681,
4.54030048683097));
#22457=CARTESIAN_POINT('Ctrl Pts',(-7.63895283194712,-0.718518422553337,
4.57211516913423));
#22458=CARTESIAN_POINT('Ctrl Pts',(-7.3112802984009,0.182397838956236,4.61188352201326));
#22459=CARTESIAN_POINT('Ctrl Pts',(-8.01203048267288,1.09908136184276,4.65960554546814));
#22460=CARTESIAN_POINT('Ctrl Pts',(-9.15975953510499,1.0043603351126,4.70732756892299));
#22461=CARTESIAN_POINT('Ctrl Pts',(-9.70248278234539,-0.0113687269931911,
4.75504959237786));
#22462=CARTESIAN_POINT('Ctrl Pts',(-9.13946832655052,-1.01853019590215,
4.80277161583271));
#22463=CARTESIAN_POINT('Ctrl Pts',(-8.18251236732564,-1.0755801003455,4.84253996871177));
#22464=CARTESIAN_POINT('Ctrl Pts',(-7.64801679391654,-0.625083676278862,
4.87435465101502));
#22465=CARTESIAN_POINT('Ctrl Pts',(-7.37871875701052,0.0199830748479729,
4.90616933331825));
#22466=CARTESIAN_POINT('Ctrl Pts',(-7.72036584095294,0.915693223013455,
4.94593768619731));
#22467=CARTESIAN_POINT('Ctrl Pts',(-8.85007720703,1.15045210196194,4.99365970965217));
#22468=CARTESIAN_POINT('Ctrl Pts',(-9.65607714221684,0.327884077309669,
5.04138173310702));
#22469=CARTESIAN_POINT('Ctrl Pts',(-9.40194327853509,-0.795356782894278,
5.0891037565619));
#22470=CARTESIAN_POINT('Ctrl Pts',(-8.31719720097595,-1.18865749368552,
5.13682578001674));
#22471=CARTESIAN_POINT('Ctrl Pts',(-7.55616952889954,-0.605685554543534,
5.17659413289581));
#22472=CARTESIAN_POINT('Ctrl Pts',(-7.44670579394524,0.0847130526542142,
5.20840881519905));
#22473=CARTESIAN_POINT('Ctrl Pts',(-7.66510184151263,0.748742955970089,
5.2402234975023));
#22474=CARTESIAN_POINT('Ctrl Pts',(-8.50951785842748,1.20259424204374,5.27999185038134));
#22475=CARTESIAN_POINT('Ctrl Pts',(-9.51746361785082,0.64098508261933,5.32771387383621));
#22476=CARTESIAN_POINT('Ctrl Pts',(-9.58881482009894,-0.508433490677276,
5.37543589729106));
#22477=CARTESIAN_POINT('Ctrl Pts',(-8.6617124163166,-1.19161368916257,5.42315792074593));
#22478=CARTESIAN_POINT('Ctrl Pts',(-7.58404122591754,-0.779322157266933,
5.47087994420079));
#22479=CARTESIAN_POINT('Ctrl Pts',(-7.38993777708112,0.159476676692078,
5.51064829707985));
#22480=CARTESIAN_POINT('Ctrl Pts',(-7.75886872441434,0.753212731004544,
5.54246297938308));
#22481=CARTESIAN_POINT('Ctrl Pts',(-8.35849223365174,1.1124956185188,5.57427766168633));
#22482=CARTESIAN_POINT('Ctrl Pts',(-9.29402998312747,0.903238554602481,
5.61404601456538));
#22483=CARTESIAN_POINT('Ctrl Pts',(-9.68884327202681,-0.180957907666868,
5.66176803802024));
#22484=CARTESIAN_POINT('Ctrl Pts',(-8.99076250408938,-1.09689310850663,
5.7094900614751));
#22485=CARTESIAN_POINT('Ctrl Pts',(-7.84264782508884,-1.00696683556617,
5.75721208492997));
#22486=CARTESIAN_POINT('Ctrl Pts',(-7.29740907026871,0.00992755527834371,
5.80493410838482));
#22487=CARTESIAN_POINT('Ctrl Pts',(-7.76485398692337,0.84689508713768,5.84470246126389));
#22488=CARTESIAN_POINT('Ctrl Pts',(-8.43232822981923,1.05452620513629,5.87651714356711));
#22489=CARTESIAN_POINT('Ctrl Pts',(-9.12086672212119,0.933914055212202,
5.90833182587037));
#22490=CARTESIAN_POINT('Ctrl Pts',(-9.6914577642696,0.163560070272183,5.94810017874941));
#22491=CARTESIAN_POINT('Ctrl Pts',(-9.28066972629324,-0.914685119721433,
5.99582220220428));
#22492=CARTESIAN_POINT('Ctrl Pts',(-8.15346672652938,-1.15062462049409,
6.04354422565913));
#22493=CARTESIAN_POINT('Ctrl Pts',(-7.34403805360179,-0.331430336978762,
6.091266249114));
#22494=CARTESIAN_POINT('Ctrl Pts',(-7.59703200636107,0.794337650555134,
6.13898827256886));
#22495=CARTESIAN_POINT('Ctrl Pts',(-8.49814899597688,1.12145776690186,6.17875662544791));
#22496=CARTESIAN_POINT('Ctrl Pts',(-9.1387772737736,0.841765157457189,6.21057130775116));
#22497=CARTESIAN_POINT('Ctrl Pts',(-9.58057280678224,0.300055592187788,
6.2423859900544));
#22498=CARTESIAN_POINT('Ctrl Pts',(-9.50805779789687,-0.655852862100263,
6.28215434293345));
#22499=CARTESIAN_POINT('Ctrl Pts',(-8.49192487348196,-1.20250941040904,
6.32987636638831));
#22500=CARTESIAN_POINT('Ctrl Pts',(-7.48510361843104,-0.643434271381045,
6.37759838984317));
#22501=CARTESIAN_POINT('Ctrl Pts',(-7.4089520541479,0.505676249830352,6.42532041329804));
#22502=CARTESIAN_POINT('Ctrl Pts',(-8.33684584266954,1.19151341644632,6.4730424367529));
#22503=CARTESIAN_POINT('Ctrl Pts',(-9.23234635719901,0.849317232992327,
6.51281078963195));
#22504=CARTESIAN_POINT('Ctrl Pts',(-9.53382663893441,0.218649185747603,
6.5446254719352));
#22505=CARTESIAN_POINT('Ctrl Pts',(-9.51350682430763,-0.48007797933493,
6.57644015423843));
#22506=CARTESIAN_POINT('Ctrl Pts',(-8.83323634964205,-1.15554187977027,
6.61620850711749));
#22507=CARTESIAN_POINT('Ctrl Pts',(-7.70711659122067,-0.904118349483649,
6.66393053057235));
#22508=CARTESIAN_POINT('Ctrl Pts',(-7.31149575633931,0.17742601193168,6.71165255402721));
#22509=CARTESIAN_POINT('Ctrl Pts',(-8.00574468256001,1.09626902308369,6.75937457748207));
#22510=CARTESIAN_POINT('Ctrl Pts',(-9.15619624715678,1.00783430475606,6.80709660093694));
#22511=CARTESIAN_POINT('Ctrl Pts',(-9.60952973285748,0.163140188382897,
6.84686495381599));
#22512=CARTESIAN_POINT('Ctrl Pts',(-9.42489238334033,-0.511056811947154,
6.87867963611922));
#22513=CARTESIAN_POINT('Ctrl Pts',(-8.95236299576311,-1.02617672416823,
6.91049431842248));
#22514=CARTESIAN_POINT('Ctrl Pts',(-7.99596439398607,-1.09191190509855,
6.95026267130151));
#22515=CARTESIAN_POINT('Ctrl Pts',(-7.30883370513701,-0.164975597507443,
6.99798469475639));
#22516=CARTESIAN_POINT('Ctrl Pts',(-7.71727582008019,0.911792292728067,
7.04570671821124));
#22517=CARTESIAN_POINT('Ctrl Pts',(-8.84348349583492,1.15243792799422,7.09342874166611));
#22518=CARTESIAN_POINT('Ctrl Pts',(-9.65565533900699,0.332842662605653,
7.14115076512097));
#22519=CARTESIAN_POINT('Ctrl Pts',(-9.44582473222385,-0.602566614636137,
7.18091911800003));
#22520=CARTESIAN_POINT('Ctrl Pts',(-8.86507923315232,-0.991626007786943,
7.21273380030326));
#22521=CARTESIAN_POINT('Ctrl Pts',(-8.17069521096301,-1.07202113089142,
7.24454848260651));
#22522=CARTESIAN_POINT('Ctrl Pts',(-7.40440644892101,-0.495982128165813,
7.28431683548555));
#22523=CARTESIAN_POINT('Ctrl Pts',(-7.49123647716817,0.654591662637485,
7.33203885894042));
#22524=CARTESIAN_POINT('Ctrl Pts',(-8.50462872339795,1.20166588610525,7.37976088239528));
#22525=CARTESIAN_POINT('Ctrl Pts',(-9.51377638599174,0.646800996440254,
7.42748290585015));
#22526=CARTESIAN_POINT('Ctrl Pts',(-9.59174012789106,-0.5044075671302,7.475204929305));
#22527=CARTESIAN_POINT('Ctrl Pts',(-8.82103645592899,-1.07452619471326,
7.51497328218406));
#22528=CARTESIAN_POINT('Ctrl Pts',(-8.12729238132298,-0.98878411029843,
7.5467879644873));
#22529=CARTESIAN_POINT('Ctrl Pts',(-7.54956132387895,-0.595262355683333,
7.57860264679055));
#22530=CARTESIAN_POINT('Ctrl Pts',(-7.34694308408231,0.341735642390682,
7.61837099966959));
#22531=CARTESIAN_POINT('Ctrl Pts',(-8.16540476730042,1.15504983444235,7.66609302312446));
#22532=CARTESIAN_POINT('Ctrl Pts',(-9.28972515479892,0.905735340365632,
7.71381504657931));
#22533=CARTESIAN_POINT('Ctrl Pts',(-9.68986002054785,-0.174147125421056,
7.76153707003418));
#22534=CARTESIAN_POINT('Ctrl Pts',(-8.99560885476197,-1.09576245770118,
7.80925909348904));
#22535=CARTESIAN_POINT('Ctrl Pts',(-8.03974503939758,-1.02266139088228,
7.84902744636809));
#22536=CARTESIAN_POINT('Ctrl Pts',(-7.57119801841753,-0.503916525633981,
7.88084212867134));
#22537=CARTESIAN_POINT('Ctrl Pts',(-7.39175997946444,0.17168286473535,7.91265681097457));
#22538=CARTESIAN_POINT('Ctrl Pts',(-7.85158730821006,1.01285955677552,7.95242516385363));
#22539=CARTESIAN_POINT('Ctrl Pts',(-9.00268601129995,1.09242888273514,8.00014718730849));
#22540=CARTESIAN_POINT('Ctrl Pts',(-9.68983581786349,0.168264831258786,
8.04786921076336));
#22541=CARTESIAN_POINT('Ctrl Pts',(-9.28589479704269,-0.91019968016463,
8.09559123421821));
#22542=CARTESIAN_POINT('Ctrl Pts',(-8.15787155631456,-1.15294042718917,
8.14331325767308));
#22543=CARTESIAN_POINT('Ctrl Pts',(-7.48282485956976,-0.472255950572485,
8.18308161055214));
#22544=CARTESIAN_POINT('Ctrl Pts',(-7.4678884532851,0.226607018726978,8.21489629285537));
#22545=CARTESIAN_POINT('Ctrl Pts',(-7.77421828515018,0.854933828755218,
8.24671097515861));
#22546=CARTESIAN_POINT('Ctrl Pts',(-8.67232841342475,1.19022116371383,8.28647932803768));
#22547=CARTESIAN_POINT('Ctrl Pts',(-9.59491116316883,0.497256105602345,
8.33420135149252));
#22548=CARTESIAN_POINT('Ctrl Pts',(-9.5099094215147,-0.651233665626483,
8.3819233749474));
#22549=CARTESIAN_POINT('Ctrl Pts',(-8.49881107916957,-1.202535935537,8.42964539840226));
#22550=CARTESIAN_POINT('Ctrl Pts',(-7.48691960206137,-0.648067595192266,
8.4773674218571));
#22551=CARTESIAN_POINT('Ctrl Pts',(-7.42177080556001,0.30837112935176,8.51713577473619));
#22552=CARTESIAN_POINT('Ctrl Pts',(-7.86772641284064,0.846661146373908,
8.54895045703939));
#22553=CARTESIAN_POINT('Ctrl Pts',(-8.51049035685063,1.12141022894102,8.58076513934267));
#22554=CARTESIAN_POINT('Ctrl Pts',(-9.40906056154167,0.787357857695821,
8.62053349222169));
#22555=CARTESIAN_POINT('Ctrl Pts',(-9.65337439438576,-0.340325720693924,
8.66825551567658));
#22556=CARTESIAN_POINT('Ctrl Pts',(-8.83765888906691,-1.15326007541383,
8.71597753913143));
#22557=CARTESIAN_POINT('Ctrl Pts',(-7.71230695230558,-0.908643908472651,
8.76369956258628));
#22558=CARTESIAN_POINT('Ctrl Pts',(-7.30983761385512,0.172733885592004,
8.81142158604117));
#22559=CARTESIAN_POINT('Ctrl Pts',(-7.88634632323323,0.938669331634422,
8.85118993892019));
#22560=CARTESIAN_POINT('Ctrl Pts',(-8.57579354715678,1.05397358790813,8.88300462122346));
#22561=CARTESIAN_POINT('Ctrl Pts',(-9.24164844925372,0.841206589893327,
8.91481930352667));
#22562=CARTESIAN_POINT('Ctrl Pts',(-9.70263172305109,0.000662824957779389,
8.95458765640575));
#22563=CARTESIAN_POINT('Ctrl Pts',(-9.14957526799147,-1.01200101828229,
9.00230967986059));
#22564=CARTESIAN_POINT('Ctrl Pts',(-8.00080189061878,-1.09307985732958,
9.05003170331546));
#22565=CARTESIAN_POINT('Ctrl Pts',(-7.30979795505992,-0.171794010404939,
9.09775372677033));
#22566=CARTESIAN_POINT('Ctrl Pts',(-7.71295188493065,0.909328744289747,
9.14547575022519));
#22567=CARTESIAN_POINT('Ctrl Pts',(-8.65007393300695,1.11137246852359,9.18524410310424));
#22568=CARTESIAN_POINT('Ctrl Pts',(-9.246911830585,0.747480904860254,9.21705878540749));
#22569=CARTESIAN_POINT('Ctrl Pts',(-9.61125784799244,0.150920324793055,
9.24887346771071));
#22570=CARTESIAN_POINT('Ctrl Pts',(-9.40992790634683,-0.786355330545322,
9.28864182058978));
#22571=CARTESIAN_POINT('Ctrl Pts',(-8.32911251233276,-1.19033254023796,
9.33636384404463));
#22572=CARTESIAN_POINT('Ctrl Pts',(-7.40730065527932,-0.500030468028132,
9.3840858674995));
#22573=CARTESIAN_POINT('Ctrl Pts',(-7.48750455049532,0.648804326837381,
9.43180789095436));
#22574=CARTESIAN_POINT('Ctrl Pts',(-8.49974688525287,1.20263187907136,9.47952991440923));
#22575=CARTESIAN_POINT('Ctrl Pts',(-9.34064149709282,0.742288907721195,
9.51929826728827));
#22576=CARTESIAN_POINT('Ctrl Pts',(-9.55391555690441,0.0765962447736241,
9.55111294959152));
#22577=CARTESIAN_POINT('Ctrl Pts',(-9.4391364257873,-0.612938596369855,
9.58292763189476));
#22578=CARTESIAN_POINT('Ctrl Pts',(-8.67364027820268,-1.19003048465638,
9.62269598477381));
#22579=CARTESIAN_POINT('Ctrl Pts',(-7.59195627203432,-0.78838485392146,
9.67041800822867));
#22580=CARTESIAN_POINT('Ctrl Pts',(-7.34648309378723,0.336780453694595,
9.71814003168354));
#22581=CARTESIAN_POINT('Ctrl Pts',(-8.1587959535008,1.15311486350804,9.76586205513838));
#22582=CARTESIAN_POINT('Ctrl Pts',(-9.28666527733334,0.909659959580418,
9.81358407859327));
#22583=CARTESIAN_POINT('Ctrl Pts',(-9.62140191411355,0.0113444340048612,
9.85335243147231));
#22584=CARTESIAN_POINT('Ctrl Pts',(-9.34714244837062,-0.63162857595835,
9.88516711377556));
#22585=CARTESIAN_POINT('Ctrl Pts',(-8.80919223289119,-1.07799402237682,
9.91698179607879));
#22586=CARTESIAN_POINT('Ctrl Pts',(-7.85270416759372,-1.01357368058532,
9.95675014895785));
#22587=CARTESIAN_POINT('Ctrl Pts',(-7.29746531872796,-0.00210478704529599,
10.0044721724127));
#22588=CARTESIAN_POINT('Ctrl Pts',(-7.84799736347558,1.00941314082721,10.0521941958676));
#22589=CARTESIAN_POINT('Ctrl Pts',(-8.99642206321121,1.09528956214679,10.0999162193224));
#22590=CARTESIAN_POINT('Ctrl Pts',(-9.69008957102098,0.173234850918763,
10.1476382427773));
#22591=CARTESIAN_POINT('Ctrl Pts',(-9.35548634532394,-0.725130375949533,
10.1874065956563));
#22592=CARTESIAN_POINT('Ctrl Pts',(-8.72739302219708,-1.03193866060664,
10.2192212779596));
#22593=CARTESIAN_POINT('Ctrl Pts',(-8.02851887983101,-1.01753452151983,
10.2510359602628));
#22594=CARTESIAN_POINT('Ctrl Pts',(-7.34732047653931,-0.343006438452994,
10.2908043131419));
#22595=CARTESIAN_POINT('Ctrl Pts',(-7.58920203641245,0.7852013495374,10.3385263365967));
#22596=CARTESIAN_POINT('Ctrl Pts',(-8.66735858846781,1.18996362540016,10.3862483600516));
#22597=CARTESIAN_POINT('Ctrl Pts',(-9.59204571388488,0.503517873144797,
10.4339703835065));
#22598=CARTESIAN_POINT('Ctrl Pts',(-9.51335310231618,-0.647641097099265,
10.4816924069613));
#22599=CARTESIAN_POINT('Ctrl Pts',(-8.67252686454233,-1.10810894327751,
10.5214607598404));
#22600=CARTESIAN_POINT('Ctrl Pts',(-7.99679100783777,-0.929185501396585,
10.5532754421436));
#22601=CARTESIAN_POINT('Ctrl Pts',(-7.47768944170931,-0.461033698950278,
10.5850901244469));
#22602=CARTESIAN_POINT('Ctrl Pts',(-7.40386039813483,0.494774164491896,
10.6248584773259));
#22603=CARTESIAN_POINT('Ctrl Pts',(-8.32494671266358,1.18972704280574,10.6725805007808));
#22604=CARTESIAN_POINT('Ctrl Pts',(-9.40513361302378,0.790414745234386,
10.7203025242356));
#22605=CARTESIAN_POINT('Ctrl Pts',(-9.65530433140282,-0.333715435112715,
10.7680245476905));
#22606=CARTESIAN_POINT('Ctrl Pts',(-8.84261372599144,-1.15279631131785,
10.8157465711454));
#22607=CARTESIAN_POINT('Ctrl Pts',(-7.90546168306107,-0.950891759798041,
10.8555149240244));
#22608=CARTESIAN_POINT('Ctrl Pts',(-7.51150003530626,-0.373460581051111,
10.8873296063277));
#22609=CARTESIAN_POINT('Ctrl Pts',(-7.42522961150793,0.320217990095783,
10.9191442886309));
#22610=CARTESIAN_POINT('Ctrl Pts',(-7.99476109608862,1.09135564808188,10.95891264151));
#22611=CARTESIAN_POINT('Ctrl Pts',(-9.14602870394829,1.01426870377897,11.0066346649648));
#22612=CARTESIAN_POINT('Ctrl Pts',(-9.70166201229556,0.0055439259745542,
11.0543566884197));
#22613=CARTESIAN_POINT('Ctrl Pts',(-9.15535975983058,-1.00826468498374,
11.1020787118745));
#22614=CARTESIAN_POINT('Ctrl Pts',(-8.00485243357111,-1.09597097958172,
11.1498007353294));
#22615=CARTESIAN_POINT('Ctrl Pts',(-7.42822998271092,-0.330121158365471,
11.1895690882084));
#22616=CARTESIAN_POINT('Ctrl Pts',(-7.50809623085543,0.364323892375102,
11.2213837705117));
#22617=CARTESIAN_POINT('Ctrl Pts',(-7.89671320806008,0.945365535563497,
11.2531984528149));
#22618=CARTESIAN_POINT('Ctrl Pts',(-8.83196240436717,1.15590850101232,11.292966805694));
#22619=CARTESIAN_POINT('Ctrl Pts',(-9.65217599238663,0.34436110749974,11.3406888291488));
#22620=CARTESIAN_POINT('Ctrl Pts',(-9.41238816090703,-0.782029520380217,
11.3884108526037));
#22621=CARTESIAN_POINT('Ctrl Pts',(-8.33593165763767,-1.19129159689182,
11.4361328760586));
#22622=CARTESIAN_POINT('Ctrl Pts',(-7.40847229147015,-0.504867073730658,
11.4838548995134));
#22623=CARTESIAN_POINT('Ctrl Pts',(-7.47347904807857,0.451581315409203,
11.5236232523925));
#22624=CARTESIAN_POINT('Ctrl Pts',(-7.9882389265501,0.924502887772644,11.5554379346957));
#22625=CARTESIAN_POINT('Ctrl Pts',(-8.662295109207,1.10965366069233,11.587252616999));
#22626=CARTESIAN_POINT('Ctrl Pts',(-9.50733424510565,0.6569636361803,11.627020969878));
#22627=CARTESIAN_POINT('Ctrl Pts',(-9.59664513622963,-0.493420241755894,
11.6747429933329));
#22628=CARTESIAN_POINT('Ctrl Pts',(-8.67833114031927,-1.18836876907038,
11.7224650167878));
#22629=CARTESIAN_POINT('Ctrl Pts',(-7.59648578275535,-0.793571766778151,
11.7701870402426));
#22630=CARTESIAN_POINT('Ctrl Pts',(-7.34420465835447,0.332356177701384,
11.8179090636975));
#22631=CARTESIAN_POINT('Ctrl Pts',(-8.01915026029997,1.01314089690961,11.8576774165765));
#22632=CARTESIAN_POINT('Ctrl Pts',(-8.71786174690529,1.03399286507883,11.8894920988798));
#22633=CARTESIAN_POINT('Ctrl Pts',(-9.34875922243034,0.732992995532587,
11.921306781183));
#22634=CARTESIAN_POINT('Ctrl Pts',(-9.6916373311426,-0.162246638341423,
11.9610751340621));
#22635=CARTESIAN_POINT('Ctrl Pts',(-9.00650705906901,-1.09066249999891,
12.0087971575169));
#22636=CARTESIAN_POINT('Ctrl Pts',(-7.85733887313724,-1.01538613489102,
12.0565191809718));
#22637=CARTESIAN_POINT('Ctrl Pts',(-7.29749708846947,-0.0089909705338671,
12.1042412044266));
#22638=CARTESIAN_POINT('Ctrl Pts',(-7.84337957856142,1.00755799970802,12.1519632278815));
#22639=CARTESIAN_POINT('Ctrl Pts',(-8.79923252726346,1.08080101951651,12.1917315807606));
#22640=CARTESIAN_POINT('Ctrl Pts',(-9.34127841248145,0.639418187488609,
12.2235462630638));
#22641=CARTESIAN_POINT('Ctrl Pts',(-9.62145885139695,-0.000996887084038987,
12.2553609453671));
#22642=CARTESIAN_POINT('Ctrl Pts',(-9.29502513200662,-0.902362754164655,
12.2951292982461));
#22643=CARTESIAN_POINT('Ctrl Pts',(-8.1694501543662,-1.15621403266957,12.342851321701));
#22644=CARTESIAN_POINT('Ctrl Pts',(-7.34963963733674,-0.347409503213033,
12.3905733451558));
#22645=CARTESIAN_POINT('Ctrl Pts',(-7.58472057763644,0.779972864135922,
12.4382953686107));
#22646=CARTESIAN_POINT('Ctrl Pts',(-8.66265259355083,1.19158198813047,12.4860173920655));
#22647=CARTESIAN_POINT('Ctrl Pts',(-9.43344092441323,0.621577822795351,
12.5257857449446));
#22648=CARTESIAN_POINT('Ctrl Pts',(-9.55457743897031,-0.0668686100748459,
12.5576004272478));
#22649=CARTESIAN_POINT('Ctrl Pts',(-9.34745473800569,-0.73450079386759,
12.5894151095511));
#22650=CARTESIAN_POINT('Ctrl Pts',(-8.51084346084306,-1.20258301999602,
12.6291834624301));
#22651=CARTESIAN_POINT('Ctrl Pts',(-7.49353410420185,-0.658118902923919,
12.676905485885));
#22652=CARTESIAN_POINT('Ctrl Pts',(-7.40273343869918,0.489926954106946,
12.7246275093399));
#22653=CARTESIAN_POINT('Ctrl Pts',(-8.31813670676161,1.18870510740178,12.7723495327947));
#22654=CARTESIAN_POINT('Ctrl Pts',(-9.40263354937312,0.794717670730844,
12.8200715562496));
#22655=CARTESIAN_POINT('Ctrl Pts',(-9.61260306996757,-0.140660434590392,
12.8598399091286));
#22656=CARTESIAN_POINT('Ctrl Pts',(-9.25377696749447,-0.740557404306628,
12.8916545914319));
#22657=CARTESIAN_POINT('Ctrl Pts',(-8.66032206785154,-1.10994044151937,
12.9234692737351));
#22658=CARTESIAN_POINT('Ctrl Pts',(-7.7213756745308,-0.916552050029583,
12.9632376266142));
#22659=CARTESIAN_POINT('Ctrl Pts',(-7.30826349421839,0.160804821376725,
13.010959650069));
#22660=CARTESIAN_POINT('Ctrl Pts',(-7.99073740166053,1.08842727494398,13.0586816735239));
#22661=CARTESIAN_POINT('Ctrl Pts',(-9.1402099835718,1.0179515050952,13.1064036969788));
#22662=CARTESIAN_POINT('Ctrl Pts',(-9.70258664433777,0.010433766633717,
13.1541257204336));
#22663=CARTESIAN_POINT('Ctrl Pts',(-9.24937860779893,-0.83432766425052,
13.1938940733127));
#22664=CARTESIAN_POINT('Ctrl Pts',(-8.58551523025838,-1.05322938204002,
13.2257087556159));
#22665=CARTESIAN_POINT('Ctrl Pts',(-7.89503345433145,-0.944291495133931,
13.2575234379192));
#22666=CARTESIAN_POINT('Ctrl Pts',(-7.31148207597819,-0.183708042569379,
13.2972917907982));
#22667=CARTESIAN_POINT('Ctrl Pts',(-7.70395651638576,0.901337263173938,
13.3450138142531));
#22668=CARTESIAN_POINT('Ctrl Pts',(-8.82700349925863,1.15632652757863,13.3927358377079));
#22669=CARTESIAN_POINT('Ctrl Pts',(-9.65018514507657,0.350953304352284,
13.4404578611628));
#22670=CARTESIAN_POINT('Ctrl Pts',(-9.41628673666211,-0.77893652940587,
13.4881798846177));
#22671=CARTESIAN_POINT('Ctrl Pts',(-8.52083705101177,-1.12126569842545,
13.5279482374967));
#22672=CARTESIAN_POINT('Ctrl Pts',(-7.87556538618484,-0.852459030609716,
13.5597629197999));
#22673=CARTESIAN_POINT('Ctrl Pts',(-7.42466201419345,-0.318306715986269,
13.5915776021032));
#22674=CARTESIAN_POINT('Ctrl Pts',(-7.48098307234338,0.638692415623545,
13.6313459549823));
#22675=CARTESIAN_POINT('Ctrl Pts',(-8.48771545022648,1.2024737750269,13.6790679784371));
#22676=CARTESIAN_POINT('Ctrl Pts',(-9.5038575626246,0.660524277275879,13.726790001892));
#22677=CARTESIAN_POINT('Ctrl Pts',(-9.59945268682829,-0.487132301553321,
13.7745120253468));
#22678=CARTESIAN_POINT('Ctrl Pts',(-8.68330312999737,-1.18858044034005,
13.8222340488017));
#22679=CARTESIAN_POINT('Ctrl Pts',(-7.78213757023688,-0.861594151033408,
13.8620024016807));
#22680=CARTESIAN_POINT('Ctrl Pts',(-7.47002326942581,-0.236120563005943,
13.893817083984));
#22681=CARTESIAN_POINT('Ctrl Pts',(-7.47851070073035,0.462850473304309,
13.9256317662872));
#22682=CARTESIAN_POINT('Ctrl Pts',(-8.14724805356803,1.14973456280755,13.9654001191663));
#22683=CARTESIAN_POINT('Ctrl Pts',(-9.27746302049914,0.917412307278985,
14.0131221426211));
#22684=CARTESIAN_POINT('Ctrl Pts',(-9.69133773090962,-0.157279171604172,
14.060844166076));
#22685=CARTESIAN_POINT('Ctrl Pts',(-9.01274434530469,-1.08774414553638,
14.1085661895309));
#22686=CARTESIAN_POINT('Ctrl Pts',(-7.86096046478965,-1.01879928006645,
14.1562882129857));
#22687=CARTESIAN_POINT('Ctrl Pts',(-7.39339125658958,-0.181901176928426,
14.1960565658648));
#22688=CARTESIAN_POINT('Ctrl Pts',(-7.56658796866361,0.495325110967661,
14.227871248168));
#22689=CARTESIAN_POINT('Ctrl Pts',(-8.03032863686894,1.01837113068607,14.2596859304713));
#22690=CARTESIAN_POINT('Ctrl Pts',(-8.98547726602411,1.10028874610241,14.2994542833503));
#22691=CARTESIAN_POINT('Ctrl Pts',(-9.68820253147304,0.185118432341084,
14.3471763068052));
#22692=CARTESIAN_POINT('Ctrl Pts',(-9.29804866714497,-0.898410068830433,
14.3948983302601));
#22693=CARTESIAN_POINT('Ctrl Pts',(-8.17607654062253,-1.15808794236719,
14.4426203537149));
#22694=CARTESIAN_POINT('Ctrl Pts',(-7.35014532908186,-0.352360236686861,
14.4903423771698));
#22695=CARTESIAN_POINT('Ctrl Pts',(-7.54410935628155,0.586467412906594,
14.5301107300488));
#22696=CARTESIAN_POINT('Ctrl Pts',(-8.11818483430833,0.985303082841334,
14.5619254123521));
#22697=CARTESIAN_POINT('Ctrl Pts',(-8.81110824342201,1.07744262493533,14.5937400946553));
#22698=CARTESIAN_POINT('Ctrl Pts',(-9.58703953535871,0.514459472793815,
14.6335084475343));
#22699=CARTESIAN_POINT('Ctrl Pts',(-9.5197011993494,-0.637419449003044,
14.6812304709892));
#22700=CARTESIAN_POINT('Ctrl Pts',(-8.51571617796591,-1.20157202386707,
14.7289524944441));
#22701=CARTESIAN_POINT('Ctrl Pts',(-7.49731927134888,-0.663871558339892,
14.7766745178989));
#22702=CARTESIAN_POINT('Ctrl Pts',(-7.39987670884486,0.485852082205623,
14.8243965413538));
#22703=CARTESIAN_POINT('Ctrl Pts',(-8.16081779720729,1.06893703341116,14.8641648942329));
#22704=CARTESIAN_POINT('Ctrl Pts',(-8.8559140568051,0.994952345727948,14.8959795765361));
#22705=CARTESIAN_POINT('Ctrl Pts',(-9.44022464924591,0.611267993885705,
14.9277942588393));
#22706=CARTESIAN_POINT('Ctrl Pts',(-9.65867724640615,-0.322165374756826,
14.9675626117184));
#22707=CARTESIAN_POINT('Ctrl Pts',(-8.85410231103244,-1.14921958576719,
15.0152846351732));
#22708=CARTESIAN_POINT('Ctrl Pts',(-7.72572214438401,-0.918975590321003,
15.0630066586281));
#22709=CARTESIAN_POINT('Ctrl Pts',(-7.30736222115706,0.153977788901801,
15.110728682083));
#22710=CARTESIAN_POINT('Ctrl Pts',(-7.98591084190305,1.0872147627098,15.1584507055378));
#22711=CARTESIAN_POINT('Ctrl Pts',(-8.9428753883204,1.03030690516172,15.1982190584169));
#22712=CARTESIAN_POINT('Ctrl Pts',(-9.42013743498128,0.519569006187592,
15.2300337407202));
#22713=CARTESIAN_POINT('Ctrl Pts',(-9.61098803899296,-0.152895867268804,
15.2618484230234));
#22714=CARTESIAN_POINT('Ctrl Pts',(-9.1654669503698,-1.00173643888712,15.3016167759024));
#22715=CARTESIAN_POINT('Ctrl Pts',(-8.01588181111314,-1.10078331455882,
15.3493387993573));
#22716=CARTESIAN_POINT('Ctrl Pts',(-7.31318175323431,-0.188383730563224,
15.3970608228122));
#22717=CARTESIAN_POINT('Ctrl Pts',(-7.69881132927115,0.896762228213724,
15.444782846267));
#22718=CARTESIAN_POINT('Ctrl Pts',(-8.82255375228613,1.15857095575389,15.4925048697219));
#22719=CARTESIAN_POINT('Ctrl Pts',(-9.50904512931535,0.489402906826901,
15.5322732226009));
#22720=CARTESIAN_POINT('Ctrl Pts',(-9.53578529193268,-0.209092634933555,
15.5640879049042));
#22721=CARTESIAN_POINT('Ctrl Pts',(-9.2401877616229,-0.842543822232629,
15.5959025872074));
#22722=CARTESIAN_POINT('Ctrl Pts',(-8.34777029430052,-1.19292557033953,
15.6356709400864));
#22723=CARTESIAN_POINT('Ctrl Pts',(-7.41379258935603,-0.515793056893565,
15.6833929635413));
#22724=CARTESIAN_POINT('Ctrl Pts',(-7.47897580231666,0.634172756274122,
15.7311149869962));
#22725=CARTESIAN_POINT('Ctrl Pts',(-8.48126958185156,1.2021390181908,15.7788370104511));
#22726=CARTESIAN_POINT('Ctrl Pts',(-9.50111792497817,0.665597216139478,
15.8265590339059));
#22727=CARTESIAN_POINT('Ctrl Pts',(-9.60129174604384,-0.482092567813502,
15.8742810573608));
#22728=CARTESIAN_POINT('Ctrl Pts',(-8.68981880352144,-1.18720590861504,
15.9220030808156));
#22729=CARTESIAN_POINT('Ctrl Pts',(-7.60428317324231,-0.801471685911831,
15.9697251042705));
#22730=CARTESIAN_POINT('Ctrl Pts',(-7.34085844261802,0.319812236206833,
16.0174471277253));
#22731=CARTESIAN_POINT('Ctrl Pts',(-8.14340243192267,1.1485135933495,16.0651691511802));
#22732=CARTESIAN_POINT('Ctrl Pts',(-9.08302755349385,0.958038040322845,
16.1049375040593));
#22733=CARTESIAN_POINT('Ctrl Pts',(-9.48389821835483,0.385376694788,16.1367521863625));
#22734=CARTESIAN_POINT('Ctrl Pts',(-9.57857408885389,-0.307189213773236,
16.1685668686657));
#22735=CARTESIAN_POINT('Ctrl Pts',(-9.01839426272804,-1.08517048015552,
16.2083352215448));
#22736=CARTESIAN_POINT('Ctrl Pts',(-7.86628709111648,-1.02200475985657,
16.2560572449997));
#22737=CARTESIAN_POINT('Ctrl Pts',(-7.29849140255546,-0.0200766297914018,
16.3037792684545));
#22738=CARTESIAN_POINT('Ctrl Pts',(-7.83249587692306,1.00026625060406,16.3515012919094));
#22739=CARTESIAN_POINT('Ctrl Pts',(-8.98185711668004,1.10187833907993,16.3992233153643));
#22740=CARTESIAN_POINT('Ctrl Pts',(-9.56769966619584,0.343058292158321,
16.4389916682433));
#22741=CARTESIAN_POINT('Ctrl Pts',(-9.49623696904437,-0.352302076283959,
16.4708063505465));
#22742=CARTESIAN_POINT('Ctrl Pts',(-9.11467520479983,-0.938000704161855,
16.5026210328498));
#22743=CARTESIAN_POINT('Ctrl Pts',(-8.18204041706793,-1.15983848287103,
16.5423893857288));
#22744=CARTESIAN_POINT('Ctrl Pts',(-7.35207269505694,-0.358269358953146,
16.5901114091837));
#22745=CARTESIAN_POINT('Ctrl Pts',(-7.57822133797448,0.770938669115475,
16.6378334326386));
#22746=CARTESIAN_POINT('Ctrl Pts',(-8.64964987006652,1.19318859338267,16.6855554560934));
#22747=CARTESIAN_POINT('Ctrl Pts',(-9.58534244846187,0.518030172478724,
16.7332774795483));
#22748=CARTESIAN_POINT('Ctrl Pts',(-9.53190693470597,-0.439134409383287,
16.7730458324274));
#22749=CARTESIAN_POINT('Ctrl Pts',(-9.02290381225217,-0.918246475208663,
16.8048605147306));
#22750=CARTESIAN_POINT('Ctrl Pts',(-8.35113597915327,-1.11153517775485,
16.8366751970339));
#22751=CARTESIAN_POINT('Ctrl Pts',(-7.50068418268081,-0.669097450885376,
16.8764435499128));
#22752=CARTESIAN_POINT('Ctrl Pts',(-7.39746804575687,0.480122254695365,
16.9241655733678));
#22753=CARTESIAN_POINT('Ctrl Pts',(-8.30731076557255,1.18612528247467,16.9718875968226));
#22754=CARTESIAN_POINT('Ctrl Pts',(-9.39385135696734,0.804440079539564,
17.0196096202775));
#22755=CARTESIAN_POINT('Ctrl Pts',(-9.65973006081727,-0.318354655403303,
17.0673316437323));
#22756=CARTESIAN_POINT('Ctrl Pts',(-8.99306665327201,-1.00725181786075,
17.1070999966114));
#22757=CARTESIAN_POINT('Ctrl Pts',(-8.29465842608819,-1.03655189152894,
17.1389146789146));
#22758=CARTESIAN_POINT('Ctrl Pts',(-7.66016704512213,-0.743203577124704,
17.1707293612179));
#22759=CARTESIAN_POINT('Ctrl Pts',(-7.30648773259623,0.147824112332773,
17.2104977140969));
#22760=CARTESIAN_POINT('Ctrl Pts',(-7.9803404223588,1.08445747411188,17.2582197375518));
#22761=CARTESIAN_POINT('Ctrl Pts',(-9.13033490461218,1.02308368911607,17.3059417610066));
#22762=CARTESIAN_POINT('Ctrl Pts',(-9.7023062493245,0.0235323740106206,
17.3536637844615));
#22763=CARTESIAN_POINT('Ctrl Pts',(-9.16875696690466,-0.99954370581896,
17.4013858079164));
#22764=CARTESIAN_POINT('Ctrl Pts',(-8.21385965450184,-1.08434065304146,
17.4411541607954));
#22765=CARTESIAN_POINT('Ctrl Pts',(-7.66651569284325,-0.649545145099307,
17.4729688430987));
#22766=CARTESIAN_POINT('Ctrl Pts',(-7.37861109970015,-0.0125651679117135,
17.5047835254019));
#22767=CARTESIAN_POINT('Ctrl Pts',(-7.69412058637172,0.892682402266311,
17.544551878281));
#22768=CARTESIAN_POINT('Ctrl Pts',(-8.81654339210534,1.16012687698589,17.5922739017358));
#22769=CARTESIAN_POINT('Ctrl Pts',(-9.64607496368117,0.361295591631848,
17.6399959251907));
#22770=CARTESIAN_POINT('Ctrl Pts',(-9.42464482979018,-0.768847207534023,
17.6877179486456));
#22771=CARTESIAN_POINT('Ctrl Pts',(-8.35176929286965,-1.19346183771808,
17.7354399721004));
#22772=CARTESIAN_POINT('Ctrl Pts',(-7.57414417389279,-0.632820621048115,
17.7752083249795));
#22773=CARTESIAN_POINT('Ctrl Pts',(-7.44469102409625,0.0541105458809273,
17.8070230072827));
#22774=CARTESIAN_POINT('Ctrl Pts',(-7.64372479594433,0.724198677214912,
17.8388376895859));
#22775=CARTESIAN_POINT('Ctrl Pts',(-8.47461430237912,1.20236394946876,17.878606042465));
#22776=CARTESIAN_POINT('Ctrl Pts',(-9.49843356039162,0.670242131825755,
17.9263280659198));
#22777=CARTESIAN_POINT('Ctrl Pts',(-9.60311108913075,-0.476621707380359,
17.9740500893747));
#22778=CARTESIAN_POINT('Ctrl Pts',(-8.69622519637391,-1.18641888138153,
18.0217721128296));
#22779=CARTESIAN_POINT('Ctrl Pts',(-7.60704310414848,-0.80557524960553,
18.0694941362844));
#22780=CARTESIAN_POINT('Ctrl Pts',(-7.38577725982833,0.127195261093777,
18.1092624891635));
#22781=CARTESIAN_POINT('Ctrl Pts',(-7.73732247271078,0.731387705096654,
18.1410771714667));
#22782=CARTESIAN_POINT('Ctrl Pts',(-8.3262669675734,1.10792047666078,18.17289185377));
#22783=CARTESIAN_POINT('Ctrl Pts',(-9.26748337738822,0.92590105630058,18.212660206649));
#22784=CARTESIAN_POINT('Ctrl Pts',(-9.69359399866432,-0.146381201467666,
18.2603822301039));
#22785=CARTESIAN_POINT('Ctrl Pts',(-9.02238788447832,-1.0821890893276,18.3081042535587));
#22786=CARTESIAN_POINT('Ctrl Pts',(-7.87214708287262,-1.02561922965847,
18.3558262770137));
#22787=CARTESIAN_POINT('Ctrl Pts',(-7.2976274719566,-0.0249760772001006,
18.4035483004684));
#22788=CARTESIAN_POINT('Ctrl Pts',(-7.740586531955,0.825204298166379,18.4433166533476));
#22789=CARTESIAN_POINT('Ctrl Pts',(-8.40175415087621,1.05211821528215,18.4751313356508));
#22790=CARTESIAN_POINT('Ctrl Pts',(-9.09350283873543,0.951538401523235,
18.506946017954));
#22791=CARTESIAN_POINT('Ctrl Pts',(-9.68620940283924,0.198067547169027,
18.5467143708331));
#22792=CARTESIAN_POINT('Ctrl Pts',(-9.30688528934162,-0.891644671174926,
18.5944363942879));
#22793=CARTESIAN_POINT('Ctrl Pts',(-8.18700405536254,-1.16019647713218,
18.6421584177428));
#22794=CARTESIAN_POINT('Ctrl Pts',(-7.35414309684935,-0.364837014696453,
18.6898804411976));
#22795=CARTESIAN_POINT('Ctrl Pts',(-7.5743604621335,0.767798766972237,18.7376024646525));
#22796=CARTESIAN_POINT('Ctrl Pts',(-8.46560482642789,1.12093172013077,18.7773708175315));
#22797=CARTESIAN_POINT('Ctrl Pts',(-9.11408002803092,0.859948082719013,
18.8091854998348));
#22798=CARTESIAN_POINT('Ctrl Pts',(-9.57141001751387,0.331287674885919,
18.841000182138));
#22799=CARTESIAN_POINT('Ctrl Pts',(-9.52666622211786,-0.626322575824964,
18.8807685350171));
#22800=CARTESIAN_POINT('Ctrl Pts',(-8.52682536005481,-1.20223728516816,
18.928490558472));
#22801=CARTESIAN_POINT('Ctrl Pts',(-7.50420367062632,-0.672615787292656,
18.9762125819268));
#22802=CARTESIAN_POINT('Ctrl Pts',(-7.39473674138445,0.47380082201821,19.0239346053817));
#22803=CARTESIAN_POINT('Ctrl Pts',(-8.3023365797739,1.18627681125878,19.0716566288366));
#22804=CARTESIAN_POINT('Ctrl Pts',(-9.20739053959603,0.870212372728869,
19.1114249817156));
#22805=CARTESIAN_POINT('Ctrl Pts',(-9.52704596967527,0.248558970814542,
19.1432396640189));
#22806=CARTESIAN_POINT('Ctrl Pts',(-9.52701192807412,-0.450463593150274,
19.175054346322));
#22807=CARTESIAN_POINT('Ctrl Pts',(-8.86663007628672,-1.14538460256273,
19.2148226992012));
#22808=CARTESIAN_POINT('Ctrl Pts',(-7.73368824589063,-0.926747206796109,
19.262544722656));
#22809=CARTESIAN_POINT('Ctrl Pts',(-7.30684738329652,0.142860631956667,
19.3102667461109));
#22810=CARTESIAN_POINT('Ctrl Pts',(-7.97413888435272,1.08146390454826,19.3579887695657));
#22811=CARTESIAN_POINT('Ctrl Pts',(-9.12667230207592,1.02645278821612,19.4057107930206));
#22812=CARTESIAN_POINT('Ctrl Pts',(-9.60432806254847,0.195270272771769,
19.4454791458997));
#22813=CARTESIAN_POINT('Ctrl Pts',(-9.43933382179755,-0.484000988661962,
19.4772938282029));
#22814=CARTESIAN_POINT('Ctrl Pts',(-8.98195234416682,-1.01261685109054,
19.5091085105061));
#22815=CARTESIAN_POINT('Ctrl Pts',(-8.02786420308556,-1.10607924214215,
19.5488768633852));
#22816=CARTESIAN_POINT('Ctrl Pts',(-7.31412302271695,-0.199474019713455,
19.59659888684));
#22817=CARTESIAN_POINT('Ctrl Pts',(-7.6911450727875,0.888693441876024,19.6443209102949));
#22818=CARTESIAN_POINT('Ctrl Pts',(-8.80989482891317,1.16192051569952,19.6920429337498));
#22819=CARTESIAN_POINT('Ctrl Pts',(-9.64550943889695,0.366239847673363,
19.7397649572046));
#22820=CARTESIAN_POINT('Ctrl Pts',(-9.46291298893969,-0.574864788356032,
19.7795333100837));
#22821=CARTESIAN_POINT('Ctrl Pts',(-8.89370267398479,-0.980613680455146,
19.8113479923869));
#22822=CARTESIAN_POINT('Ctrl Pts',(-8.20194419316234,-1.08112611899387,
19.8431626746901));
#22823=CARTESIAN_POINT('Ctrl Pts',(-7.41926139538849,-0.527567596738221,
19.8829310275693));
#22824=CARTESIAN_POINT('Ctrl Pts',(-7.47266495046468,0.625041427256538,
19.930653051024));
#22825=CARTESIAN_POINT('Ctrl Pts',(-8.46975416762413,1.20129410076522,19.978375074479));
#22826=CARTESIAN_POINT('Ctrl Pts',(-9.49457910241488,0.675948591854568,
20.0260970979338));
#22827=CARTESIAN_POINT('Ctrl Pts',(-9.60591833167572,-0.472512586381968,
20.0738191213886));
#22828=CARTESIAN_POINT('Ctrl Pts',(-8.85208422800519,-1.06475708288341,
20.1135874742677));
#22829=CARTESIAN_POINT('Ctrl Pts',(-8.15614408721544,-0.999183715360516,
20.1454021565709));
#22830=CARTESIAN_POINT('Ctrl Pts',(-7.56723626857872,-0.622593583732944,
20.1772168388742));
#22831=CARTESIAN_POINT('Ctrl Pts',(-7.33751148016779,0.308129748456874,
20.2169851917532));
#22832=CARTESIAN_POINT('Ctrl Pts',(-8.13202589224642,1.14485332938919,20.2647072152081));
#22833=CARTESIAN_POINT('Ctrl Pts',(-9.26310790487898,0.928271863421839,
20.312429238663));
#22834=CARTESIAN_POINT('Ctrl Pts',(-9.69441266856891,-0.139543781490679,
20.3601512621178));
#22835=CARTESIAN_POINT('Ctrl Pts',(-9.02719938225488,-1.08091827257006,
20.4078732855727));
#22836=CARTESIAN_POINT('Ctrl Pts',(-8.06961674413775,-1.03558737064229,
20.4476416384518));
#22837=CARTESIAN_POINT('Ctrl Pts',(-7.58621297435389,-0.530658324686794,
20.479456320755));
#22838=CARTESIAN_POINT('Ctrl Pts',(-7.38724446850424,0.13944918890389,20.5112710030583));
#22839=CARTESIAN_POINT('Ctrl Pts',(-7.82246699818582,0.993615887593619,
20.5510393559372));
#22840=CARTESIAN_POINT('Ctrl Pts',(-8.97077176781247,1.10655683650741,20.5987613793922));
#22841=CARTESIAN_POINT('Ctrl Pts',(-9.68445160636614,0.202723257388189,
20.646483402847));
#22842=CARTESIAN_POINT('Ctrl Pts',(-9.31197799098589,-0.887009488080663,
20.6942054263019));
#22843=CARTESIAN_POINT('Ctrl Pts',(-8.19147423515819,-1.16238347934517,
20.7419274497567));
#22844=CARTESIAN_POINT('Ctrl Pts',(-7.49695823929343,-0.501575692631794,
20.7816958026358));
#22845=CARTESIAN_POINT('Ctrl Pts',(-7.46174696796193,0.196559475127261,
20.813510484939));
#22846=CARTESIAN_POINT('Ctrl Pts',(-7.74971360013524,0.833511408043322,
20.8453251672423));
#22847=CARTESIAN_POINT('Ctrl Pts',(-8.63771535503727,1.19472088021124,20.8850935201213));
#22848=CARTESIAN_POINT('Ctrl Pts',(-9.58001953300302,0.528821234560933,
20.9328155435762));
#22849=CARTESIAN_POINT('Ctrl Pts',(-9.52838301578789,-0.621651590320803,
20.9805375670311));
#22850=CARTESIAN_POINT('Ctrl Pts',(-8.53370943520822,-1.20206395993246,
21.0282595904859));
#22851=CARTESIAN_POINT('Ctrl Pts',(-7.50615334947754,-0.677194459421418,
21.0759816139408));
#22852=CARTESIAN_POINT('Ctrl Pts',(-7.41327593151281,0.276950804532245,
21.1157499668198));
#22853=CARTESIAN_POINT('Ctrl Pts',(-7.84342241956686,0.827955836183989,
21.1475646491231));
#22854=CARTESIAN_POINT('Ctrl Pts',(-8.47794236898817,1.12124235117772,21.1793793314263));
#22855=CARTESIAN_POINT('Ctrl Pts',(-9.38582839088678,0.813407377963039,
21.2191476843054));
#22856=CARTESIAN_POINT('Ctrl Pts',(-9.66276494835087,-0.306711207289787,
21.2668697077602));
#22857=CARTESIAN_POINT('Ctrl Pts',(-8.87098453458713,-1.14297541618645,
21.3145917312151));
#22858=CARTESIAN_POINT('Ctrl Pts',(-7.73900775363358,-0.931120234320342,
21.3623137546699));
#22859=CARTESIAN_POINT('Ctrl Pts',(-7.30532610571126,0.138122362167578,
21.4100357781248));
#22860=CARTESIAN_POINT('Ctrl Pts',(-7.85936439009799,0.920465623739351,
21.4498041310038));
#22861=CARTESIAN_POINT('Ctrl Pts',(-8.54517508124857,1.05572922562215,21.4816188133071));
#22862=CARTESIAN_POINT('Ctrl Pts',(-9.21692408647285,0.862375094373378,
21.5134334956103));
#22863=CARTESIAN_POINT('Ctrl Pts',(-9.70210596903635,0.0355631808614804,
21.5532018484894));
#22864=CARTESIAN_POINT('Ctrl Pts',(-9.17867017339294,-0.992723972480452,
21.6009238719442));
#22865=CARTESIAN_POINT('Ctrl Pts',(-8.03273355651315,-1.10710631725258,
21.6486458953991));
#22866=CARTESIAN_POINT('Ctrl Pts',(-7.31528473835207,-0.206261578121178,
21.696367918854));
#22867=CARTESIAN_POINT('Ctrl Pts',(-7.68689445148562,0.886105449481559,
21.7440899423088));
#22868=CARTESIAN_POINT('Ctrl Pts',(-8.61775845399796,1.11525956425955,21.7838582951879));
#22869=CARTESIAN_POINT('Ctrl Pts',(-9.22490519083297,0.768841628751961,
21.8156729774911));
#22870=CARTESIAN_POINT('Ctrl Pts',(-9.60641007295241,0.183105706164161,
21.8474876597944));
#22871=CARTESIAN_POINT('Ctrl Pts',(-9.43236487056282,-0.759617830732116,
21.8872560126734));
#22872=CARTESIAN_POINT('Ctrl Pts',(-8.36372819600901,-1.1947903938464,21.9349780361283));
#22873=CARTESIAN_POINT('Ctrl Pts',(-7.4222718664851,-0.531530241039888,
21.9827000595831));
#22874=CARTESIAN_POINT('Ctrl Pts',(-7.46910254533488,0.619148227612382,
22.030422083038));
#22875=CARTESIAN_POINT('Ctrl Pts',(-8.46484635226162,1.20211801487061,22.0781441064929));
#22876=CARTESIAN_POINT('Ctrl Pts',(-9.31874605361725,0.766371873731396,
22.1179124593719));
#22877=CARTESIAN_POINT('Ctrl Pts',(-9.55124883403978,0.107148843804094,
22.1497271416752));
#22878=CARTESIAN_POINT('Ctrl Pts',(-9.45652849662567,-0.585426497780417,
22.1815418239783));
#22879=CARTESIAN_POINT('Ctrl Pts',(-8.7081020895998,-1.18449019452673,22.2213101768575));
#22880=CARTESIAN_POINT('Ctrl Pts',(-7.61521781807871,-0.814404432911052,
22.2690322003123));
#22881=CARTESIAN_POINT('Ctrl Pts',(-7.33719548426661,0.30316329774476,22.3167542237672));
#22882=CARTESIAN_POINT('Ctrl Pts',(-8.12547601519426,1.14272738419793,22.364476247222));
#22883=CARTESIAN_POINT('Ctrl Pts',(-9.25993542285189,0.932106031372354,
22.4121982706769));
#22884=CARTESIAN_POINT('Ctrl Pts',(-9.62060038945631,0.043882984296242,
22.4519666235559));
#22885=CARTESIAN_POINT('Ctrl Pts',(-9.36511565208,-0.606778290914208,22.4837813058592));
#22886=CARTESIAN_POINT('Ctrl Pts',(-8.84034563057633,-1.06856717192135,
22.5155959881624));
#22887=CARTESIAN_POINT('Ctrl Pts',(-7.88239092197955,-1.03193145478393,
22.5553643410415));
#22888=CARTESIAN_POINT('Ctrl Pts',(-7.29803287792558,-0.0370017194567047,
22.6030863644964));
#22889=CARTESIAN_POINT('Ctrl Pts',(-7.81897858119011,0.990066742210633,
22.6508083879512));
#22890=CARTESIAN_POINT('Ctrl Pts',(-8.96442744040265,1.10923452993118,22.6985304114061));
#22891=CARTESIAN_POINT('Ctrl Pts',(-9.68456102159392,0.207698547770979,
22.7462524348609));
#22892=CARTESIAN_POINT('Ctrl Pts',(-9.37616947743245,-0.699998568552913,
22.78602078774));
#22893=CARTESIAN_POINT('Ctrl Pts',(-8.75724433503361,-1.02490503847511,
22.8178354700433));
#22894=CARTESIAN_POINT('Ctrl Pts',(-8.05824652988369,-1.03078844619088,
22.8496501523464));
#22895=CARTESIAN_POINT('Ctrl Pts',(-7.35776007830284,-0.376312983973493,
22.8894185052256));
#22896=CARTESIAN_POINT('Ctrl Pts',(-7.56679892742373,0.758439086501402,
22.9371405286804));
#22897=CARTESIAN_POINT('Ctrl Pts',(-8.63275509706559,1.19431922496145,22.9848625521353));
#22898=CARTESIAN_POINT('Ctrl Pts',(-9.57697357271459,0.534997208838448,
23.0325845755901));
#22899=CARTESIAN_POINT('Ctrl Pts',(-9.53172098907367,-0.617960598526017,
23.080306599045));
#22900=CARTESIAN_POINT('Ctrl Pts',(-8.70461176387205,-1.10263546797914,
23.120074951924));
#22901=CARTESIAN_POINT('Ctrl Pts',(-8.02396811303862,-0.94339738625594,
23.1518896342273));
#22902=CARTESIAN_POINT('Ctrl Pts',(-7.49149931215251,-0.490507198491067,
23.1837043165305));
#22903=CARTESIAN_POINT('Ctrl Pts',(-7.38996361074661,0.462755567399329,
23.2234726694096));
#22904=CARTESIAN_POINT('Ctrl Pts',(-8.29049430233965,1.18414587464485,23.2711946928644));
#22905=CARTESIAN_POINT('Ctrl Pts',(-9.38181438475884,0.816349017113292,
23.3189167163193));
#22906=CARTESIAN_POINT('Ctrl Pts',(-9.66450224059603,-0.300047698603672,
23.3666387397741));
#22907=CARTESIAN_POINT('Ctrl Pts',(-8.87592382612184,-1.1423680569675,23.414360763229));
#22908=CARTESIAN_POINT('Ctrl Pts',(-7.93330717426711,-0.967744899456104,
23.4541291161081));
#22909=CARTESIAN_POINT('Ctrl Pts',(-7.52275427457137,-0.40198977341469,
23.4859437984113));
#22910=CARTESIAN_POINT('Ctrl Pts',(-7.41638948221304,0.288893050975484,
23.5177584807145));
#22911=CARTESIAN_POINT('Ctrl Pts',(-7.96330251111076,1.0762338528618,23.5575268335936));
#22912=CARTESIAN_POINT('Ctrl Pts',(-9.11632231352085,1.03258941290663,23.6052488570485));
#22913=CARTESIAN_POINT('Ctrl Pts',(-9.70099501608219,0.0404140848616688,
23.6529708805033));
#22914=CARTESIAN_POINT('Ctrl Pts',(-9.18434379973964,-0.988821345617322,
23.7006929039582));
#22915=CARTESIAN_POINT('Ctrl Pts',(-8.03686629447588,-1.10987867419518,
23.7484149274131));
#22916=CARTESIAN_POINT('Ctrl Pts',(-7.43826157375447,-0.361085119319684,
23.7881832802921));
#22917=CARTESIAN_POINT('Ctrl Pts',(-7.49794123728335,0.335385184319912,
23.8199979625954));
#22918=CARTESIAN_POINT('Ctrl Pts',(-7.86953258335037,0.927459856653405,
23.8518126448985));
#22919=CARTESIAN_POINT('Ctrl Pts',(-8.79827787305733,1.16505528240947,23.8915809977777));
#22920=CARTESIAN_POINT('Ctrl Pts',(-9.64169728990653,0.377652469885521,
23.9393030212325));
#22921=CARTESIAN_POINT('Ctrl Pts',(-9.43469855296966,-0.755222445366839,
23.9870250446874));
#22922=CARTESIAN_POINT('Ctrl Pts',(-8.37057230129222,-1.19555115348436,
24.0347470681422));
#22923=CARTESIAN_POINT('Ctrl Pts',(-7.42358336856485,-0.53633080854597,
24.0824690915971));
#22924=CARTESIAN_POINT('Ctrl Pts',(-7.46080640494651,0.421601258489856,
24.1222374444762));
#22925=CARTESIAN_POINT('Ctrl Pts',(-7.96162519206712,0.909262092018453,
24.1540521267794));
#22926=CARTESIAN_POINT('Ctrl Pts',(-8.63002436311974,1.11389614154808,24.1858668090826));
#22927=CARTESIAN_POINT('Ctrl Pts',(-9.48784475277574,0.685919999008078,
24.2256351619617));
#22928=CARTESIAN_POINT('Ctrl Pts',(-9.61050241956603,-0.461387544184418,
24.2733571854165));
#22929=CARTESIAN_POINT('Ctrl Pts',(-8.7127427526925,-1.18269304897183,24.3210792088714));
#22930=CARTESIAN_POINT('Ctrl Pts',(-7.61989594642513,-0.819457713778855,
24.3688012323262));
#22931=CARTESIAN_POINT('Ctrl Pts',(-7.33504640190931,0.298674764453505,
24.4165232557811));
#22932=CARTESIAN_POINT('Ctrl Pts',(-7.98995121235915,0.998759822673351,
24.4562916086602));
#22933=CARTESIAN_POINT('Ctrl Pts',(-8.68776329032791,1.03987976834045,24.4881062909634));
#22934=CARTESIAN_POINT('Ctrl Pts',(-9.32713012937044,0.757315454911642,
24.5199209732667));
#22935=CARTESIAN_POINT('Ctrl Pts',(-9.6958438758722,-0.127596728660042,
24.5596893261457));
#22936=CARTESIAN_POINT('Ctrl Pts',(-9.03794499462271,-1.07550419457617,
24.6074113496006));
#22937=CARTESIAN_POINT('Ctrl Pts',(-7.88707627331942,-1.03360864556243,
24.6551333730554));
#22938=CARTESIAN_POINT('Ctrl Pts',(-7.29826447283417,-0.0438840806905483,
24.7028553965103));
#22939=CARTESIAN_POINT('Ctrl Pts',(-7.81441657777274,0.988078373304951,
24.7505774199651));
#22940=CARTESIAN_POINT('Ctrl Pts',(-8.76774141647179,1.08902960614764,24.7903457728442));
#22941=CARTESIAN_POINT('Ctrl Pts',(-9.32236803150491,0.663562963521387,
24.8221604551474));
#22942=CARTESIAN_POINT('Ctrl Pts',(-9.62101545059055,0.0315485133984316,
24.8539751374507));
#22943=CARTESIAN_POINT('Ctrl Pts',(-9.32087705117602,-0.878910898486496,
24.8937434903297));
#22944=CARTESIAN_POINT('Ctrl Pts',(-8.20314295733665,-1.16531969262162,
24.9414655137846));
#22945=CARTESIAN_POINT('Ctrl Pts',(-7.36020604022749,-0.380646891719252,
24.9891875372395));
#22946=CARTESIAN_POINT('Ctrl Pts',(-7.56247108791455,0.753082750296701,
25.0369095606943));
#22947=CARTESIAN_POINT('Ctrl Pts',(-8.62800411895744,1.19580033707794,25.0846315841492));
#22948=CARTESIAN_POINT('Ctrl Pts',(-9.41500945814661,0.648404688957932,
25.1243999370283));
#22949=CARTESIAN_POINT('Ctrl Pts',(-9.55607381873532,-0.03623637923947,
25.1562146193315));
#22950=CARTESIAN_POINT('Ctrl Pts',(-9.36841318440126,-0.709598118880296,
25.1880293016347));
#22951=CARTESIAN_POINT('Ctrl Pts',(-8.54573811554186,-1.20176184221852,
25.2277976545138));
#22952=CARTESIAN_POINT('Ctrl Pts',(-7.51305675689754,-0.687049579495533,
25.2755196779686));
#22953=CARTESIAN_POINT('Ctrl Pts',(-7.38897779306161,0.457877693930538,
25.3232417014235));
#22954=CARTESIAN_POINT('Ctrl Pts',(-8.2837168214319,1.18292674179725,25.3709637248784));
#22955=CARTESIAN_POINT('Ctrl Pts',(-9.37919050223605,0.820577577931373,
25.4186857483332));
#22956=CARTESIAN_POINT('Ctrl Pts',(-9.61621646562617,-0.108313207991237,
25.4584541012123));
#22957=CARTESIAN_POINT('Ctrl Pts',(-9.2749506328032,-0.718370727769788,
25.4902687835155));
#22958=CARTESIAN_POINT('Ctrl Pts',(-8.69246525801796,-1.1048203807029,25.5220834658188));
#22959=CARTESIAN_POINT('Ctrl Pts',(-7.74830215233154,-0.938761868865786,
25.5618518186978));
#22960=CARTESIAN_POINT('Ctrl Pts',(-7.30409883310168,0.126152640883285,
25.6095738421527));
#22961=CARTESIAN_POINT('Ctrl Pts',(-7.95936549339064,1.07318994459167,25.6572958656076));
#22962=CARTESIAN_POINT('Ctrl Pts',(-9.11039916814726,1.03610180258297,25.7050178890624));
#22963=CARTESIAN_POINT('Ctrl Pts',(-9.70177735444918,0.0453286990647764,
25.7527399125173));
#22964=CARTESIAN_POINT('Ctrl Pts',(-9.27327535899608,-0.812229135361383,
25.7925082653963));
#22965=CARTESIAN_POINT('Ctrl Pts',(-8.61604415988881,-1.05030411726996,
25.8243229476996));
#22966=CARTESIAN_POINT('Ctrl Pts',(-7.92269179652815,-0.961450044133608,
25.8561376300028));
#22967=CARTESIAN_POINT('Ctrl Pts',(-7.31731389777389,-0.218121718833848,
25.8959059828819));
#22968=CARTESIAN_POINT('Ctrl Pts',(-7.67813478609319,0.877856286621276,
25.9436280063367));
#22969=CARTESIAN_POINT('Ctrl Pts',(-8.7933089252946,1.16532922440482,25.9913500297916));
#22970=CARTESIAN_POINT('Ctrl Pts',(-9.63951597410066,0.384184115444669,
26.0390720532464));
#22971=CARTESIAN_POINT('Ctrl Pts',(-9.43850572746812,-0.752017619564397,
26.0867940767013));
#22972=CARTESIAN_POINT('Ctrl Pts',(-8.55336765023902,-1.12018875332168,
26.1265624295803));
#22973=CARTESIAN_POINT('Ctrl Pts',(-7.9005669296872,-0.870221224754899,
26.1583771118836));
#22974=CARTESIAN_POINT('Ctrl Pts',(-7.43435225028074,-0.34937919611602,
26.1901917941868));
#22975=CARTESIAN_POINT('Ctrl Pts',(-7.46287726373823,0.608851320565757,
26.2299601470659));
#22976=CARTESIAN_POINT('Ctrl Pts',(-8.45282457279144,1.20161082254541,26.2776821705207));
#22977=CARTESIAN_POINT('Ctrl Pts',(-9.48426620400552,0.689378246365516,
26.3254041939756));
#22978=CARTESIAN_POINT('Ctrl Pts',(-9.61312631029696,-0.455020776575367,
26.3731262174304));
#22979=CARTESIAN_POINT('Ctrl Pts',(-8.71771879103822,-1.18276034286521,
26.4208482408854));
#22980=CARTESIAN_POINT('Ctrl Pts',(-7.80744356640935,-0.882063793301015,
26.4606165937644));
#22981=CARTESIAN_POINT('Ctrl Pts',(-7.47730934038002,-0.265911264380824,
26.4924312760676));
#22982=CARTESIAN_POINT('Ctrl Pts',(-7.4655089049693,0.433011689752842,26.5242459583709));
#22983=CARTESIAN_POINT('Ctrl Pts',(-8.11403107601491,1.13901338462003,26.5640143112499));
#22984=CARTESIAN_POINT('Ctrl Pts',(-9.25051206695811,0.939588062472506,
26.6117363347048));
#22985=CARTESIAN_POINT('Ctrl Pts',(-9.69540024485459,-0.122640048560796,
26.6594583581596));
#22986=CARTESIAN_POINT('Ctrl Pts',(-9.04409496258458,-1.07240606184442,
26.7071803816145));
#22987=CARTESIAN_POINT('Ctrl Pts',(-7.89079538986508,-1.03691525382556,
26.7549024050694));
#22988=CARTESIAN_POINT('Ctrl Pts',(-7.39913614463224,-0.213938591902498,
26.7946707579484));
#22989=CARTESIAN_POINT('Ctrl Pts',(-7.55260665586685,0.468028671440933,
26.8264854402517));
#22990=CARTESIAN_POINT('Ctrl Pts',(-8.00097309834699,1.00431225253255,26.8583001225549));
#22991=CARTESIAN_POINT('Ctrl Pts',(-8.95334217548371,1.11391398795126,26.8980684754339));
#22992=CARTESIAN_POINT('Ctrl Pts',(-9.68232991269352,0.219522361823951,
26.9457904988889));
#22993=CARTESIAN_POINT('Ctrl Pts',(-9.32378460508592,-0.874872134276119,
26.9935125223437));
#22994=CARTESIAN_POINT('Ctrl Pts',(-8.20982093399049,-1.16700051389895,
27.0412345457986));
#22995=CARTESIAN_POINT('Ctrl Pts',(-7.36085519035604,-0.385580864783285,
27.0889565692533));
#22996=CARTESIAN_POINT('Ctrl Pts',(-7.52749254142181,0.558480252265147,
27.1287249221325));
#22997=CARTESIAN_POINT('Ctrl Pts',(-8.08975193490343,0.973807738151165,
27.1605396044356));
#22998=CARTESIAN_POINT('Ctrl Pts',(-8.77970959220288,1.08601726192087,27.192354286739));
#22999=CARTESIAN_POINT('Ctrl Pts',(-9.57165197508597,0.545788919748368,
27.232122639618));
#23000=CARTESIAN_POINT('Ctrl Pts',(-9.53776977793861,-0.607559032348173,
27.2798446630729));
#23001=CARTESIAN_POINT('Ctrl Pts',(-8.55057944115751,-1.20060986462781,
27.3275666865277));
#23002=CARTESIAN_POINT('Ctrl Pts',(-7.5170072729736,-0.692689965571765,
27.3752887099826));
#23003=CARTESIAN_POINT('Ctrl Pts',(-7.38624052039643,0.453721635167412,
27.4230107334374));
#23004=CARTESIAN_POINT('Ctrl Pts',(-8.12993986576823,1.05864368236566,27.4627790863165));
#23005=CARTESIAN_POINT('Ctrl Pts',(-8.8268904211843,1.00486199964796,27.4945937686197));
#23006=CARTESIAN_POINT('Ctrl Pts',(-9.42208951743369,0.638296068450471,
27.526408450923));
#23007=CARTESIAN_POINT('Ctrl Pts',(-9.66753855376051,-0.288404622203879,
27.566176803802));
#23008=CARTESIAN_POINT('Ctrl Pts',(-8.88730376835095,-1.13845943309884,
27.6138988272569));
#23009=CARTESIAN_POINT('Ctrl Pts',(-7.75271713556691,-0.941058259319852,
27.6616208507118));
#23010=CARTESIAN_POINT('Ctrl Pts',(-7.30339603824854,0.119302340762093,
27.7093428741666));
#23011=CARTESIAN_POINT('Ctrl Pts',(-7.95457620017757,1.07183785117575,27.7570648976215));
#23012=CARTESIAN_POINT('Ctrl Pts',(-8.91278904795361,1.04272534785048,27.7968332505005));
#23013=CARTESIAN_POINT('Ctrl Pts',(-9.40467199804332,0.546052709685484,
27.8286479328038));
#23014=CARTESIAN_POINT('Ctrl Pts',(-9.61495692658599,-0.12059021941417,
27.860462615107));
#23015=CARTESIAN_POINT('Ctrl Pts',(-9.19425784119395,-0.98200282614995,
27.9002309679861));
#23016=CARTESIAN_POINT('Ctrl Pts',(-8.04802974380756,-1.1143684208142,27.9479529914409));
#23017=CARTESIAN_POINT('Ctrl Pts',(-7.31915026362204,-0.222747002236805,
27.9956750148958));
#23018=CARTESIAN_POINT('Ctrl Pts',(-7.67312128813442,0.873135548270785,
28.0433970383507));
#23019=CARTESIAN_POINT('Ctrl Pts',(-8.78880236016895,1.16744023289704,28.0911190618055));
#23020=CARTESIAN_POINT('Ctrl Pts',(-9.4944063106267,0.518485331080839,28.1308874146846));
#23021=CARTESIAN_POINT('Ctrl Pts',(-9.54143198385559,-0.178953649868804,
28.1627020969878));
#23022=CARTESIAN_POINT('Ctrl Pts',(-9.2642902385457,-0.820689576163826,
28.1945167792911));
#23023=CARTESIAN_POINT('Ctrl Pts',(-8.38253104166786,-1.19688117390719,
28.2342851321701));
#23024=CARTESIAN_POINT('Ctrl Pts',(-7.42908821758638,-0.547030203993041,
28.282007155625));
#23025=CARTESIAN_POINT('Ctrl Pts',(-7.4612397960453,0.604151939156692,28.3297291790798));
#23026=CARTESIAN_POINT('Ctrl Pts',(-8.44594441868381,1.20132097455935,28.3774512025347));
#23027=CARTESIAN_POINT('Ctrl Pts',(-9.48223928754388,0.693923254147899,
28.4251732259896));
#23028=CARTESIAN_POINT('Ctrl Pts',(-9.59125710079042,-0.258512841292752,
28.4649415788686));
#23029=CARTESIAN_POINT('Ctrl Pts',(-9.17050079378615,-0.816721293551335,
28.4967562611719));
#23030=CARTESIAN_POINT('Ctrl Pts',(-8.5410371348917,-1.12070821481403,28.5285709434751));
#23031=CARTESIAN_POINT('Ctrl Pts',(-7.62806957928328,-0.828287897936413,
28.5683392963542));
#23032=CARTESIAN_POINT('Ctrl Pts',(-7.33220907315438,0.286981604349355,
28.616061319809));
#23033=CARTESIAN_POINT('Ctrl Pts',(-8.10971802963793,1.13653082253137,28.6637833432638));
#23034=CARTESIAN_POINT('Ctrl Pts',(-9.24511928569963,0.94387040363248,28.7115053667187));
#23035=CARTESIAN_POINT('Ctrl Pts',(-9.69684108623964,-0.117876702228018,
28.7592273901736));
#23036=CARTESIAN_POINT('Ctrl Pts',(-9.15612729992706,-0.909487720987729,
28.7989957430526));
#23037=CARTESIAN_POINT('Ctrl Pts',(-8.47270492162156,-1.05634272967534,
28.8308104253559));
#23038=CARTESIAN_POINT('Ctrl Pts',(-7.79777869557615,-0.874389043558764,
28.8626251076591));
#23039=CARTESIAN_POINT('Ctrl Pts',(-7.29866841691336,-0.0559097679814885,
28.9023934605382));
#23040=CARTESIAN_POINT('Ctrl Pts',(-7.80462023258882,0.981091778944407,
28.950115483993));
#23041=CARTESIAN_POINT('Ctrl Pts',(-8.94845616402851,1.11485849141853,28.9978375074479));
#23042=CARTESIAN_POINT('Ctrl Pts',(-9.68105338849322,0.226289253312137,
29.0455595309028));
#23043=CARTESIAN_POINT('Ctrl Pts',(-9.32799092443192,-0.872212497622574,
29.0932815543577));
#23044=CARTESIAN_POINT('Ctrl Pts',(-8.40113958681821,-1.1170934666179,29.1330499072367));
#23045=CARTESIAN_POINT('Ctrl Pts',(-7.78821550048514,-0.781003980273933,
29.1648645895399));
#23046=CARTESIAN_POINT('Ctrl Pts',(-7.39684779309566,-0.201811312772201,
29.1966792718432));
#23047=CARTESIAN_POINT('Ctrl Pts',(-7.55490987902498,0.743724623326478,
29.2364476247223));
#23048=CARTESIAN_POINT('Ctrl Pts',(-8.61602196756742,1.1969251851499,29.284169648177));
#23049=CARTESIAN_POINT('Ctrl Pts',(-9.56857936365253,0.549701954262166,
29.331891671632));
#23050=CARTESIAN_POINT('Ctrl Pts',(-9.54122335203833,-0.601610010653767,
29.3796136950868));
#23051=CARTESIAN_POINT('Ctrl Pts',(-8.55551746389829,-1.20134333884888,
29.4273357185417));
#23052=CARTESIAN_POINT('Ctrl Pts',(-7.6943163535033,-0.780136065581471,
29.4671040714207));
#23053=CARTESIAN_POINT('Ctrl Pts',(-7.45075543190132,-0.124914290005815,
29.498918753724));
#23054=CARTESIAN_POINT('Ctrl Pts',(-7.53360098225563,0.569107464161486,
29.5307334360272));
#23055=CARTESIAN_POINT('Ctrl Pts',(-8.27207885390538,1.18088449447138,29.5705017889063));
#23056=CARTESIAN_POINT('Ctrl Pts',(-9.37052414128468,0.829120622166084,
29.6182238123611));
#23057=CARTESIAN_POINT('Ctrl Pts',(-9.66839871578049,-0.283165032010691,
29.665945835816));
#23058=CARTESIAN_POINT('Ctrl Pts',(-8.89262325021065,-1.13673653623531,
29.7136678592708));
#23059=CARTESIAN_POINT('Ctrl Pts',(-7.94740422892346,-0.975943072842761,
29.7534362121499));
#23060=CARTESIAN_POINT('Ctrl Pts',(-7.52860489572998,-0.416034089157435,
29.7852508944531));
#23061=CARTESIAN_POINT('Ctrl Pts',(-7.41259114042627,0.272911730206623,
29.8170655767564));
#23062=CARTESIAN_POINT('Ctrl Pts',(-7.94709221312467,1.06881550059101,29.8568339296354));
#23063=CARTESIAN_POINT('Ctrl Pts',(-9.10241563751445,1.0405751389091,29.9045559530903));
#23064=CARTESIAN_POINT('Ctrl Pts',(-9.5986718480284,0.223190340067093,29.9443243059693));
#23065=CARTESIAN_POINT('Ctrl Pts',(-9.45136298239413,-0.462871519683194,
29.9761389882726));
#23066=CARTESIAN_POINT('Ctrl Pts',(-9.22802350159151,-0.72929719873085,
29.9920463294242));
#23067=CARTESIAN_POINT('Ctrl Pts',(-9.09015970213924,-0.82760676144889,
30.));
#23068=CARTESIAN_POINT('Ctrl Pts',(-8.96251688654953,0.969001292714065,
1.73389339417778));
#23069=CARTESIAN_POINT('Ctrl Pts',(-9.12393436899475,0.89195463449329,1.74184706475359));
#23070=CARTESIAN_POINT('Ctrl Pts',(-9.40504227116756,0.655650918757411,
1.75775440590521));
#23071=CARTESIAN_POINT('Ctrl Pts',(-9.68384680217516,-0.0311347557633745,
1.78956908820845));
#23072=CARTESIAN_POINT('Ctrl Pts',(-9.3171516591104,-0.972316947591156,
1.8293374410875));
#23073=CARTESIAN_POINT('Ctrl Pts',(-8.1203802128438,-1.21312531614354,1.87705946454236));
#23074=CARTESIAN_POINT('Ctrl Pts',(-7.41865918333397,-0.482923354571855,
1.91682781742141));
#23075=CARTESIAN_POINT('Ctrl Pts',(-7.41327429528892,0.255051675597989,
1.94864249972466));
#23076=CARTESIAN_POINT('Ctrl Pts',(-7.74650629928063,0.914194267158726,
1.9804571820279));
#23077=CARTESIAN_POINT('Ctrl Pts',(-8.70043812865199,1.25445422207282,2.02022553490695));
#23078=CARTESIAN_POINT('Ctrl Pts',(-9.66372213760587,0.5084118152494,2.06794755836181));
#23079=CARTESIAN_POINT('Ctrl Pts',(-9.55738109299735,-0.703265592318366,
2.11566958181668));
#23080=CARTESIAN_POINT('Ctrl Pts',(-8.47898877892832,-1.27024239984107,
2.16339160527153));
#23081=CARTESIAN_POINT('Ctrl Pts',(-7.59875658277994,-0.76892502565052,
2.20315995815059));
#23082=CARTESIAN_POINT('Ctrl Pts',(-7.3855597050091,-0.0620612536970827,
2.23497464045383));
#23083=CARTESIAN_POINT('Ctrl Pts',(-7.51904000752238,0.664170613866673,
2.26678932275707));
#23084=CARTESIAN_POINT('Ctrl Pts',(-8.33790718168219,1.25997621452937,2.30655767563613));
#23085=CARTESIAN_POINT('Ctrl Pts',(-9.47313874820412,0.816432151476354,
2.35427969909098));
#23086=CARTESIAN_POINT('Ctrl Pts',(-9.71229297188154,-0.376327816436324,
2.40200172254585));
#23087=CARTESIAN_POINT('Ctrl Pts',(-8.83974515101956,-1.22398743093948,
2.44972374600071));
#23088=CARTESIAN_POINT('Ctrl Pts',(-7.65288086934604,-0.946688199618081,
2.49744576945557));
#23089=CARTESIAN_POINT('Ctrl Pts',(-7.31540450356857,0.00807318411347469,
2.53721412233462));
#23090=CARTESIAN_POINT('Ctrl Pts',(-7.6165690570546,0.682257445519576,2.56902880463787));
#23091=CARTESIAN_POINT('Ctrl Pts',(-8.19271835958521,1.14407521357768,2.60084348694111));
#23092=CARTESIAN_POINT('Ctrl Pts',(-9.20178133687243,1.05893083384115,2.64061183982016));
#23093=CARTESIAN_POINT('Ctrl Pts',(-9.77011946603895,-0.0192825748483143,
2.68833386327502));
#23094=CARTESIAN_POINT('Ctrl Pts',(-9.17057421212321,-1.07777272054635,
2.73605588672988));
#23095=CARTESIAN_POINT('Ctrl Pts',(-7.95610586271703,-1.14793494130798,
2.78377791018475));
#23096=CARTESIAN_POINT('Ctrl Pts',(-7.23996422244131,-0.161682533818757,
2.83149993363961));
#23097=CARTESIAN_POINT('Ctrl Pts',(-7.60942829901139,0.781160600976021,
2.87126828651866));
#23098=CARTESIAN_POINT('Ctrl Pts',(-8.27828889582619,1.09396997251331,2.9030829688219));
#23099=CARTESIAN_POINT('Ctrl Pts',(-9.01616168526782,1.06625838374102,2.93489765112514));
#23100=CARTESIAN_POINT('Ctrl Pts',(-9.72356051529724,0.341659331902824,
2.9746660040042));
#23101=CARTESIAN_POINT('Ctrl Pts',(-9.44791592231979,-0.845594970502356,
3.02238802745905));
#23102=CARTESIAN_POINT('Ctrl Pts',(-8.30195997305303,-1.2538117450032,3.07011005091392));
#23103=CARTESIAN_POINT('Ctrl Pts',(-7.3376086220987,-0.512271154700922,
3.11783207436878));
#23104=CARTESIAN_POINT('Ctrl Pts',(-7.44130827730874,0.702141914088998,
3.16555409782365));
#23105=CARTESIAN_POINT('Ctrl Pts',(-8.33759911760778,1.17343759126272,3.2053224507027));
#23106=CARTESIAN_POINT('Ctrl Pts',(-9.048091740403,0.972379329670738,3.23713713300594));
#23107=CARTESIAN_POINT('Ctrl Pts',(-9.58797938135923,0.468647727902608,
3.26895181530918));
#23108=CARTESIAN_POINT('Ctrl Pts',(-9.64886220328975,-0.542168856809507,
3.30872016818823));
#23109=CARTESIAN_POINT('Ctrl Pts',(-8.66360959361254,-1.25968541784617,
3.3564421916431));
#23110=CARTESIAN_POINT('Ctrl Pts',(-7.52988896786481,-0.818625878810704,
3.40416421509795));
#23111=CARTESIAN_POINT('Ctrl Pts',(-7.28576943901448,0.373121422369535,
3.45188623855282));
#23112=CARTESIAN_POINT('Ctrl Pts',(-8.15875752784666,1.22367683912943,3.49960826200768));
#23113=CARTESIAN_POINT('Ctrl Pts',(-9.14493928233647,0.993671549987388,
3.53937661488673));
#23114=CARTESIAN_POINT('Ctrl Pts',(-9.55070350372043,0.376760220734811,
3.57119129718998));
#23115=CARTESIAN_POINT('Ctrl Pts',(-9.62941435269904,-0.357425582565709,
3.60300597949321));
#23116=CARTESIAN_POINT('Ctrl Pts',(-9.01410119783594,-1.1616933286404,3.64277433237227));
#23117=CARTESIAN_POINT('Ctrl Pts',(-7.79954467407403,-1.05968758954777,
3.69049635582713));
#23118=CARTESIAN_POINT('Ctrl Pts',(-7.23074064851598,0.0156346666816528,
3.73821837928199));
#23119=CARTESIAN_POINT('Ctrl Pts',(-7.82585959046674,1.07661978399709,3.78594040273685));
#23120=CARTESIAN_POINT('Ctrl Pts',(-9.04256021742503,1.14867743161063,3.83366242619172));
#23121=CARTESIAN_POINT('Ctrl Pts',(-9.63787582997991,0.32949722715489,3.87343077907076));
#23122=CARTESIAN_POINT('Ctrl Pts',(-9.54110428679668,-0.402526993718299,
3.90524546137401));
#23123=CARTESIAN_POINT('Ctrl Pts',(-9.12026732761714,-1.00925629522235,
3.93706014367725));
#23124=CARTESIAN_POINT('Ctrl Pts',(-8.12871927263138,-1.21490001765928,
3.97682849655631));
#23125=CARTESIAN_POINT('Ctrl Pts',(-7.27694707414092,-0.343099098814263,
4.02455052001116));
#23126=CARTESIAN_POINT('Ctrl Pts',(-7.55034783376434,0.842273415997345,
4.07227254346603));
#23127=CARTESIAN_POINT('Ctrl Pts',(-8.69458871454493,1.25527315084461,4.11999456692089));
#23128=CARTESIAN_POINT('Ctrl Pts',(-9.66186840419519,0.513705404640438,
4.16771659037575));
#23129=CARTESIAN_POINT('Ctrl Pts',(-9.57610546723251,-0.49530480569805,
4.2074849432548));
#23130=CARTESIAN_POINT('Ctrl Pts',(-9.0239736441167,-0.98558497194781,4.23929962555805));
#23131=CARTESIAN_POINT('Ctrl Pts',(-8.30874409956685,-1.16908126651006,
4.27111430786129));
#23132=CARTESIAN_POINT('Ctrl Pts',(-7.42433423631398,-0.675851016317698,
4.31088266074034));
#23133=CARTESIAN_POINT('Ctrl Pts',(-7.35057965317154,0.540747924042572,
4.3586046841952));
#23134=CARTESIAN_POINT('Ctrl Pts',(-8.33290414333639,1.25830946861962,4.40632670765007));
#23135=CARTESIAN_POINT('Ctrl Pts',(-9.46845713256172,0.82198919302504,4.45404873110492));
#23136=CARTESIAN_POINT('Ctrl Pts',(-9.71477345998143,-0.371694595533183,
4.50177075455979));
#23137=CARTESIAN_POINT('Ctrl Pts',(-8.98974083571195,-1.07864903513211,
4.54153910743884));
#23138=CARTESIAN_POINT('Ctrl Pts',(-8.25140932968082,-1.08817682170158,
4.57335378974208));
#23139=CARTESIAN_POINT('Ctrl Pts',(-7.59045685283196,-0.758986884336549,
4.60516847204533));
#23140=CARTESIAN_POINT('Ctrl Pts',(-7.24432911621094,0.192670867097964,
4.64493682492437));
#23141=CARTESIAN_POINT('Ctrl Pts',(-7.98454701788834,1.16098392507899,4.69265884837925));
#23142=CARTESIAN_POINT('Ctrl Pts',(-9.19691857333501,1.06092801182391,4.74038087183409));
#23143=CARTESIAN_POINT('Ctrl Pts',(-9.77020913005612,-0.0120090374981049,
4.78810289528898));
#23144=CARTESIAN_POINT('Ctrl Pts',(-9.17548452143473,-1.07589594883799,
4.83582491874381));
#23145=CARTESIAN_POINT('Ctrl Pts',(-8.16463079918994,-1.13615902333401,
4.87559327162288));
#23146=CARTESIAN_POINT('Ctrl Pts',(-7.60003131611499,-0.660289697545374,
4.90740795392612));
#23147=CARTESIAN_POINT('Ctrl Pts',(-7.31556584999249,0.0211085634582759,
4.93922263622936));
#23148=CARTESIAN_POINT('Ctrl Pts',(-7.67645521294405,0.96726698234605,4.97899098910842));
#23149=CARTESIAN_POINT('Ctrl Pts',(-8.86979428821997,1.21524797282673,5.02671301256327));
#23150=CARTESIAN_POINT('Ctrl Pts',(-9.72118982712491,0.346351194972045,
5.07443503601814));
#23151=CARTESIAN_POINT('Ctrl Pts',(-9.45274261220889,-0.840152941993902,
5.122157059473));
#23152=CARTESIAN_POINT('Ctrl Pts',(-8.3069013646354,-1.25560517219555,5.16987908292785));
#23153=CARTESIAN_POINT('Ctrl Pts',(-7.50301102084912,-0.639799032983755,
5.20964743580691));
#23154=CARTESIAN_POINT('Ctrl Pts',(-7.38738205917888,0.0894842691273791,
5.24146211811015));
#23155=CARTESIAN_POINT('Ctrl Pts',(-7.61807862935953,0.790913726750847,
5.2732768004134));
#23156=CARTESIAN_POINT('Ctrl Pts',(-8.51005392413996,1.27032686739803,5.31304515329244));
#23157=CARTESIAN_POINT('Ctrl Pts',(-9.5747692988779,0.677086704380666,5.36076717674732));
#23158=CARTESIAN_POINT('Ctrl Pts',(-9.65013915021099,-0.537069529282636,
5.40848920020216));
#23159=CARTESIAN_POINT('Ctrl Pts',(-8.67082039814986,-1.25872786679072,
5.45621122365704));
#23160=CARTESIAN_POINT('Ctrl Pts',(-7.53245251019283,-0.823215212682402,
5.50393324711189));
#23161=CARTESIAN_POINT('Ctrl Pts',(-7.32741674876059,0.168458736989412,
5.54370159999096));
#23162=CARTESIAN_POINT('Ctrl Pts',(-7.71712665940812,0.795635248872751,
5.57551628229418));
#23163=CARTESIAN_POINT('Ctrl Pts',(-8.35052222000327,1.17515370077386,5.60733096459744));
#23164=CARTESIAN_POINT('Ctrl Pts',(-9.33875141408655,0.954110840936048,
5.64709931747647));
#23165=CARTESIAN_POINT('Ctrl Pts',(-9.75580141396196,-0.191149835863871,
5.69482134093136));
#23166=CARTESIAN_POINT('Ctrl Pts',(-9.01840327573551,-1.15867242473384,
5.7425433643862));
#23167=CARTESIAN_POINT('Ctrl Pts',(-7.80562437442478,-1.06368131583976,
5.79026538784108));
#23168=CARTESIAN_POINT('Ctrl Pts',(-7.22967663147079,0.0104866959751704,
5.83798741129593));
#23169=CARTESIAN_POINT('Ctrl Pts',(-7.72344902443187,0.894593991428199,
5.87775576417499));
#23170=CARTESIAN_POINT('Ctrl Pts',(-8.42851681405126,1.11391932867013,5.90957044647822));
#23171=CARTESIAN_POINT('Ctrl Pts',(-9.15583523570149,0.986514049959575,
5.94138512878147));
#23172=CARTESIAN_POINT('Ctrl Pts',(-9.75856315988134,0.172772115844345,
5.98115348166051));
#23173=CARTESIAN_POINT('Ctrl Pts',(-9.32463867961743,-0.966202100566147,
6.02887550511538));
#23174=CARTESIAN_POINT('Ctrl Pts',(-8.13394924709671,-1.21543020796378,
6.07659752857024));
#23175=CARTESIAN_POINT('Ctrl Pts',(-7.27893185676339,-0.350097187409828,
6.12431955202511));
#23176=CARTESIAN_POINT('Ctrl Pts',(-7.54617495858737,0.839076409987852,
6.17204157547996));
#23177=CARTESIAN_POINT('Ctrl Pts',(-8.49804474355533,1.18462061611618,6.21180992835903));
#23178=CARTESIAN_POINT('Ctrl Pts',(-9.17475454711885,0.889175133368411,
6.24362461066226));
#23179=CARTESIAN_POINT('Ctrl Pts',(-9.64143292944961,0.31695535130891,6.27543929296551));
#23180=CARTESIAN_POINT('Ctrl Pts',(-9.56483372345286,-0.692791868328002,
6.31520764584455));
#23181=CARTESIAN_POINT('Ctrl Pts',(-8.49147006545099,-1.27023725786807,
6.36292966929943));
#23182=CARTESIAN_POINT('Ctrl Pts',(-7.42794252952587,-0.67967383658084,
6.41065169275427));
#23183=CARTESIAN_POINT('Ctrl Pts',(-7.34750194971839,0.534156994858903,
6.45837371620915));
#23184=CARTESIAN_POINT('Ctrl Pts',(-8.32765665896405,1.25862194650517,6.506095739664));
#23185=CARTESIAN_POINT('Ctrl Pts',(-9.27359363721055,0.89715255760802,6.54586409254306));
#23186=CARTESIAN_POINT('Ctrl Pts',(-9.59205391956505,0.230963965632939,
6.5776787748463));
#23187=CARTESIAN_POINT('Ctrl Pts',(-9.57058965043867,-0.507116976178952,
6.60949345714954));
#23188=CARTESIAN_POINT('Ctrl Pts',(-8.85200491848723,-1.22062441757679,
6.64926181002859));
#23189=CARTESIAN_POINT('Ctrl Pts',(-7.66245973772922,-0.955040187706783,
6.69698383348346));
#23190=CARTESIAN_POINT('Ctrl Pts',(-7.24455670919153,0.18741901636682,6.74470585693831));
#23191=CARTESIAN_POINT('Ctrl Pts',(-7.97790718835371,1.15801318951335,6.79242788039319));
#23192=CARTESIAN_POINT('Ctrl Pts',(-9.19315459354979,1.06459764271049,6.84014990384804));
#23193=CARTESIAN_POINT('Ctrl Pts',(-9.67202077022298,0.172328585328035,
6.87991825672709));
#23194=CARTESIAN_POINT('Ctrl Pts',(-9.47698425864094,-0.539840601498366,
6.91173293903033));
#23195=CARTESIAN_POINT('Ctrl Pts',(-8.97784102671058,-1.08397314558408,
6.94354762133358));
#23196=CARTESIAN_POINT('Ctrl Pts',(-7.96757605345196,-1.15341066952153,
6.98331597421262));
#23197=CARTESIAN_POINT('Ctrl Pts',(-7.24174472569243,-0.174267368536913,
7.03103799766749));
#23198=CARTESIAN_POINT('Ctrl Pts',(-7.67319115562676,0.963146343500352,
7.07876002112235));
#23199=CARTESIAN_POINT('Ctrl Pts',(-8.86282920540638,1.21734564473849,7.12648204457721));
#23200=CARTESIAN_POINT('Ctrl Pts',(-9.72074426707527,0.351589058172741,
7.17420406803208));
#23201=CARTESIAN_POINT('Ctrl Pts',(-9.49909556123563,-0.636504427851428,
7.21397242091113));
#23202=CARTESIAN_POINT('Ctrl Pts',(-8.88564125986018,-1.04747646052394,
7.24578710321437));
#23203=CARTESIAN_POINT('Ctrl Pts',(-8.15214807584167,-1.13239960526954,
7.27760178551761));
#23204=CARTESIAN_POINT('Ctrl Pts',(-7.34270032648874,-0.523916879967266,
7.31737013839667));
#23205=CARTESIAN_POINT('Ctrl Pts',(-7.43442080370642,0.691459635471147,
7.36509216185152));
#23206=CARTESIAN_POINT('Ctrl Pts',(-8.50488942279009,1.26934622450957,7.41281418530639));
#23207=CARTESIAN_POINT('Ctrl Pts',(-9.5708743944013,0.683230182643655,7.46053620876125));
#23208=CARTESIAN_POINT('Ctrl Pts',(-9.65322921746207,-0.53281685729308,
7.50825823221611));
#23209=CARTESIAN_POINT('Ctrl Pts',(-8.83911790121967,-1.13504575953026,
7.54802658509517));
#23210=CARTESIAN_POINT('Ctrl Pts',(-8.10630070797208,-1.04447450141926,
7.57984126739841));
#23211=CARTESIAN_POINT('Ctrl Pts',(-7.49603062788743,-0.628788777742681,
7.61165594970165));
#23212=CARTESIAN_POINT('Ctrl Pts',(-7.28200050464232,0.360982909197031,
7.65142430258071));
#23213=CARTESIAN_POINT('Ctrl Pts',(-8.14655966331663,1.2201046592259,7.69914632603555));
#23214=CARTESIAN_POINT('Ctrl Pts',(-9.33420412881433,0.956748250900423,
7.74686834949043));
#23215=CARTESIAN_POINT('Ctrl Pts',(-9.75687542788829,-0.183955456103537,
7.79459037294528));
#23216=CARTESIAN_POINT('Ctrl Pts',(-9.02352258302385,-1.157478093308,7.84231239640016));
#23217=CARTESIAN_POINT('Ctrl Pts',(-8.01382251646826,-1.08025982136799,
7.88208074927919));
#23218=CARTESIAN_POINT('Ctrl Pts',(-7.51888594635904,-0.532298159311594,
7.91389543158245));
#23219=CARTESIAN_POINT('Ctrl Pts',(-7.32934158139695,0.181352403097051,
7.94571011388567));
#23220=CARTESIAN_POINT('Ctrl Pts',(-7.81506734795048,1.06990592744422,7.98547846676475));
#23221=CARTESIAN_POINT('Ctrl Pts',(-9.03099833983435,1.1539567644209,8.03320049021958));
#23222=CARTESIAN_POINT('Ctrl Pts',(-9.7568498620581,0.177741858819174,8.08092251367447));
#23223=CARTESIAN_POINT('Ctrl Pts',(-9.33015803729021,-0.961464031663194,
8.12864453712933));
#23224=CARTESIAN_POINT('Ctrl Pts',(-8.13860216611695,-1.21787644574009,
8.17636656058419));
#23225=CARTESIAN_POINT('Ctrl Pts',(-7.42553542619493,-0.498854394380912,
8.21613491346323));
#23226=CARTESIAN_POINT('Ctrl Pts',(-7.40975777023888,0.239370000425714,
8.24794959576648));
#23227=CARTESIAN_POINT('Ctrl Pts',(-7.73334073953907,0.903085491802819,
8.27976427806972));
#23228=CARTESIAN_POINT('Ctrl Pts',(-8.68203431044009,1.2572569113934,8.31953263094878));
#23229=CARTESIAN_POINT('Ctrl Pts',(-9.65657885208541,0.525262610480109,
8.36725465440363));
#23230=CARTESIAN_POINT('Ctrl Pts',(-9.56678963438923,-0.687912509038488,
8.4149766778585));
#23231=CARTESIAN_POINT('Ctrl Pts',(-8.49874411665927,-1.27026527694677,
8.46269870131337));
#23232=CARTESIAN_POINT('Ctrl Pts',(-7.42986079315603,-0.684568118889016,
8.5104207247682));
#23233=CARTESIAN_POINT('Ctrl Pts',(-7.36104268004619,0.325739236934825,
8.5501890776473));
#23234=CARTESIAN_POINT('Ctrl Pts',(-7.83211544074118,0.894346874630846,
8.5820037599505));
#23235=CARTESIAN_POINT('Ctrl Pts',(-8.51108119571025,1.18457040071787,8.61381844225378));
#23236=CARTESIAN_POINT('Ctrl Pts',(-9.4602607554946,0.831703500582261,8.65358679513279));
#23237=CARTESIAN_POINT('Ctrl Pts',(-9.71833485487774,-0.359493577758626,
8.70130881858769));
#23238=CARTESIAN_POINT('Ctrl Pts',(-8.8566765445911,-1.21821409722202,8.74903084204253));
#23239=CARTESIAN_POINT('Ctrl Pts',(-7.66794243081652,-0.959820635652346,
8.7967528654974));
#23240=CARTESIAN_POINT('Ctrl Pts',(-7.24280517665126,0.182462619648683,
8.84447488895226));
#23241=CARTESIAN_POINT('Ctrl Pts',(-7.85178406346805,0.991537153505232,
8.88424324183131));
#23242=CARTESIAN_POINT('Ctrl Pts',(-8.58006239840726,1.11333558688276,8.91605792413455));
#23243=CARTESIAN_POINT('Ctrl Pts',(-9.28341964256379,0.888585106109975,
8.9478726064378));
#23244=CARTESIAN_POINT('Ctrl Pts',(-9.7703664594142,0.000700156646912752,
8.98764095931684));
#23245=CARTESIAN_POINT('Ctrl Pts',(-9.18616070697658,-1.06899903426569,
9.03536298277171));
#23246=CARTESIAN_POINT('Ctrl Pts',(-7.97268600802238,-1.15464440326732,
9.08308500622657));
#23247=CARTESIAN_POINT('Ctrl Pts',(-7.24276328418966,-0.181469808723208,
9.13080702968144));
#23248=CARTESIAN_POINT('Ctrl Pts',(-7.66862368739739,0.960544042856526,
9.17852905313629));
#23249=CARTESIAN_POINT('Ctrl Pts',(-8.65852641109519,1.17396729261957,9.21829740601534));
#23250=CARTESIAN_POINT('Ctrl Pts',(-9.2889794685506,0.789580594280234,9.2501120883186));
#23251=CARTESIAN_POINT('Ctrl Pts',(-9.67384621642015,0.159420473438413,
9.28192677062181));
#23252=CARTESIAN_POINT('Ctrl Pts',(-9.46117695097487,-0.830644509004026,
9.3216951235009));
#23253=CARTESIAN_POINT('Ctrl Pts',(-8.31948777127265,-1.25737456087654,
9.36941714695573));
#23254=CARTESIAN_POINT('Ctrl Pts',(-7.34575754060823,-0.528193230805871,
9.41713917041061));
#23255=CARTESIAN_POINT('Ctrl Pts',(-7.4304786871105,0.685346344802941,9.46486119386546));
#23256=CARTESIAN_POINT('Ctrl Pts',(-8.49973262930053,1.27036662422184,9.51258321732033));
#23257=CARTESIAN_POINT('Ctrl Pts',(-9.38798818610006,0.7840961729928,9.55235157019938));
#23258=CARTESIAN_POINT('Ctrl Pts',(-9.61327428745144,0.0809103056341308,
9.58416625250263));
#23259=CARTESIAN_POINT('Ctrl Pts',(-9.49203055537855,-0.64746058131023,
9.61598093480587));
#23260=CARTESIAN_POINT('Ctrl Pts',(-8.6834200621885,-1.25705549289229,9.65574928768491));
#23261=CARTESIAN_POINT('Ctrl Pts',(-7.5408133482771,-0.832788339385354,
9.70347131113979));
#23262=CARTESIAN_POINT('Ctrl Pts',(-7.28151460673084,0.355748633899845,
9.75119333459464));
#23263=CARTESIAN_POINT('Ctrl Pts',(-8.13957862728818,1.21806070667769,9.79891535804951));
#23264=CARTESIAN_POINT('Ctrl Pts',(-9.33097191264403,0.960893912885614,
9.84663738150436));
#23265=CARTESIAN_POINT('Ctrl Pts',(-9.6845616175819,0.0119833762775842,
9.88640573438342));
#23266=CARTESIAN_POINT('Ctrl Pts',(-9.3948552845635,-0.66720321967679,9.91822041668666));
#23267=CARTESIAN_POINT('Ctrl Pts',(-8.82660658674435,-1.13870890250777,
9.9500350989899));
#23268=CARTESIAN_POINT('Ctrl Pts',(-7.81624711119259,-1.07066027220188,
9.98980345186896));
#23269=CARTESIAN_POINT('Ctrl Pts',(-7.22973604796101,-0.002223333057961,
10.0375254753238));
#23270=CARTESIAN_POINT('Ctrl Pts',(-7.81127521001297,1.06626540213459,10.0852474987787));
#23271=CARTESIAN_POINT('Ctrl Pts',(-9.02438159307564,1.15697856328588,10.1329695222335));
#23272=CARTESIAN_POINT('Ctrl Pts',(-9.75711790712465,0.182991800391184,
10.1806915456884));
#23273=CARTESIAN_POINT('Ctrl Pts',(-9.40366912726124,-0.765971236790376,
10.2204598985675));
#23274=CARTESIAN_POINT('Ctrl Pts',(-8.74020027325655,-1.09005960634535,
10.2522745808707));
#23275=CARTESIAN_POINT('Ctrl Pts',(-8.00196407609283,-1.0748441959899,10.2840892631739));
#23276=CARTESIAN_POINT('Ctrl Pts',(-7.28239915263251,-0.362325279153768,
10.323857616053));
#23277=CARTESIAN_POINT('Ctrl Pts',(-7.53790398833915,0.829425533369869,
10.3715796395079));
#23278=CARTESIAN_POINT('Ctrl Pts',(-8.67678457453722,1.25698486798276,10.4193016629627));
#23279=CARTESIAN_POINT('Ctrl Pts',(-9.65355201469891,0.531877053879621,
10.4670236864176));
#23280=CARTESIAN_POINT('Ctrl Pts',(-9.57042727050285,-0.684117599530743,
10.5147457098724));
#23281=CARTESIAN_POINT('Ctrl Pts',(-8.68224393873985,-1.17051995879944,
10.5545140627515));
#23282=CARTESIAN_POINT('Ctrl Pts',(-7.96844922392633,-0.981519174093803,
10.5863287450547));
#23283=CARTESIAN_POINT('Ctrl Pts',(-7.42011077084954,-0.487000082053453,
10.618143427358));
#23284=CARTESIAN_POINT('Ctrl Pts',(-7.34212352097922,0.522640881250568,
10.657911780237));
#23285=CARTESIAN_POINT('Ctrl Pts',(-8.31508734504523,1.25673496056136,10.7056338036919));
#23286=CARTESIAN_POINT('Ctrl Pts',(-9.45611263301509,0.834932558426621,
10.7533558271467));
#23287=CARTESIAN_POINT('Ctrl Pts',(-9.72037348998793,-0.352510987054788,
10.8010778506016));
#23288=CARTESIAN_POINT('Ctrl Pts',(-8.86191044830422,-1.21772421296126,
10.8487998740565));
#23289=CARTESIAN_POINT('Ctrl Pts',(-7.87197604037941,-1.00444797441067,
10.8885682269355));
#23290=CARTESIAN_POINT('Ctrl Pts',(-7.45582564786067,-0.394494662819061,
10.9203829092388));
#23291=CARTESIAN_POINT('Ctrl Pts',(-7.36469629318614,0.338253337677466,
10.952197591542));
#23292=CARTESIAN_POINT('Ctrl Pts',(-7.96630498329803,1.15282308294524,10.9919659444211));
#23293=CARTESIAN_POINT('Ctrl Pts',(-9.18241439302195,1.07139444055684,11.0396879678759));
#23294=CARTESIAN_POINT('Ctrl Pts',(-9.76934213251881,0.00585617149158359,
11.0874099913308));
#23295=CARTESIAN_POINT('Ctrl Pts',(-9.19227099350598,-1.06505226285372,
11.1351320147856));
#23296=CARTESIAN_POINT('Ctrl Pts',(-7.97696468603363,-1.1576983595773,11.1828540382405));
#23297=CARTESIAN_POINT('Ctrl Pts',(-7.36786565157653,-0.348714273116267,
11.2226223911196));
#23298=CARTESIAN_POINT('Ctrl Pts',(-7.45223013401734,0.38484337670927,11.2544370734228));
#23299=CARTESIAN_POINT('Ctrl Pts',(-7.86273483295154,0.99861050165816,11.286251755726));
#23300=CARTESIAN_POINT('Ctrl Pts',(-8.85065922194766,1.22101168769465,11.3260201086051));
#23301=CARTESIAN_POINT('Ctrl Pts',(-9.71706895636918,0.363756245997238,
11.3737421320599));
#23302=CARTESIAN_POINT('Ctrl Pts',(-9.46377577222247,-0.826075060154299,
11.4214641555148));
#23303=CARTESIAN_POINT('Ctrl Pts',(-8.32669098511707,-1.25838763360895,
11.4691861789697));
#23304=CARTESIAN_POINT('Ctrl Pts',(-7.34699516580216,-0.533302244267042,
11.5169082024245));
#23305=CARTESIAN_POINT('Ctrl Pts',(-7.41566323903509,0.477015320482895,
11.5566765553036));
#23306=CARTESIAN_POINT('Ctrl Pts',(-7.95941547151687,0.976572825867565,
11.5884912376068));
#23307=CARTESIAN_POINT('Ctrl Pts',(-8.67143590952399,1.17215167793291,11.6203059199101));
#23308=CARTESIAN_POINT('Ctrl Pts',(-9.56406941865381,0.693965203529443,
11.6600742727891));
#23309=CARTESIAN_POINT('Ctrl Pts',(-9.65841048613898,-0.521210702751624,
11.707796296244));
#23310=CARTESIAN_POINT('Ctrl Pts',(-8.68837512347985,-1.25530018600567,
11.7555183196989));
#23311=CARTESIAN_POINT('Ctrl Pts',(-7.54559797052453,-0.838267390032985,
11.8032403431537));
#23312=CARTESIAN_POINT('Ctrl Pts',(-7.27910784504458,0.351075173420432,
11.8509623666086));
#23313=CARTESIAN_POINT('Ctrl Pts',(-7.99206779629669,1.07020311324363,11.8907307194876));
#23314=CARTESIAN_POINT('Ctrl Pts',(-8.73013217658673,1.09222950791386,11.9225454017909));
#23315=CARTESIAN_POINT('Ctrl Pts',(-9.39656311872312,0.77427669556865,11.9543600840941));
#23316=CARTESIAN_POINT('Ctrl Pts',(-9.75875284033654,-0.171384708677798,
11.9941284369732));
#23317=CARTESIAN_POINT('Ctrl Pts',(-9.03503459701296,-1.15209089531113,
12.041850460428));
#23318=CARTESIAN_POINT('Ctrl Pts',(-7.8211428530551,-1.07257480772847,12.0895724838829));
#23319=CARTESIAN_POINT('Ctrl Pts',(-7.22976960704087,-0.00949736081689754,
12.1372945073378));
#23320=CARTESIAN_POINT('Ctrl Pts',(-7.80639734178506,1.06430577558381,12.1850165307926));
#23321=CARTESIAN_POINT('Ctrl Pts',(-8.81608592964515,1.14167399560278,12.2247848836717));
#23322=CARTESIAN_POINT('Ctrl Pts',(-9.38866097389678,0.67543155843589,12.2565995659749));
#23323=CARTESIAN_POINT('Ctrl Pts',(-9.68462176169229,-0.00105303385171488,
12.2884142482782));
#23324=CARTESIAN_POINT('Ctrl Pts',(-9.33980261183377,-0.953185713584225,
12.3281826011572));
#23325=CARTESIAN_POINT('Ctrl Pts',(-8.15083289505076,-1.22133442753447,
12.3759046246121));
#23326=CARTESIAN_POINT('Ctrl Pts',(-7.28484893342126,-0.366976333738949,
12.4236266480669));
#23327=CARTESIAN_POINT('Ctrl Pts',(-7.53317012442289,0.823902568724695,
12.4713486715218));
#23328=CARTESIAN_POINT('Ctrl Pts',(-8.67181352813447,1.25869438029009,12.5190706949767));
#23329=CARTESIAN_POINT('Ctrl Pts',(-9.48601427144361,0.656586387054127,
12.5588390478557));
#23330=CARTESIAN_POINT('Ctrl Pts',(-9.61397344810094,-0.0706347901844313,
12.590653730159));
#23331=CARTESIAN_POINT('Ctrl Pts',(-9.39518516300458,-0.775869416262637,
12.6224684124622));
#23332=CARTESIAN_POINT('Ctrl Pts',(-8.51145418725852,-1.27031501330109,
12.6622367653413));
#23333=CARTESIAN_POINT('Ctrl Pts',(-7.43684783790457,-0.695185537314625,
12.7099587887961));
#23334=CARTESIAN_POINT('Ctrl Pts',(-7.34093308882888,0.517520665829057,
12.757680812251));
#23335=CARTESIAN_POINT('Ctrl Pts',(-8.30789378535402,1.25565546761602,12.8054028357058));
#23336=CARTESIAN_POINT('Ctrl Pts',(-9.45347176054575,0.839477833695256,
12.8531248591607));
#23337=CARTESIAN_POINT('Ctrl Pts',(-9.67526720411315,-0.148582724740579,
12.8928932120397));
#23338=CARTESIAN_POINT('Ctrl Pts',(-9.29623126434288,-0.782267147681163,
12.924707894343));
#23339=CARTESIAN_POINT('Ctrl Pts',(-8.66935174234859,-1.17245461085654,
12.9565225766462));
#23340=CARTESIAN_POINT('Ctrl Pts',(-7.67752192246292,-0.968174180297535,
12.9962909295253));
#23341=CARTESIAN_POINT('Ctrl Pts',(-7.24114239930117,0.169861685563191,
13.0440129529802));
#23342=CARTESIAN_POINT('Ctrl Pts',(-7.96205466597611,1.14972977770164,13.091734976435));
#23343=CARTESIAN_POINT('Ctrl Pts',(-9.1762679501323,1.07528466495317,13.1394569998899));
#23344=CARTESIAN_POINT('Ctrl Pts',(-9.77031884177337,0.0110214182135979,
13.1871790233447));
#23345=CARTESIAN_POINT('Ctrl Pts',(-9.29158517982126,-0.881318744974018,
13.2269473762238));
#23346=CARTESIAN_POINT('Ctrl Pts',(-8.59033162705337,-1.11254946578217,
13.258762058527));
#23347=CARTESIAN_POINT('Ctrl Pts',(-7.86096047197614,-0.997475969022965,
13.2905767408303));
#23348=CARTESIAN_POINT('Ctrl Pts',(-7.24454225832378,-0.194054864121289,
13.3303450937093));
#23349=CARTESIAN_POINT('Ctrl Pts',(-7.65912168086415,0.952102464794035,
13.3780671171642));
#23350=CARTESIAN_POINT('Ctrl Pts',(-8.84542102092192,1.22145325839232,13.425789140619));
#23351=CARTESIAN_POINT('Ctrl Pts',(-9.71496598037074,0.370719729177345,
13.4735111640739));
#23352=CARTESIAN_POINT('Ctrl Pts',(-9.46789392392579,-0.822807865453071,
13.5212331875287));
#23353=CARTESIAN_POINT('Ctrl Pts',(-8.52201063734719,-1.18441772994109,
13.5610015404078));
#23354=CARTESIAN_POINT('Ctrl Pts',(-7.84039592147494,-0.900471307844614,
13.592816222711));
#23355=CARTESIAN_POINT('Ctrl Pts',(-7.36409672760257,-0.336234416608623,
13.6246309050143));
#23356=CARTESIAN_POINT('Ctrl Pts',(-7.42358990565628,0.674664909580162,
13.6643992578934));
#23357=CARTESIAN_POINT('Ctrl Pts',(-8.48702355866553,1.2701996154266,13.7121212813482));
#23358=CARTESIAN_POINT('Ctrl Pts',(-9.56039692213696,0.697726387385763,
13.7598433048031));
#23359=CARTESIAN_POINT('Ctrl Pts',(-9.66137616386497,-0.514568612592982,
13.8075653282579));
#23360=CARTESIAN_POINT('Ctrl Pts',(-8.69362714602554,-1.25552377904438,
13.8552873517128));
#23361=CARTESIAN_POINT('Ctrl Pts',(-7.74170605534076,-0.910120937375022,
13.8950557045919));
#23362=CARTESIAN_POINT('Ctrl Pts',(-7.41201282369385,-0.249419367434961,
13.9268703868951));
#23363=CARTESIAN_POINT('Ctrl Pts',(-7.42097828489804,0.48891918094274,13.9586850691983));
#23364=CARTESIAN_POINT('Ctrl Pts',(-8.12738032545558,1.21449002036506,13.9984534220774));
#23365=CARTESIAN_POINT('Ctrl Pts',(-9.3212513654399,0.969082889036178,14.0461754455323));
#23366=CARTESIAN_POINT('Ctrl Pts',(-9.75843636599122,-0.166137463814466,
14.0938974689871));
#23367=CARTESIAN_POINT('Ctrl Pts',(-9.04162318026726,-1.14900817301567,
14.141619492442));
#23368=CARTESIAN_POINT('Ctrl Pts',(-7.8249684203312,-1.07618018838563,14.1893415158968));
#23369=CARTESIAN_POINT('Ctrl Pts',(-7.33106473546485,-0.192146232024756,
14.2291098687759));
#23370=CARTESIAN_POINT('Ctrl Pts',(-7.51401624895191,0.523222858185244,
14.2609245510791));
#23371=CARTESIAN_POINT('Ctrl Pts',(-8.00387576243607,1.07572792473592,14.2927392333824));
#23372=CARTESIAN_POINT('Ctrl Pts',(-9.01282036199793,1.16225931174772,14.3325075862614));
#23373=CARTESIAN_POINT('Ctrl Pts',(-9.75512458555882,0.195544689997601,
14.3802296097163));
#23374=CARTESIAN_POINT('Ctrl Pts',(-9.34299643880091,-0.949010404736995,
14.4279516331711));
#23375=CARTESIAN_POINT('Ctrl Pts',(-8.15783249325345,-1.2233138797493,14.475673656626));
#23376=CARTESIAN_POINT('Ctrl Pts',(-7.28538310678412,-0.372205902886431,
14.5233956800809));
#23377=CARTESIAN_POINT('Ctrl Pts',(-7.49027159406131,0.619498485376649,
14.5631640329599));
#23378=CARTESIAN_POINT('Ctrl Pts',(-8.09668020484303,1.04079741520829,14.5949787152632));
#23379=CARTESIAN_POINT('Ctrl Pts',(-8.82863051099968,1.13812644920796,14.6267933975664));
#23380=CARTESIAN_POINT('Ctrl Pts',(-9.64826387771769,0.543434907327214,
14.6665617504455));
#23381=CARTESIAN_POINT('Ctrl Pts',(-9.57713290565078,-0.673320246814625,
14.7142837739003));
#23382=CARTESIAN_POINT('Ctrl Pts',(-8.51660134601078,-1.26924707575363,
14.7620057973552));
#23383=CARTESIAN_POINT('Ctrl Pts',(-7.44084619358963,-0.701262194326865,
14.8097278208101));
#23384=CARTESIAN_POINT('Ctrl Pts',(-7.33791546196855,0.51321628861147,14.8574498442649));
#23385=CARTESIAN_POINT('Ctrl Pts',(-8.14171434546497,1.12914180496267,14.897218197144));
#23386=CARTESIAN_POINT('Ctrl Pts',(-8.87595988159389,1.05099014478143,14.9290328794472));
#23387=CARTESIAN_POINT('Ctrl Pts',(-9.49318006986067,0.645695886996565,
14.9608475617504));
#23388=CARTESIAN_POINT('Ctrl Pts',(-9.72393637462547,-0.340310403119495,
15.0006159146295));
#23389=CARTESIAN_POINT('Ctrl Pts',(-8.87404609450619,-1.21394603873967,
15.0483379380843));
#23390=CARTESIAN_POINT('Ctrl Pts',(-7.68211319459765,-0.970734219451872,
15.0960599615392));
#23391=CARTESIAN_POINT('Ctrl Pts',(-7.24019036465419,0.162650140326822,
15.1437819849941));
#23392=CARTESIAN_POINT('Ctrl Pts',(-7.95695626426865,1.14844897424003,15.1915040084489));
#23393=CARTESIAN_POINT('Ctrl Pts',(-8.9678190573545,1.08833594701761,15.231272361328));
#23394=CARTESIAN_POINT('Ctrl Pts',(-9.47196150163588,0.548832220338601,
15.2630870436313));
#23395=CARTESIAN_POINT('Ctrl Pts',(-9.67356121121295,-0.161507282602432,
15.2949017259345));
#23396=CARTESIAN_POINT('Ctrl Pts',(-9.20294744217587,-1.05815633227,15.3346700788135));
#23397=CARTESIAN_POINT('Ctrl Pts',(-7.98861526120894,-1.16278173533498,
15.3823921022684));
#23398=CARTESIAN_POINT('Ctrl Pts',(-7.24633766496125,-0.198993896651544,
15.4301141257232));
#23399=CARTESIAN_POINT('Ctrl Pts',(-7.65368670603976,0.947269754286983,
15.4778361491781));
#23400=CARTESIAN_POINT('Ctrl Pts',(-8.84072065488431,1.22382409746114,15.525558172633));
#23401=CARTESIAN_POINT('Ctrl Pts',(-9.56587666344393,0.516967103108893,
15.565326525512));
#23402=CARTESIAN_POINT('Ctrl Pts',(-9.59412288800059,-0.220869169870519,
15.5971412078153));
#23403=CARTESIAN_POINT('Ctrl Pts',(-9.28187668594746,-0.889997654174282,
15.6289558901185));
#23404=CARTESIAN_POINT('Ctrl Pts',(-8.3391963985811,-1.26011363586197,15.6687242429976));
#23405=CARTESIAN_POINT('Ctrl Pts',(-7.35261511400304,-0.544843601675332,
15.7164462664524));
#23406=CARTESIAN_POINT('Ctrl Pts',(-7.42146958197941,0.669890693554228,
15.7641682899073));
#23407=CARTESIAN_POINT('Ctrl Pts',(-8.48021464548925,1.26984600438468,15.8118903133622));
#23408=CARTESIAN_POINT('Ctrl Pts',(-9.55750298236283,0.703085044786402,
15.859612336817));
#23409=CARTESIAN_POINT('Ctrl Pts',(-9.66331880274563,-0.509245030498203,
15.9073343602719));
#23410=CARTESIAN_POINT('Ctrl Pts',(-8.70050979592311,-1.25407183081503,
15.9550563837268));
#23411=CARTESIAN_POINT('Ctrl Pts',(-7.55383452636763,-0.846612249150831,
16.0027784071816));
#23412=CARTESIAN_POINT('Ctrl Pts',(-7.27557316343251,0.33782473088005,16.0505004306365));
#23413=CARTESIAN_POINT('Ctrl Pts',(-8.1233181103483,1.21320028335102,16.0982224540913));
#23414=CARTESIAN_POINT('Ctrl Pts',(-9.1158648858804,1.01199674841544,16.1379908069704));
#23415=CARTESIAN_POINT('Ctrl Pts',(-9.53931342581282,0.407081917028108,
16.1698054892736));
#23416=CARTESIAN_POINT('Ctrl Pts',(-9.63932163954313,-0.324490753396568,
16.2016201715769));
#23417=CARTESIAN_POINT('Ctrl Pts',(-9.04759131286806,-1.14628955341257,
16.2413885244559));
#23418=CARTESIAN_POINT('Ctrl Pts',(-7.8305950534041,-1.07956620750823,16.2891105479108));
#23419=CARTESIAN_POINT('Ctrl Pts',(-7.2308199229778,-0.0212073876117485,
16.3368325713657));
#23420=CARTESIAN_POINT('Ctrl Pts',(-7.79490064728529,1.05660333990498,16.3845545948205));
#23421=CARTESIAN_POINT('Ctrl Pts',(-9.00899631826399,1.16393843392956,16.4322766182754));
#23422=CARTESIAN_POINT('Ctrl Pts',(-9.62783474663535,0.362380053368341,
16.4720449711544));
#23423=CARTESIAN_POINT('Ctrl Pts',(-9.55234712077239,-0.372144466768089,
16.5038596534577));
#23424=CARTESIAN_POINT('Ctrl Pts',(-9.14929499916242,-0.990830867533636,
16.5356743357609));
#23425=CARTESIAN_POINT('Ctrl Pts',(-8.16413226770568,-1.22516301435909,
16.5754426886399));
#23426=CARTESIAN_POINT('Ctrl Pts',(-7.28741902604588,-0.378447839289557,
16.6231647120948));
#23427=CARTESIAN_POINT('Ctrl Pts',(-7.52630483397695,0.814359548927526,
16.6708867355497));
#23428=CARTESIAN_POINT('Ctrl Pts',(-8.65807846404219,1.26039147291354,16.7186087590046));
#23429=CARTESIAN_POINT('Ctrl Pts',(-9.64647120733396,0.54720671629367,16.7663307824594));
#23430=CARTESIAN_POINT('Ctrl Pts',(-9.59002609357546,-0.463867378651884,
16.8060991353385));
#23431=CARTESIAN_POINT('Ctrl Pts',(-9.0523548496622,-0.969964039050123,
16.8379138176417));
#23432=CARTESIAN_POINT('Ctrl Pts',(-8.34275164585083,-1.17413916597537,
16.869728499945));
#23433=CARTESIAN_POINT('Ctrl Pts',(-7.44440062377225,-0.706782420080965,
16.909496852824));
#23434=CARTESIAN_POINT('Ctrl Pts',(-7.33537113793291,0.507163745220385,
16.9572188762789));
#23435=CARTESIAN_POINT('Ctrl Pts',(-8.29645810449297,1.25293034154812,17.0049408997337));
#23436=CARTESIAN_POINT('Ctrl Pts',(-9.44419493667808,0.849747828922038,
17.0526629231886));
#23437=CARTESIAN_POINT('Ctrl Pts',(-9.72504848574826,-0.336285056074205,
17.1003849466434));
#23438=CARTESIAN_POINT('Ctrl Pts',(-9.02083719942392,-1.0639823489339,17.1401532995225));
#23439=CARTESIAN_POINT('Ctrl Pts',(-8.28309315876083,-1.09493266409099,
17.1719679818257));
#23440=CARTESIAN_POINT('Ctrl Pts',(-7.61286589490514,-0.785062358491983,
17.203782664129));
#23441=CARTESIAN_POINT('Ctrl Pts',(-7.23926662306685,0.156149875810646,
17.243551017008));
#23442=CARTESIAN_POINT('Ctrl Pts',(-7.95107210703395,1.14553638937586,17.2912730404629));
#23443=CARTESIAN_POINT('Ctrl Pts',(-9.16583668605209,1.08070590432238,17.3389950639178));
#23444=CARTESIAN_POINT('Ctrl Pts',(-9.77002265432594,0.024857766580027,
17.3867170873726));
#23445=CARTESIAN_POINT('Ctrl Pts',(-9.20642275932966,-1.05584009988493,
17.4344391108275));
#23446=CARTESIAN_POINT('Ctrl Pts',(-8.19774363120575,-1.14541298869811,
17.4742074637065));
#23447=CARTESIAN_POINT('Ctrl Pts',(-7.61957211175687,-0.686128887500105,
17.5060221460098));
#23448=CARTESIAN_POINT('Ctrl Pts',(-7.31545212919699,-0.013272864473688,
17.537836828313));
#23449=CARTESIAN_POINT('Ctrl Pts',(-7.64873177068013,0.942960144001058,
17.5776051811921));
#23450=CARTESIAN_POINT('Ctrl Pts',(-8.83437177863538,1.22546765143426,17.6253272046469));
#23451=CARTESIAN_POINT('Ctrl Pts',(-9.7106243049545,0.38164451572817,17.6730492281018));
#23452=CARTESIAN_POINT('Ctrl Pts',(-9.47672276235654,-0.812150291851311,
17.7207712515566));
#23453=CARTESIAN_POINT('Ctrl Pts',(-8.34342062912157,-1.26068010694196,
17.7684932750115));
#23454=CARTESIAN_POINT('Ctrl Pts',(-7.52199803547846,-0.668462403241392,
17.8082616278906));
#23455=CARTESIAN_POINT('Ctrl Pts',(-7.38525381327406,0.0571581651059841,
17.8400763101938));
#23456=CARTESIAN_POINT('Ctrl Pts',(-7.59549758383178,0.764987062832501,
17.8718909924971));
#23457=CARTESIAN_POINT('Ctrl Pts',(-8.47318452674403,1.27008360426311,17.9116593453761));
#23458=CARTESIAN_POINT('Ctrl Pts',(-9.55466742874301,0.707991571848307,
17.959381368831));
#23459=CARTESIAN_POINT('Ctrl Pts',(-9.66524061504402,-0.50346603975217,
18.0071033922858));
#23460=CARTESIAN_POINT('Ctrl Pts',(-8.70727701023286,-1.25324047656007,
18.0548254157407));
#23461=CARTESIAN_POINT('Ctrl Pts',(-7.55674990236037,-0.850946934142607,
18.1025474391955));
#23462=CARTESIAN_POINT('Ctrl Pts',(-7.32302190246604,0.134359164483167,
18.1423157920746));
#23463=CARTESIAN_POINT('Ctrl Pts',(-7.69436687770133,0.772580991814832,
18.1741304743778));
#23464=CARTESIAN_POINT('Ctrl Pts',(-8.31648195947549,1.17032087734831,18.2059451566811));
#23465=CARTESIAN_POINT('Ctrl Pts',(-9.31070964793652,0.978049742173947,
18.2457135095601));
#23466=CARTESIAN_POINT('Ctrl Pts',(-9.76081971146936,-0.154625697184869,
18.293435533015));
#23467=CARTESIAN_POINT('Ctrl Pts',(-9.05180986375601,-1.14314024441165,
18.3411575564698));
#23468=CARTESIAN_POINT('Ctrl Pts',(-7.83678509216389,-1.0833842518163,18.3888795799247));
#23469=CARTESIAN_POINT('Ctrl Pts',(-7.22990733399897,-0.0263827821555435,
18.4366016033796));
#23470=CARTESIAN_POINT('Ctrl Pts',(-7.69781477559553,0.871681531812165,
18.4763699562586));
#23471=CARTESIAN_POINT('Ctrl Pts',(-8.39622073897505,1.11137571578626,18.5081846385619));
#23472=CARTESIAN_POINT('Ctrl Pts',(-9.12693016111688,1.00513103635158,18.5399993208651));
#23473=CARTESIAN_POINT('Ctrl Pts',(-9.75301919974774,0.209223126081749,
18.5797676737442));
#23474=CARTESIAN_POINT('Ctrl Pts',(-9.35233075805922,-0.941863965722109,
18.627489697199));
#23475=CARTESIAN_POINT('Ctrl Pts',(-8.16937546850047,-1.2255411716065,18.6752117206539));
#23476=CARTESIAN_POINT('Ctrl Pts',(-7.28960603720165,-0.385385399153776,
18.7229337441087));
#23477=CARTESIAN_POINT('Ctrl Pts',(-7.52222650552583,0.811042800922165,
18.7706557675636));
#23478=CARTESIAN_POINT('Ctrl Pts',(-8.4636676182458,1.18406494128967,18.8104241204426));
#23479=CARTESIAN_POINT('Ctrl Pts',(-9.14866630079203,0.90838215904711,18.8422388027459));
#23480=CARTESIAN_POINT('Ctrl Pts',(-9.63175407270726,0.34994649028926,18.8740534850491));
#23481=CARTESIAN_POINT('Ctrl Pts',(-9.5844902130829,-0.661598374507747,
18.9138218379282));
#23482=CARTESIAN_POINT('Ctrl Pts',(-8.52833622049212,-1.26994980596393,
18.9615438613831));
#23483=CARTESIAN_POINT('Ctrl Pts',(-7.44811833664692,-0.710498916560375,
19.0092658848379));
#23484=CARTESIAN_POINT('Ctrl Pts',(-7.33248600078022,0.500486276220874,
19.0569879082928));
#23485=CARTESIAN_POINT('Ctrl Pts',(-8.29120376213664,1.25309040475059,19.1047099317477));
#23486=CARTESIAN_POINT('Ctrl Pts',(-9.24723225571495,0.9192245553587,19.1444782846267));
#23487=CARTESIAN_POINT('Ctrl Pts',(-9.58489134881782,0.262558332411264,
19.17629296693));
#23488=CARTESIAN_POINT('Ctrl Pts',(-9.58485538992238,-0.475834645766379,
19.2081076492332));
#23489=CARTESIAN_POINT('Ctrl Pts',(-8.8872794497266,-1.20989506125256,19.2478760021122));
#23490=CARTESIAN_POINT('Ctrl Pts',(-7.6905279636182,-0.978943549636808,
19.2955980255671));
#23491=CARTESIAN_POINT('Ctrl Pts',(-7.23964653004754,0.150906841828665,
19.343320049022));
#23492=CARTESIAN_POINT('Ctrl Pts',(-7.94452128542435,1.14237421570735,19.3910420724768));
#23493=CARTESIAN_POINT('Ctrl Pts',(-9.16196779807331,1.08426475813698,19.4387640959317));
#23494=CARTESIAN_POINT('Ctrl Pts',(-9.66652613095242,0.206268303334325,
19.4785324488107));
#23495=CARTESIAN_POINT('Ctrl Pts',(-9.49223906914536,-0.511260937604133,
19.510347131114));
#23496=CARTESIAN_POINT('Ctrl Pts',(-9.00909690916197,-1.06964955206693,
19.5421618134172));
#23497=CARTESIAN_POINT('Ctrl Pts',(-8.00127252658247,-1.16837594064688,
19.5819301662963));
#23498=CARTESIAN_POINT('Ctrl Pts',(-7.24733194871174,-0.210708814104341,
19.6296521897511));
#23499=CARTESIAN_POINT('Ctrl Pts',(-7.64558866994153,0.938746517010665,
19.677374213206));
#23500=CARTESIAN_POINT('Ctrl Pts',(-8.82734875444545,1.22736231163525,19.7250962366608));
#23501=CARTESIAN_POINT('Ctrl Pts',(-9.71002692863045,0.386867242620788,
19.7728182601158));
#23502=CARTESIAN_POINT('Ctrl Pts',(-9.51714626434415,-0.607242376721195,
19.8125866129947));
#23503=CARTESIAN_POINT('Ctrl Pts',(-8.91587683280376,-1.03584389586241,
19.8444012952981));
#23504=CARTESIAN_POINT('Ctrl Pts',(-8.18515706613851,-1.1420174053633,19.8762159776012));
#23505=CARTESIAN_POINT('Ctrl Pts',(-7.35839193464024,-0.557281308254152,
19.9159843304804));
#23506=CARTESIAN_POINT('Ctrl Pts',(-7.41480328973932,0.660245068969852,
19.9637063539351));
#23507=CARTESIAN_POINT('Ctrl Pts',(-8.46805065902489,1.26895349944085,20.0114283773901));
#23508=CARTESIAN_POINT('Ctrl Pts',(-9.5505958796237,0.714019431652471,20.0591504008449));
#23509=CARTESIAN_POINT('Ctrl Pts',(-9.6682059673661,-0.499125484456667,
20.1068724242998));
#23510=CARTESIAN_POINT('Ctrl Pts',(-8.87191434881798,-1.12472643087044,
20.1466407771788));
#23511=CARTESIAN_POINT('Ctrl Pts',(-8.13677740234172,-1.05545983401012,
20.1784554594821));
#23512=CARTESIAN_POINT('Ctrl Pts',(-7.51470106247534,-0.657659357774231,
20.2102701417853));
#23513=CARTESIAN_POINT('Ctrl Pts',(-7.27203769305019,0.325484260962615,
20.2500384946644));
#23514=CARTESIAN_POINT('Ctrl Pts',(-8.11130082014058,1.20933386566167,20.2977605181192));
#23515=CARTESIAN_POINT('Ctrl Pts',(-9.30608773965546,0.980554078115584,
20.3454825415741));
#23516=CARTESIAN_POINT('Ctrl Pts',(-9.76168449057688,-0.147403179400575,
20.3932045650289));
#23517=CARTESIAN_POINT('Ctrl Pts',(-9.05689235516024,-1.14179785259385,
20.4409265884838));
#23518=CARTESIAN_POINT('Ctrl Pts',(-8.04537665815608,-1.09391381936874,
20.4806949413629));
#23519=CARTESIAN_POINT('Ctrl Pts',(-7.53474657604769,-0.560546112471273,
20.5125096236661));
#23520=CARTESIAN_POINT('Ctrl Pts',(-7.32457174740621,0.147303259161259,
20.5443243059694));
#23521=CARTESIAN_POINT('Ctrl Pts',(-7.78430692110201,1.04957841452719,20.5840926588484));
#23522=CARTESIAN_POINT('Ctrl Pts',(-8.99728661934093,1.16888043412664,20.6318146823032));
#23523=CARTESIAN_POINT('Ctrl Pts',(-9.7511624004973,0.214141055647227,20.6795367057581));
#23524=CARTESIAN_POINT('Ctrl Pts',(-9.35771029132173,-0.936967719412176,
20.727258729213));
#23525=CARTESIAN_POINT('Ctrl Pts',(-8.17409741818057,-1.22785135036264,
20.7749807526679));
#23526=CARTESIAN_POINT('Ctrl Pts',(-7.440464827453,-0.529825485694162,20.8147491055469));
#23527=CARTESIAN_POINT('Ctrl Pts',(-7.40327038360504,0.207630116265646,
20.8465637878501));
#23528=CARTESIAN_POINT('Ctrl Pts',(-7.70745589936328,0.880456515508389,
20.8783784701534));
#23529=CARTESIAN_POINT('Ctrl Pts',(-8.6454717721415,1.26201006134416,20.9181468230324));
#23530=CARTESIAN_POINT('Ctrl Pts',(-9.64084849413286,0.55860555358354,20.9658688464873));
#23531=CARTESIAN_POINT('Ctrl Pts',(-9.58630370016657,-0.65666430932124,
21.0135908699422));
#23532=CARTESIAN_POINT('Ctrl Pts',(-8.53560802117004,-1.2697667186881,21.061312893397));
#23533=CARTESIAN_POINT('Ctrl Pts',(-7.45017782549272,-0.715335469088922,
21.1090349168518));
#23534=CARTESIAN_POINT('Ctrl Pts',(-7.35206935690855,0.29254925364273,21.1488032697309));
#23535=CARTESIAN_POINT('Ctrl Pts',(-7.8064425956856,0.87458804221129,21.1806179520342));
#23536=CARTESIAN_POINT('Ctrl Pts',(-8.47670003703183,1.18439306772749,21.2124326343374));
#23537=CARTESIAN_POINT('Ctrl Pts',(-9.43572010035171,0.859220184365848,
21.2522009872165));
#23538=CARTESIAN_POINT('Ctrl Pts',(-9.72825430450134,-0.323985824587268,
21.2999230106713));
#23539=CARTESIAN_POINT('Ctrl Pts',(-8.89187916023458,-1.20735018445592,
21.3476450341262));
#23540=CARTESIAN_POINT('Ctrl Pts',(-7.69614707717368,-0.983562875226182,
21.395367057581));
#23541=CARTESIAN_POINT('Ctrl Pts',(-7.23803957092387,0.145901702765443,
21.4430890810359));
#23542=CARTESIAN_POINT('Ctrl Pts',(-7.8232824513717,0.97230817467188,21.4828574339149));
#23543=CARTESIAN_POINT('Ctrl Pts',(-8.54771943639906,1.11519010578827,21.5146721162182));
#23544=CARTESIAN_POINT('Ctrl Pts',(-9.25730275191042,0.910945865078809,
21.5464867985214));
#23545=CARTESIAN_POINT('Ctrl Pts',(-9.76981109383267,0.0375661736593354,
21.5862551514005));
#23546=CARTESIAN_POINT('Ctrl Pts',(-9.21689429836074,-1.04863626488762,
21.6339771748553));
#23547=CARTESIAN_POINT('Ctrl Pts',(-8.00641613218915,-1.16946086277772,
21.6816991983102));
#23548=CARTESIAN_POINT('Ctrl Pts',(-7.24855909460346,-0.217878662011405,
21.7294212217651));
#23549=CARTESIAN_POINT('Ctrl Pts',(-7.64109864474925,0.936012763466559,
21.7771432452199));
#23550=CARTESIAN_POINT('Ctrl Pts',(-8.62439085665566,1.17807331772505,21.816911598099));
#23551=CARTESIAN_POINT('Ctrl Pts',(-9.26573336877662,0.812144398860403,
21.8487262804022));
#23552=CARTESIAN_POINT('Ctrl Pts',(-9.66872540454101,0.193418602868739,
21.8805409627055));
#23553=CARTESIAN_POINT('Ctrl Pts',(-9.48487761198751,-0.802401097226132,
21.9203093155845));
#23554=CARTESIAN_POINT('Ctrl Pts',(-8.3560530827218,-1.26208349013278,21.9680313390394));
#23555=CARTESIAN_POINT('Ctrl Pts',(-7.36157196177148,-0.561467136978719,
22.0157533624943));
#23556=CARTESIAN_POINT('Ctrl Pts',(-7.41104024249466,0.654019951984267,
22.0634753859491));
#23557=CARTESIAN_POINT('Ctrl Pts',(-8.46286642522661,1.26982381811353,22.111197409404));
#23558=CARTESIAN_POINT('Ctrl Pts',(-9.36485954540964,0.809535542066614,
22.150965762283));
#23559=CARTESIAN_POINT('Ctrl Pts',(-9.61045736917226,0.113183691004152,
22.1827804445863));
#23560=CARTESIAN_POINT('Ctrl Pts',(-9.510402184057,-0.6183989437314,22.2145951268895));
#23561=CARTESIAN_POINT('Ctrl Pts',(-8.71982283494963,-1.25120316202389,
22.2543634797686));
#23562=CARTESIAN_POINT('Ctrl Pts',(-7.56538503329298,-0.860273395535878,
22.3020855032234));
#23563=CARTESIAN_POINT('Ctrl Pts',(-7.27170389959832,0.320238089349084,
22.3498075266783));
#23564=CARTESIAN_POINT('Ctrl Pts',(-8.10438204030062,1.20708818278655,22.3975295501332));
#23565=CARTESIAN_POINT('Ctrl Pts',(-9.30273657679897,0.984604194431938,
22.445251573588));
#23566=CARTESIAN_POINT('Ctrl Pts',(-9.68371494937798,0.0463545658411376,
22.485019926467));
#23567=CARTESIAN_POINT('Ctrl Pts',(-9.41384077673285,-0.640953314554658,
22.5168346087703));
#23568=CARTESIAN_POINT('Ctrl Pts',(-8.85951460900709,-1.12875111209944,
22.5486492910735));
#23569=CARTESIAN_POINT('Ctrl Pts',(-7.8476058857349,-1.09005199467554,22.5884176439526));
#23570=CARTESIAN_POINT('Ctrl Pts',(-7.23033557328084,-0.0390857337598358,
22.6361396674074));
#23571=CARTESIAN_POINT('Ctrl Pts',(-7.78062202915808,1.04582937384607,22.6838616908624));
#23572=CARTESIAN_POINT('Ctrl Pts',(-8.99058496612945,1.17170894084981,22.7315837143172));
#23573=CARTESIAN_POINT('Ctrl Pts',(-9.75127797821979,0.219396564800193,
22.7793057377721));
#23574=CARTESIAN_POINT('Ctrl Pts',(-9.42551717667043,-0.739423953387505,
22.8190740906511));
#23575=CARTESIAN_POINT('Ctrl Pts',(-8.77173287452605,-1.08262983589042,
22.8508887729544));
#23576=CARTESIAN_POINT('Ctrl Pts',(-8.03336604963158,-1.08884460944564,
22.8827034552576));
#23577=CARTESIAN_POINT('Ctrl Pts',(-7.29342673462276,-0.397507719045549,
22.9224718081366));
#23578=CARTESIAN_POINT('Ctrl Pts',(-7.51423908935107,0.801155963652635,
22.9701938315915));
#23579=CARTESIAN_POINT('Ctrl Pts',(-8.64023214205648,1.26158578402983,23.0179158550463));
#23580=CARTESIAN_POINT('Ctrl Pts',(-9.63763097898426,0.565129371661826,
23.0656378785012));
#23581=CARTESIAN_POINT('Ctrl Pts',(-9.58982967509586,-0.652765433141446,
23.1133599019561));
#23582=CARTESIAN_POINT('Ctrl Pts',(-8.71613592676988,-1.16473820591349,
23.1531282548351));
#23583=CARTESIAN_POINT('Ctrl Pts',(-7.99715700058761,-0.996531502061154,
23.1849429371384));
#23584=CARTESIAN_POINT('Ctrl Pts',(-7.43469844210718,-0.518133590791431,
23.2167576194416));
#23585=CARTESIAN_POINT('Ctrl Pts',(-7.32744403743226,0.488818929738514,
23.2565259723207));
#23586=CARTESIAN_POINT('Ctrl Pts',(-8.27869450284539,1.25083944932543,23.3042479957755));
#23587=CARTESIAN_POINT('Ctrl Pts',(-9.43148001699525,0.862327502791391,
23.3519700192304));
#23588=CARTESIAN_POINT('Ctrl Pts',(-9.73008944468282,-0.316947013141832,
23.3996920426852));
#23589=CARTESIAN_POINT('Ctrl Pts',(-8.89709664300896,-1.20670861749425,
23.4474140661402));
#23590=CARTESIAN_POINT('Ctrl Pts',(-7.90138984794499,-1.02225031817649,
23.4871824190191));
#23591=CARTESIAN_POINT('Ctrl Pts',(-7.46771374944203,-0.424630679022691,
23.5189971013225));
#23592=CARTESIAN_POINT('Ctrl Pts',(-7.35535826930249,0.305164112406859,
23.5508117836256));
#23593=CARTESIAN_POINT('Ctrl Pts',(-7.93307458495534,1.13684959656076,23.5905801365048));
#23594=CARTESIAN_POINT('Ctrl Pts',(-9.15103487649505,1.09074701037714,23.6383021599595));
#23595=CARTESIAN_POINT('Ctrl Pts',(-9.76863756968231,0.0426902907282275,
23.6860241834145));
#23596=CARTESIAN_POINT('Ctrl Pts',(-9.22288747522111,-1.04451383390937,
23.7337462068693));
#23597=CARTESIAN_POINT('Ctrl Pts',(-8.01078163460585,-1.17238936466728,
23.7814682303242));
#23598=CARTESIAN_POINT('Ctrl Pts',(-7.3784622428289,-0.381422189174766,
23.8212365832032));
#23599=CARTESIAN_POINT('Ctrl Pts',(-7.44150318994769,0.354274780032955,
23.8530512655065));
#23600=CARTESIAN_POINT('Ctrl Pts',(-7.83402333855529,0.979696337426145,
23.8848659478097));
#23601=CARTESIAN_POINT('Ctrl Pts',(-8.81507750731556,1.23067363496897,23.9246343006888));
#23602=CARTESIAN_POINT('Ctrl Pts',(-9.70600007142817,0.398922647608368,
23.9723563241436));
#23603=CARTESIAN_POINT('Ctrl Pts',(-9.48734273227305,-0.797758154555304,
24.0200783475985));
#23604=CARTESIAN_POINT('Ctrl Pts',(-8.3632826623428,-1.2628870973462,24.0678003710533));
#23605=CARTESIAN_POINT('Ctrl Pts',(-7.36295733039398,-0.566538082496778,
24.1155223945082));
#23606=CARTESIAN_POINT('Ctrl Pts',(-7.40227684611156,0.445346723994319,
24.1552907473872));
#23607=CARTESIAN_POINT('Ctrl Pts',(-7.93130279579168,0.960473636589752,
24.1871054296905));
#23608=CARTESIAN_POINT('Ctrl Pts',(-8.63734760745799,1.17663310419213,24.2189201119937));
#23609=CARTESIAN_POINT('Ctrl Pts',(-9.54348223731444,0.724552449332103,
24.2586884648728));
#23610=CARTESIAN_POINT('Ctrl Pts',(-9.67304824068325,-0.487373856592171,
24.3064104883276));
#23611=CARTESIAN_POINT('Ctrl Pts',(-8.72472486990299,-1.24930479746899,
24.3541325117826));
#23612=CARTESIAN_POINT('Ctrl Pts',(-7.57032664362157,-0.865611287761247,
24.4018545352373));
#23613=CARTESIAN_POINT('Ctrl Pts',(-7.26943377642353,0.315496752466079,
24.4495765586923));
#23614=CARTESIAN_POINT('Ctrl Pts',(-7.96122419684737,1.05501206679947,24.4893449115713));
#23615=CARTESIAN_POINT('Ctrl Pts',(-8.69833851192349,1.09844797389147,24.5211595938745));
#23616=CARTESIAN_POINT('Ctrl Pts',(-9.37371582986139,0.79996904677923,24.5529742761777));
#23617=CARTESIAN_POINT('Ctrl Pts',(-9.76319630647174,-0.134783243543247,
24.5927426290568));
#23618=CARTESIAN_POINT('Ctrl Pts',(-9.06824318291268,-1.13607884239293,
24.6404646525116));
#23619=CARTESIAN_POINT('Ctrl Pts',(-7.85255512587106,-1.09182364834989,
24.6881866759666));
#23620=CARTESIAN_POINT('Ctrl Pts',(-7.23058021209953,-0.0463557239866595,
24.7359086994214));
#23621=CARTESIAN_POINT('Ctrl Pts',(-7.77580308415762,1.04372901584095,24.7836307228763));
#23622=CARTESIAN_POINT('Ctrl Pts',(-8.78282117356678,1.1503660334596,24.8233990757553));
#23623=CARTESIAN_POINT('Ctrl Pts',(-9.36868552067456,0.700936218802155,
24.8552137580586));
#23624=CARTESIAN_POINT('Ctrl Pts',(-9.68415338762423,0.0333253917200288,
24.8870284403618));
#23625=CARTESIAN_POINT('Ctrl Pts',(-9.36711056521203,-0.92841300029759,
24.9267967932409));
#23626=CARTESIAN_POINT('Ctrl Pts',(-8.18642334722071,-1.23095293731781,
24.9745188166957));
#23627=CARTESIAN_POINT('Ctrl Pts',(-7.29601045824367,-0.402085721548624,
25.0222408401506));
#23628=CARTESIAN_POINT('Ctrl Pts',(-7.50966749686034,0.795497947379344,
25.0699628636054));
#23629=CARTESIAN_POINT('Ctrl Pts',(-8.63521357891507,1.26315031548144,25.1176848870603));
#23630=CARTESIAN_POINT('Ctrl Pts',(-9.46654470641044,0.684924198481284,
25.1574532399394));
#23631=CARTESIAN_POINT('Ctrl Pts',(-9.61555410710697,-0.0382772879795426,
25.1892679222426));
#23632=CARTESIAN_POINT('Ctrl Pts',(-9.41732403297787,-0.749564170486076,
25.2210826045458));
#23633=CARTESIAN_POINT('Ctrl Pts',(-8.54831418196222,-1.26944758507203,
25.2608509574249));
#23634=CARTESIAN_POINT('Ctrl Pts',(-7.45747004727097,-0.725745650157399,
25.3085729808797));
#23635=CARTESIAN_POINT('Ctrl Pts',(-7.3264026964314,0.483666324224087,25.3562950043346));
#23636=CARTESIAN_POINT('Ctrl Pts',(-8.2715353000242,1.24955165236358,25.4040170277895));
#23637=CARTESIAN_POINT('Ctrl Pts',(-9.42870835191566,0.86679422500728,25.4517390512443));
#23638=CARTESIAN_POINT('Ctrl Pts',(-9.67908411377995,-0.114413634620136,
25.4915074041234));
#23639=CARTESIAN_POINT('Ctrl Pts',(-9.31859747480905,-0.758830871073753,
25.5233220864267));
#23640=CARTESIAN_POINT('Ctrl Pts',(-8.70330530427728,-1.16704617749599,
25.5551367687298));
#23641=CARTESIAN_POINT('Ctrl Pts',(-7.70596495586421,-0.991634902627059,
25.5949051216089));
#23642=CARTESIAN_POINT('Ctrl Pts',(-7.2367431757516,0.133257821719693,25.6426271450638));
#23643=CARTESIAN_POINT('Ctrl Pts',(-7.92891582615506,1.13363424900439,25.6903491685186));
#23644=CARTESIAN_POINT('Ctrl Pts',(-9.14477812717384,1.09445722519328,25.7380711919735));
#23645=CARTESIAN_POINT('Ctrl Pts',(-9.76946397098398,0.0478817062920451,
25.7857932154284));
#23646=CARTESIAN_POINT('Ctrl Pts',(-9.31682784607392,-0.857975580674369,
25.8255615683074));
#23647=CARTESIAN_POINT('Ctrl Pts',(-8.62258000991318,-1.1094594439762,25.8573762506107));
#23648=CARTESIAN_POINT('Ctrl Pts',(-7.89017658990837,-1.01560092342389,
25.8891909329139));
#23649=CARTESIAN_POINT('Ctrl Pts',(-7.25070254053196,-0.23040679067833,
25.928959285793));
#23650=CARTESIAN_POINT('Ctrl Pts',(-7.63184561666349,0.927298990484284,
25.9766813092478));
#23651=CARTESIAN_POINT('Ctrl Pts',(-8.80982869801229,1.230963005951,26.0244033327027));
#23652=CARTESIAN_POINT('Ctrl Pts',(-9.7036958993495,0.405822169119469,26.0721253561575));
#23653=CARTESIAN_POINT('Ctrl Pts',(-9.49136433480964,-0.794372826254335,
26.1198473796125));
#23654=CARTESIAN_POINT('Ctrl Pts',(-8.55637342802605,-1.18328012903448,
26.1596157324914));
#23655=CARTESIAN_POINT('Ctrl Pts',(-7.86680560424831,-0.919233905949376,
26.1914304147947));
#23656=CARTESIAN_POINT('Ctrl Pts',(-7.3743327380729,-0.369056963869812,
26.2232450970979));
#23657=CARTESIAN_POINT('Ctrl Pts',(-7.40446434000579,0.643143101576107,
26.263013449977));
#23658=CARTESIAN_POINT('Ctrl Pts',(-8.45016755396898,1.26928805965477,26.3107354734318));
#23659=CARTESIAN_POINT('Ctrl Pts',(-9.53970213718575,0.728205472420586,
26.3584574968867));
#23660=CARTESIAN_POINT('Ctrl Pts',(-9.67581991443327,-0.48064849930249,
26.4061795203416));
#23661=CARTESIAN_POINT('Ctrl Pts',(-8.72998116914571,-1.24937588149534,
26.4539015437965));
#23662=CARTESIAN_POINT('Ctrl Pts',(-7.76843733819602,-0.931743472748531,
26.4936698966755));
#23663=CARTESIAN_POINT('Ctrl Pts',(-7.41970926141765,-0.280887943478391,
26.5254845789787));
#23664=CARTESIAN_POINT('Ctrl Pts',(-7.40724420078035,0.457399814633881,
26.557299261282));
#23665=CARTESIAN_POINT('Ctrl Pts',(-8.09229249818659,1.20316500297713,26.597067614161));
#23666=CARTESIAN_POINT('Ctrl Pts',(-9.29278247777338,0.992507629187354,
26.6447896376159));
#23667=CARTESIAN_POINT('Ctrl Pts',(-9.76272768922647,-0.129547392843957,
26.6925116610708));
#23668=CARTESIAN_POINT('Ctrl Pts',(-9.07473952994518,-1.13280621633976,
26.7402336845256));
#23669=CARTESIAN_POINT('Ctrl Pts',(-7.85648371084657,-1.09531649171282,
26.7879557079805));
#23670=CARTESIAN_POINT('Ctrl Pts',(-7.33713318762905,-0.225988061280798,
26.8277240608595));
#23671=CARTESIAN_POINT('Ctrl Pts',(-7.49924747934842,0.494389026039019,
26.8595387431628));
#23672=CARTESIAN_POINT('Ctrl Pts',(-7.97286685852847,1.06087722113241,26.8913534254661));
#23673=CARTESIAN_POINT('Ctrl Pts',(-8.97887535588318,1.17665195574207,26.931121778345));
#23674=CARTESIAN_POINT('Ctrl Pts',(-9.74892120859526,0.231886320813893,
26.9788438018));
#23675=CARTESIAN_POINT('Ctrl Pts',(-9.37018187864511,-0.924146764431696,
27.0265658252548));
#23676=CARTESIAN_POINT('Ctrl Pts',(-8.19347744150011,-1.23272842596829,
27.0742878487097));
#23677=CARTESIAN_POINT('Ctrl Pts',(-7.29669616986645,-0.407297586304945,
27.1220098721645));
#23678=CARTESIAN_POINT('Ctrl Pts',(-7.47271888540121,0.589935029256493,
27.1617782250436));
#23679=CARTESIAN_POINT('Ctrl Pts',(-8.06664590501909,1.02865462863956,27.1935929073468));
#23680=CARTESIAN_POINT('Ctrl Pts',(-8.79546342201053,1.14718402769961,27.2254075896501));
#23681=CARTESIAN_POINT('Ctrl Pts',(-9.63200965783638,0.576528894322741,
27.265175942529));
#23682=CARTESIAN_POINT('Ctrl Pts',(-9.59621914441288,-0.64177802898069,
27.312897965984));
#23683=CARTESIAN_POINT('Ctrl Pts',(-8.55342818117192,-1.26823072569173,
27.3606199894388));
#23684=CARTESIAN_POINT('Ctrl Pts',(-7.46164306468287,-0.731703714585647,
27.4083420128937));
#23685=CARTESIAN_POINT('Ctrl Pts',(-7.32351125483922,0.479276187530674,
27.4560640363485));
#23686=CARTESIAN_POINT('Ctrl Pts',(-8.10909730428403,1.11826871083707,27.4958323892276));
#23687=CARTESIAN_POINT('Ctrl Pts',(-8.84530157405367,1.06145793115618,27.5276470715308));
#23688=CARTESIAN_POINT('Ctrl Pts',(-9.47402352945873,0.674246239304349,
27.5594617538341));
#23689=CARTESIAN_POINT('Ctrl Pts',(-9.73329676936124,-0.304648174304312,
27.5992301067131));
#23690=CARTESIAN_POINT('Ctrl Pts',(-8.90911752740845,-1.20257985174657,
27.646952130168));
#23691=CARTESIAN_POINT('Ctrl Pts',(-7.71062860019822,-0.994060630599014,
27.6946741536228));
#23692=CARTESIAN_POINT('Ctrl Pts',(-7.23600079802103,0.126021698354508,
27.7423961770777));
#23693=CARTESIAN_POINT('Ctrl Pts',(-7.92385678992181,1.13220600285667,27.7901182005326));
#23694=CARTESIAN_POINT('Ctrl Pts',(-8.93603819131223,1.10145382239673,27.8298865534116));
#23695=CARTESIAN_POINT('Ctrl Pts',(-9.45562501891254,0.57680754146138,27.8617012357149));
#23696=CARTESIAN_POINT('Ctrl Pts',(-9.67775363486414,-0.127382113028449,
27.8935159180181));
#23697=CARTESIAN_POINT('Ctrl Pts',(-9.23335989624522,-1.03731128115096,
27.9332842708971));
#23698=CARTESIAN_POINT('Ctrl Pts',(-8.02257383277471,-1.17713198321521,
27.9810062943521));
#23699=CARTESIAN_POINT('Ctrl Pts',(-7.25264233434914,-0.235292579725615,
28.0287283178069));
#23700=CARTESIAN_POINT('Ctrl Pts',(-7.62654974800387,0.922312370266984,
28.0764503412618));
#23701=CARTESIAN_POINT('Ctrl Pts',(-8.80506831370423,1.23319291086091,28.1241723647166));
#23702=CARTESIAN_POINT('Ctrl Pts',(-9.55041335584025,0.547687510381144,
28.1639407175957));
#23703=CARTESIAN_POINT('Ctrl Pts',(-9.60008761343399,-0.189032694070671,
28.1957553998989));
#23704=CARTESIAN_POINT('Ctrl Pts',(-9.30733666482934,-0.866912531214819,
28.2275700822022));
#23705=CARTESIAN_POINT('Ctrl Pts',(-8.37591494401209,-1.26429202730366,
28.2673384350812));
#23706=CARTESIAN_POINT('Ctrl Pts',(-7.36877222403689,-0.577840090294717,
28.3150604585361));
#23707=CARTESIAN_POINT('Ctrl Pts',(-7.40273464670435,0.638179041167884,
28.3627824819909));
#23708=CARTESIAN_POINT('Ctrl Pts',(-8.44289989517833,1.26898188682333,28.4105045054458));
#23709=CARTESIAN_POINT('Ctrl Pts',(-9.53756106054564,0.73300646455629,28.4582265289006));
#23710=CARTESIAN_POINT('Ctrl Pts',(-9.65271898526393,-0.273072825713538,
28.4979948817797));
#23711=CARTESIAN_POINT('Ctrl Pts',(-9.20826480219185,-0.862720746617945,
28.5298095640829));
#23712=CARTESIAN_POINT('Ctrl Pts',(-8.54334843224031,-1.18382884768557,
28.5616242463862));
#23713=CARTESIAN_POINT('Ctrl Pts',(-7.57896063259388,-0.874938806376633,
28.6013925992652));
#23714=CARTESIAN_POINT('Ctrl Pts',(-7.26643664337314,0.303145009105122,
28.6491146227201));
#23715=CARTESIAN_POINT('Ctrl Pts',(-8.08773653200828,1.20054261779437,28.696836646175));
#23716=CARTESIAN_POINT('Ctrl Pts',(-9.28708596378458,0.997031160766581,
28.7445586696298));
#23717=CARTESIAN_POINT('Ctrl Pts',(-9.76424968181474,-0.124515764873607,
28.7922806930847));
#23718=CARTESIAN_POINT('Ctrl Pts',(-9.19308176306757,-0.960711973454944,
28.8320490459637));
#23719=CARTESIAN_POINT('Ctrl Pts',(-8.47116760566466,-1.11583816367412,
28.863863728267));
#23720=CARTESIAN_POINT('Ctrl Pts',(-7.758228121604,-0.923636465033635,28.8956784105702));
#23721=CARTESIAN_POINT('Ctrl Pts',(-7.23100690715492,-0.0590587231617129,
28.9354467634493));
#23722=CARTESIAN_POINT('Ctrl Pts',(-7.76545498830421,1.03634892185952,28.9831687869041));
#23723=CARTESIAN_POINT('Ctrl Pts',(-8.97371415403392,1.17764965562194,29.030890810359));
#23724=CARTESIAN_POINT('Ctrl Pts',(-9.74757278787959,0.239034337797246,
29.0786128338138));
#23725=CARTESIAN_POINT('Ctrl Pts',(-9.37462510670265,-0.921337331473851,
29.1263348572688));
#23726=CARTESIAN_POINT('Ctrl Pts',(-8.39557156138249,-1.18001050930352,
29.1661032101478));
#23727=CARTESIAN_POINT('Ctrl Pts',(-7.74812630734483,-0.824991759482091,
29.197917892451));
#23728=CARTESIAN_POINT('Ctrl Pts',(-7.33471595134323,-0.213177748401308,
29.2297325747542));
#23729=CARTESIAN_POINT('Ctrl Pts',(-7.50168042485667,0.785612751106832,
29.2695009276334));
#23730=CARTESIAN_POINT('Ctrl Pts',(-8.62255656767401,1.2643385173517,29.3172229510881));
#23731=CARTESIAN_POINT('Ctrl Pts',(-9.62876399049447,0.580662319132331,
29.3649449745431));
#23732=CARTESIAN_POINT('Ctrl Pts',(-9.59986723103598,-0.635493945930121,
29.4126669979978));
#23733=CARTESIAN_POINT('Ctrl Pts',(-8.55864432369126,-1.26900551071647,
29.4603890214528));
#23734=CARTESIAN_POINT('Ctrl Pts',(-7.64893856382622,-0.824074962017151,
29.5001573743318));
#23735=CARTESIAN_POINT('Ctrl Pts',(-7.39165978122259,-0.131949724328084,
29.5319720566351));
#23736=CARTESIAN_POINT('Ctrl Pts',(-7.47917136641087,0.601160787975001,
29.5637867389383));
#23737=CARTESIAN_POINT('Ctrl Pts',(-8.25924185780237,1.24739438139286,29.6035550918174));
#23738=CARTESIAN_POINT('Ctrl Pts',(-9.41955388337242,0.875818431378234,
29.6512771152722));
#23739=CARTESIAN_POINT('Ctrl Pts',(-9.73420537750695,-0.299113479422314,
29.6989991387271));
#23740=CARTESIAN_POINT('Ctrl Pts',(-8.91473661362289,-1.20075991772479,
29.746721162182));
#23741=CARTESIAN_POINT('Ctrl Pts',(-7.91628087823187,-1.03091022985124,
29.786489515061));
#23742=CARTESIAN_POINT('Ctrl Pts',(-7.47389388983263,-0.439466000029977,
29.8183041973642));
#23743=CARTESIAN_POINT('Ctrl Pts',(-7.35134599695441,0.288282690195251,
29.8501188796675));
#23744=CARTESIAN_POINT('Ctrl Pts',(-7.91595128905028,1.12901342715968,29.8898872325466));
#23745=CARTESIAN_POINT('Ctrl Pts',(-9.13634494738218,1.09918250918627,29.9376092560014));
#23746=CARTESIAN_POINT('Ctrl Pts',(-9.66055134658927,0.235760887270644,
29.9773776088804));
#23747=CARTESIAN_POINT('Ctrl Pts',(-9.50494573724989,-0.488941412697737,
30.0091922911837));
#23748=CARTESIAN_POINT('Ctrl Pts',(-9.26902730932514,-0.770372743754008,
30.0250996323353));
#23749=CARTESIAN_POINT('Ctrl Pts',(-9.12339873206855,-0.874219306856311,
30.0330533029111));
#23750=CARTESIAN_POINT('Ctrl Pts',(-8.98717784885836,1.02066752383268,1.76694669708888));
#23751=CARTESIAN_POINT('Ctrl Pts',(-9.15720195857778,0.939512810771836,
1.77490036766469));
#23752=CARTESIAN_POINT('Ctrl Pts',(-9.45329826783746,0.690609604732661,
1.79080770881631));
#23753=CARTESIAN_POINT('Ctrl Pts',(-9.7469683923631,-0.032794831450878,
1.82262239111956));
#23754=CARTESIAN_POINT('Ctrl Pts',(-9.3607214115926,-1.02415996628745,1.86239074399861));
#23755=CARTESIAN_POINT('Ctrl Pts',(-8.10013924535698,-1.2778080089645,1.91011276745347));
#23756=CARTESIAN_POINT('Ctrl Pts',(-7.36100311520275,-0.508672370427067,
1.94988112033252));
#23757=CARTESIAN_POINT('Ctrl Pts',(-7.35533111002763,0.268650789363701,
1.98169580263576));
#23758=CARTESIAN_POINT('Ctrl Pts',(-7.7063307288449,0.962938239586403,2.013510484939));
#23759=CARTESIAN_POINT('Ctrl Pts',(-8.71112529982286,1.32134053301244,2.05327883781806));
#23760=CARTESIAN_POINT('Ctrl Pts',(-9.72577069974048,0.535519851686026,
2.10100086127292));
#23761=CARTESIAN_POINT('Ctrl Pts',(-9.61375965135636,-0.740763047588873,
2.14872288472778));
#23762=CARTESIAN_POINT('Ctrl Pts',(-8.47786848052187,-1.33797052146523,
2.19644490818264));
#23763=CARTESIAN_POINT('Ctrl Pts',(-7.55070313740433,-0.809923379715486,
2.2362132610617));
#23764=CARTESIAN_POINT('Ctrl Pts',(-7.32613880404449,-0.065370300961561,
2.26802794336494));
#23765=CARTESIAN_POINT('Ctrl Pts',(-7.46673614985931,0.699583561915718,
2.29984262566818));
#23766=CARTESIAN_POINT('Ctrl Pts',(-8.32926454613903,1.32715695287655,2.33961097854723));
#23767=CARTESIAN_POINT('Ctrl Pts',(-9.52502558453072,0.859963540493027,
2.38733300200209));
#23768=CARTESIAN_POINT('Ctrl Pts',(-9.77693128489481,-0.396393259162436,
2.43505502545695));
#23769=CARTESIAN_POINT('Ctrl Pts',(-8.85786004067544,-1.28924928143315,
2.48277704891182));
#23770=CARTESIAN_POINT('Ctrl Pts',(-7.60771327966523,-0.997164717747076,
2.53049907236667));
#23771=CARTESIAN_POINT('Ctrl Pts',(-7.25224299371205,0.00850363864383403,
2.57026742524573));
#23772=CARTESIAN_POINT('Ctrl Pts',(-7.56946535593601,0.718634766301041,
2.60208210754897));
#23773=CARTESIAN_POINT('Ctrl Pts',(-8.17633439356632,1.20507622033207,2.63389678985222));
#23774=CARTESIAN_POINT('Ctrl Pts',(-9.2391996530484,1.11539202291409,2.67366514273126));
#23775=CARTESIAN_POINT('Ctrl Pts',(-9.83784103294923,-0.0203107034754631,
2.72138716618613));
#23776=CARTESIAN_POINT('Ctrl Pts',(-9.2063285939658,-1.13523854117206,2.76910918964099));
#23777=CARTESIAN_POINT('Ctrl Pts',(-7.92710594247716,-1.20914174508905,
2.81683121309585));
#23778=CARTESIAN_POINT('Ctrl Pts',(-7.17278030824983,-0.170303293381034,
2.86455323655072));
#23779=CARTESIAN_POINT('Ctrl Pts',(-7.56194385943746,0.822811344328335,
2.90432158942976));
#23780=CARTESIAN_POINT('Ctrl Pts',(-8.26646746974983,1.15229941527231,2.93613627173301));
#23781=CARTESIAN_POINT('Ctrl Pts',(-9.04368293743357,1.1231102708342,2.96795095403625));
#23782=CARTESIAN_POINT('Ctrl Pts',(-9.78879960305325,0.359876283870339,
3.0077193069153));
#23783=CARTESIAN_POINT('Ctrl Pts',(-9.49845790146036,-0.890681293407522,
3.05544133037016));
#23784=CARTESIAN_POINT('Ctrl Pts',(-8.29140066639367,-1.32066379967401,
3.10316335382503));
#23785=CARTESIAN_POINT('Ctrl Pts',(-7.27563101481108,-0.539584967461653,
3.15088537727989));
#23786=CARTESIAN_POINT('Ctrl Pts',(-7.38485983741583,0.73957945590063,3.19860740073475));
#23787=CARTESIAN_POINT('Ctrl Pts',(-8.32894005637996,1.2360041721841,3.23837575361381));
#23788=CARTESIAN_POINT('Ctrl Pts',(-9.07731547286537,1.0242256745203,3.27019043591704));
#23789=CARTESIAN_POINT('Ctrl Pts',(-9.64598941147203,0.493635580865258,
3.30200511822029));
#23790=CARTESIAN_POINT('Ctrl Pts',(-9.7101184478014,-0.571076786728671,
3.34177347109933));
#23791=CARTESIAN_POINT('Ctrl Pts',(-8.67233310217777,-1.32685065118963,
3.3894954945542));
#23792=CARTESIAN_POINT('Ctrl Pts',(-7.47816356649126,-0.862274235291014,
3.43721751800906));
#23793=CARTESIAN_POINT('Ctrl Pts',(-7.22102781558539,0.393015903201006,
3.48493954146392));
#23794=CARTESIAN_POINT('Ctrl Pts',(-8.14056280244616,1.28892212916197,3.53266156491878));
#23795=CARTESIAN_POINT('Ctrl Pts',(-9.17932683400365,1.04665317585688,3.57242991779784));
#23796=CARTESIAN_POINT('Ctrl Pts',(-9.60672601934412,0.396848718848358,
3.60424460010108));
#23797=CARTESIAN_POINT('Ctrl Pts',(-9.68963365623764,-0.376483176085459,
3.63605928240432));
#23798=CARTESIAN_POINT('Ctrl Pts',(-9.04151258676327,-1.2236337166026,3.67582763528338));
#23799=CARTESIAN_POINT('Ctrl Pts',(-7.76219705954577,-1.11618912811821,
3.72354965873823));
#23800=CARTESIAN_POINT('Ctrl Pts',(-7.1630649420991,0.0164682923005445,
3.7712716821931));
#23801=CARTESIAN_POINT('Ctrl Pts',(-7.78991506235602,1.13402413113802,3.81899370564796));
#23802=CARTESIAN_POINT('Ctrl Pts',(-9.07148901432152,1.20992382427138,3.86671572910283));
#23803=CARTESIAN_POINT('Ctrl Pts',(-9.69854629147273,0.347065707216833,
3.90648408198187));
#23804=CARTESIAN_POINT('Ctrl Pts',(-9.596614981266,-0.423989351762,3.93829876428512));
#23805=CARTESIAN_POINT('Ctrl Pts',(-9.15333939402706,-1.06306888494648,
3.97011344658835));
#23806=CARTESIAN_POINT('Ctrl Pts',(-8.1089229359139,-1.27967733588411,4.00988179946741));
#23807=CARTESIAN_POINT('Ctrl Pts',(-7.211735050573,-0.361392817789792,4.05760382292227));
#23808=CARTESIAN_POINT('Ctrl Pts',(-7.49971327974267,0.88718263676238,4.10532584637714));
#23809=CARTESIAN_POINT('Ctrl Pts',(-8.70496400049602,1.32220312629068,4.15304786983199));
#23810=CARTESIAN_POINT('Ctrl Pts',(-9.72381812702013,0.541095690249467,
4.20076989328686));
#23811=CARTESIAN_POINT('Ctrl Pts',(-9.63348239149061,-0.521713988800163,
4.24053824616591));
#23812=CARTESIAN_POINT('Ctrl Pts',(-9.05191142252884,-1.03813542913569,
4.27235292846915));
#23813=CARTESIAN_POINT('Ctrl Pts',(-8.2985465161075,-1.23141557232177,4.30416761077239));
#23814=CARTESIAN_POINT('Ctrl Pts',(-7.36698075663241,-0.711886752361923,
4.34393596365145));
#23815=CARTESIAN_POINT('Ctrl Pts',(-7.28929364897506,0.569580091172468,
4.39165798710631));
#23816=CARTESIAN_POINT('Ctrl Pts',(-8.32399475052738,1.32540133765357,4.43938001056117));
#23817=CARTESIAN_POINT('Ctrl Pts',(-9.52009434957654,0.865816878233629,
4.48710203401603));
#23818=CARTESIAN_POINT('Ctrl Pts',(-9.77954403027077,-0.391512999309189,
4.5348240574709));
#23819=CARTESIAN_POINT('Ctrl Pts',(-9.01585335320423,-1.1361615800215,4.57459241034995));
#23820=CARTESIAN_POINT('Ctrl Pts',(-8.2381547105969,-1.14619737914636,4.60640709265319));
#23821=CARTESIAN_POINT('Ctrl Pts',(-7.54196087371678,-0.799455346119763,
4.63822177495643));
#23822=CARTESIAN_POINT('Ctrl Pts',(-7.17737793402098,0.202943895239693,
4.67799012783549));
#23823=CARTESIAN_POINT('Ctrl Pts',(-7.95706355310381,1.22288648831522,4.72571215129034));
#23824=CARTESIAN_POINT('Ctrl Pts',(-9.23407761156503,1.11749568853522,4.77343417474522));
#23825=CARTESIAN_POINT('Ctrl Pts',(-9.83793547776687,-0.0126493480030172,
4.82115619820006));
#23826=CARTESIAN_POINT('Ctrl Pts',(-9.21150071631891,-1.13326170177383,
4.86887822165494));
#23827=CARTESIAN_POINT('Ctrl Pts',(-8.14674923105428,-1.19673794632252,
4.90864657453397));
#23828=CARTESIAN_POINT('Ctrl Pts',(-7.55204583831342,-0.695495718811888,
4.94046125683723));
#23829=CARTESIAN_POINT('Ctrl Pts',(-7.25241294297447,0.0222340520685815,
4.97227593914046));
#23830=CARTESIAN_POINT('Ctrl Pts',(-7.63254458493515,1.01884074167864,5.01204429201953));
#23831=CARTESIAN_POINT('Ctrl Pts',(-8.88951136940995,1.28004384369151,5.05976631547437));
#23832=CARTESIAN_POINT('Ctrl Pts',(-9.78630251203301,0.364818312634419,
5.10748833892925));
#23833=CARTESIAN_POINT('Ctrl Pts',(-9.50354194588265,-0.884949101093522,
5.15521036238411));
#23834=CARTESIAN_POINT('Ctrl Pts',(-8.29660552829489,-1.32255285070557,
5.20293238583896));
#23835=CARTESIAN_POINT('Ctrl Pts',(-7.44985251279868,-0.673912511423973,
5.24270073871802));
#23836=CARTESIAN_POINT('Ctrl Pts',(-7.32805832441254,0.0942554856005425,
5.27451542102126));
#23837=CARTESIAN_POINT('Ctrl Pts',(-7.57105541720643,0.833084497531607,
5.3063301033245));
#23838=CARTESIAN_POINT('Ctrl Pts',(-8.51058998985244,1.33805949275232,5.34609845620355));
#23839=CARTESIAN_POINT('Ctrl Pts',(-9.632074979905,0.713188326142003,5.39382047965842));
#23840=CARTESIAN_POINT('Ctrl Pts',(-9.711463480323,-0.565705567887997,5.44154250311327));
#23841=CARTESIAN_POINT('Ctrl Pts',(-8.67992837998318,-1.32584204441887,
5.48926452656815));
#23842=CARTESIAN_POINT('Ctrl Pts',(-7.4808637944681,-0.867108268097873,
5.53698655002299));
#23843=CARTESIAN_POINT('Ctrl Pts',(-7.26489572044008,0.177440797286747,
5.57675490290206));
#23844=CARTESIAN_POINT('Ctrl Pts',(-7.67538459440189,0.838057766740956,
5.60856958520529));
#23845=CARTESIAN_POINT('Ctrl Pts',(-8.3425522063548,1.23781178302893,5.64038426750854));
#23846=CARTESIAN_POINT('Ctrl Pts',(-9.38347284504564,1.00498312726961,5.6801526203876));
#23847=CARTESIAN_POINT('Ctrl Pts',(-9.82275955589709,-0.201341764060873,
5.72787464384245));
#23848=CARTESIAN_POINT('Ctrl Pts',(-9.04604404738165,-1.22045174096105,
5.77559666729732));
#23849=CARTESIAN_POINT('Ctrl Pts',(-7.76860092376069,-1.12039579611335,
5.82331869075218));
#23850=CARTESIAN_POINT('Ctrl Pts',(-7.16194419267288,0.0110458366719952,
5.87104071420704));
#23851=CARTESIAN_POINT('Ctrl Pts',(-7.68204406194035,0.94229289571872,5.9108090670861));
#23852=CARTESIAN_POINT('Ctrl Pts',(-8.42470539828331,1.17331245220397,5.94262374938933));
#23853=CARTESIAN_POINT('Ctrl Pts',(-9.19080374928177,1.03911404470695,5.97443843169258));
#23854=CARTESIAN_POINT('Ctrl Pts',(-9.82566855549311,0.181984161416506,
6.01420678457162));
#23855=CARTESIAN_POINT('Ctrl Pts',(-9.36860763294159,-1.01771908141086,
6.06192880802649));
#23856=CARTESIAN_POINT('Ctrl Pts',(-8.11443176766407,-1.28023579543347,
6.10965083148135));
#23857=CARTESIAN_POINT('Ctrl Pts',(-7.21382565992496,-0.368764037840895,
6.15737285493622));
#23858=CARTESIAN_POINT('Ctrl Pts',(-7.4953179108137,0.883815169420571,6.20509487839108));
#23859=CARTESIAN_POINT('Ctrl Pts',(-8.49794049113376,1.24778346533051,6.24486323127012));
#23860=CARTESIAN_POINT('Ctrl Pts',(-9.2107318204641,0.936585109279635,6.27667791357337));
#23861=CARTESIAN_POINT('Ctrl Pts',(-9.70229305211699,0.33385511043003,6.30849259587662));
#23862=CARTESIAN_POINT('Ctrl Pts',(-9.62160964900884,-0.729730874555741,
6.34826094875566));
#23863=CARTESIAN_POINT('Ctrl Pts',(-8.49101525742003,-1.33796510532709,
6.39598297221054));
#23864=CARTESIAN_POINT('Ctrl Pts',(-7.37078144062068,-0.715913401780636,
6.44370499566537));
#23865=CARTESIAN_POINT('Ctrl Pts',(-7.2860518452889,0.562637739887455,6.49142701912026));
#23866=CARTESIAN_POINT('Ctrl Pts',(-8.31846747525854,1.32573047656402,6.5391490425751));
#23867=CARTESIAN_POINT('Ctrl Pts',(-9.31484091722209,0.944987882223714,
6.57891739545418));
#23868=CARTESIAN_POINT('Ctrl Pts',(-9.65028120019568,0.243278745518274,
6.6107320777574));
#23869=CARTESIAN_POINT('Ctrl Pts',(-9.62767247656973,-0.534155973022973,
6.64254676006066));
#23870=CARTESIAN_POINT('Ctrl Pts',(-8.87077348733239,-1.28570695538331,
6.68231511293969));
#23871=CARTESIAN_POINT('Ctrl Pts',(-7.6178028842378,-1.00596202592991,6.73003713639457));
#23872=CARTESIAN_POINT('Ctrl Pts',(-7.17761766204372,0.197412020801958,
6.77775915984942));
#23873=CARTESIAN_POINT('Ctrl Pts',(-7.95006969414746,1.21975735594301,6.82548118330428));
#23874=CARTESIAN_POINT('Ctrl Pts',(-9.23011293994277,1.1213609806649,6.87320320675915));
#23875=CARTESIAN_POINT('Ctrl Pts',(-9.73451180758851,0.181516982273174,
6.9129715596382));
#23876=CARTESIAN_POINT('Ctrl Pts',(-9.52907613394154,-0.568624391049578,
6.94478624194144));
#23877=CARTESIAN_POINT('Ctrl Pts',(-9.00331905765805,-1.14176956699993,
6.97660092424469));
#23878=CARTESIAN_POINT('Ctrl Pts',(-7.93918771291786,-1.2149094339445,7.01636927712373));
#23879=CARTESIAN_POINT('Ctrl Pts',(-7.17465574624786,-0.183559139566383,
7.0640913005786));
#23880=CARTESIAN_POINT('Ctrl Pts',(-7.6291064911733,1.01450039427264,7.11181332403346));
#23881=CARTESIAN_POINT('Ctrl Pts',(-8.88217491497787,1.28225336148277,7.15953534748833));
#23882=CARTESIAN_POINT('Ctrl Pts',(-9.7858331951435,0.37033545373983,7.20725737094318));
#23883=CARTESIAN_POINT('Ctrl Pts',(-9.55236639024744,-0.670442241066719,
7.24702572382224));
#23884=CARTESIAN_POINT('Ctrl Pts',(-8.90620328656803,-1.10332691326094,
7.27884040612548));
#23885=CARTESIAN_POINT('Ctrl Pts',(-8.13360094072032,-1.19277807964766,
7.31065508842873));
#23886=CARTESIAN_POINT('Ctrl Pts',(-7.2809942040565,-0.551851631768721,
7.35042344130776));
#23887=CARTESIAN_POINT('Ctrl Pts',(-7.37760513024462,0.72832760830481,7.39814546476264));
#23888=CARTESIAN_POINT('Ctrl Pts',(-8.50515012218228,1.33702656291388,7.44586748821749));
#23889=CARTESIAN_POINT('Ctrl Pts',(-9.62797240281083,0.719659368847056,
7.49358951167236));
#23890=CARTESIAN_POINT('Ctrl Pts',(-9.71471830703312,-0.56122614745596,
7.54131153512722));
#23891=CARTESIAN_POINT('Ctrl Pts',(-8.85719934651032,-1.19556532434727,
7.58107988800627));
#23892=CARTESIAN_POINT('Ctrl Pts',(-8.08530903462118,-1.10016489254009,
7.61289457030952));
#23893=CARTESIAN_POINT('Ctrl Pts',(-7.4424999318959,-0.662315199802028,
7.64470925261275));
#23894=CARTESIAN_POINT('Ctrl Pts',(-7.21705792520234,0.380230176003379,
7.68447760549182));
#23895=CARTESIAN_POINT('Ctrl Pts',(-8.12771455933282,1.28515948400945,7.73219962894666));
#23896=CARTESIAN_POINT('Ctrl Pts',(-9.37868310282978,1.00776116143522,7.77992165240154));
#23897=CARTESIAN_POINT('Ctrl Pts',(-9.82389083522868,-0.193763786786019,
7.82764367585639));
#23898=CARTESIAN_POINT('Ctrl Pts',(-9.05143631128576,-1.21919372891482,
7.87536569931126));
#23899=CARTESIAN_POINT('Ctrl Pts',(-7.98789999353893,-1.1378582518537,7.91513405219031));
#23900=CARTESIAN_POINT('Ctrl Pts',(-7.46657387430056,-0.560679792989207,
7.94694873449354));
#23901=CARTESIAN_POINT('Ctrl Pts',(-7.26692318332948,0.191021941458752,
7.97876341679679));
#23902=CARTESIAN_POINT('Ctrl Pts',(-7.77854738769087,1.12695229811292,8.01853176967584));
#23903=CARTESIAN_POINT('Ctrl Pts',(-9.0593106683688,1.21548464610666,8.06625379313071));
#23904=CARTESIAN_POINT('Ctrl Pts',(-9.82386390625267,0.187218886379563,
8.11397581658557));
#23905=CARTESIAN_POINT('Ctrl Pts',(-9.37442127753776,-1.01272838316176,
8.16169784004043));
#23906=CARTESIAN_POINT('Ctrl Pts',(-8.11933277591933,-1.28281246429101,
8.20941986349528));
#23907=CARTESIAN_POINT('Ctrl Pts',(-7.36824599282011,-0.525452838189341,
8.24918821637434));
#23908=CARTESIAN_POINT('Ctrl Pts',(-7.35162708719266,0.252132982124451,
8.28100289867758));
#23909=CARTESIAN_POINT('Ctrl Pts',(-7.69246319392794,0.951237154850419,
8.31281758098083));
#23910=CARTESIAN_POINT('Ctrl Pts',(-8.69174020745547,1.32429265907298,8.35258593385989));
#23911=CARTESIAN_POINT('Ctrl Pts',(-9.71824654100196,0.553269115357872,
8.40030795731473));
#23912=CARTESIAN_POINT('Ctrl Pts',(-9.62366984726379,-0.724591352450493,
8.44802998076961));
#23913=CARTESIAN_POINT('Ctrl Pts',(-8.49867715414896,-1.33799461835653,
8.49575200422446));
#23914=CARTESIAN_POINT('Ctrl Pts',(-7.3728019842507,-0.721068642585769,
8.54347402767932));
#23915=CARTESIAN_POINT('Ctrl Pts',(-7.30031455453236,0.343107344517893,
8.58324238055838));
#23916=CARTESIAN_POINT('Ctrl Pts',(-7.79650446864174,0.942032602887781,
8.61505706286162));
#23917=CARTESIAN_POINT('Ctrl Pts',(-8.51167203456982,1.24773057249472,8.64687174516487));
#23918=CARTESIAN_POINT('Ctrl Pts',(-9.5114609494476,0.8760491434687,8.6866400980439));
#23919=CARTESIAN_POINT('Ctrl Pts',(-9.78329531536966,-0.378661434823328,
8.73436212149879));
#23920=CARTESIAN_POINT('Ctrl Pts',(-8.87569420011532,-1.2831681190302,8.78208414495363));
#23921=CARTESIAN_POINT('Ctrl Pts',(-7.62357790932744,-1.01099736283204,
8.82980616840852));
#23922=CARTESIAN_POINT('Ctrl Pts',(-7.17577273944743,0.192191353705361,
8.87752819186336));
#23923=CARTESIAN_POINT('Ctrl Pts',(-7.81722180370288,1.04440497537604,8.91729654474242));
#23924=CARTESIAN_POINT('Ctrl Pts',(-8.58433124965774,1.17269758585738,8.94911122704566));
#23925=CARTESIAN_POINT('Ctrl Pts',(-9.32519083587387,0.935963622326625,
8.9809259093489));
#23926=CARTESIAN_POINT('Ctrl Pts',(-9.83810119577728,0.00073748833604553,
9.02069426222796));
#23927=CARTESIAN_POINT('Ctrl Pts',(-9.22274614596173,-1.12599705024909,
9.06841628568281));
#23928=CARTESIAN_POINT('Ctrl Pts',(-7.94457012542596,-1.21620894920507,
9.11613830913767));
#23929=CARTESIAN_POINT('Ctrl Pts',(-7.17572861331942,-0.191145607041478,
9.16386033259254));
#23930=CARTESIAN_POINT('Ctrl Pts',(-7.62429548986411,1.01175934142331,9.2115823560474));
#23931=CARTESIAN_POINT('Ctrl Pts',(-8.66697888918347,1.23656211671555,9.25135070892645));
#23932=CARTESIAN_POINT('Ctrl Pts',(-9.33104710651617,0.831680283700215,
9.28316539122969));
#23933=CARTESIAN_POINT('Ctrl Pts',(-9.7364345848479,0.167920622083772,9.31498007353294));
#23934=CARTESIAN_POINT('Ctrl Pts',(-9.5124259956029,-0.87493368746273,9.35474842641199));
#23935=CARTESIAN_POINT('Ctrl Pts',(-8.30986303021255,-1.32441658151513,
9.40247044986685));
#23936=CARTESIAN_POINT('Ctrl Pts',(-7.28421442593712,-0.556355993583608,
9.45019247332171));
#23937=CARTESIAN_POINT('Ctrl Pts',(-7.37345282372569,0.721888362768501,
9.49791449677658));
#23938=CARTESIAN_POINT('Ctrl Pts',(-8.49971837334819,1.33810136937232,9.54563652023143));
#23939=CARTESIAN_POINT('Ctrl Pts',(-9.43533487510731,0.825903438264406,
9.58540487311049));
#23940=CARTESIAN_POINT('Ctrl Pts',(-9.67263301799846,0.0852243664946371,
9.61721955541373));
#23941=CARTESIAN_POINT('Ctrl Pts',(-9.54492468496979,-0.681982566250605,
9.64903423771696));
#23942=CARTESIAN_POINT('Ctrl Pts',(-8.69319984617433,-1.32408050112819,
9.68880259059603));
#23943=CARTESIAN_POINT('Ctrl Pts',(-7.48967042451988,-0.877191824849249,
9.73652461405088));
#23944=CARTESIAN_POINT('Ctrl Pts',(-7.21654611967445,0.374716814105095,
9.78424663750576));
#23945=CARTESIAN_POINT('Ctrl Pts',(-8.12036130107557,1.28300654984733,9.83196866096061));
#23946=CARTESIAN_POINT('Ctrl Pts',(-9.3752785479547,1.01212786619081,9.87969068441547));
#23947=CARTESIAN_POINT('Ctrl Pts',(-9.74772132105027,0.0126223185503058,
9.91945903729454));
#23948=CARTESIAN_POINT('Ctrl Pts',(-9.44256812075637,-0.702777863395229,
9.95127371959776));
#23949=CARTESIAN_POINT('Ctrl Pts',(-8.84402094059755,-1.19942378263872,
9.98308840190103));
#23950=CARTESIAN_POINT('Ctrl Pts',(-7.77979005479142,-1.12774686381844,
10.02285675478));
#23951=CARTESIAN_POINT('Ctrl Pts',(-7.16200677719407,-0.00234187907062422,
10.0705787782349));
#23952=CARTESIAN_POINT('Ctrl Pts',(-7.77455305655034,1.12311766344198,10.1183008016898));
#23953=CARTESIAN_POINT('Ctrl Pts',(-9.05234112294006,1.21866756442496,10.1660228251446));
#23954=CARTESIAN_POINT('Ctrl Pts',(-9.82414624322832,0.192748749863605,
10.2137448485995));
#23955=CARTESIAN_POINT('Ctrl Pts',(-9.45185190919853,-0.806812097631219,
10.2535132014786));
#23956=CARTESIAN_POINT('Ctrl Pts',(-8.75300752431604,-1.14818055208406,
10.2853278837818));
#23957=CARTESIAN_POINT('Ctrl Pts',(-7.97540927235462,-1.13215387045997,
10.3171425660851));
#23958=CARTESIAN_POINT('Ctrl Pts',(-7.21747782872572,-0.38164411985454,
10.3569109189641));
#23959=CARTESIAN_POINT('Ctrl Pts',(-7.48660594026586,0.873649717202334,
10.4046329424189));
#23960=CARTESIAN_POINT('Ctrl Pts',(-8.68621056060662,1.32400611056535,10.4523549658738));
#23961=CARTESIAN_POINT('Ctrl Pts',(-9.71505831551299,0.560236234614444,
10.5000769893287));
#23962=CARTESIAN_POINT('Ctrl Pts',(-9.62750143868948,-0.720594101962218,
10.5477990127836));
#23963=CARTESIAN_POINT('Ctrl Pts',(-8.6919610129374,-1.23293097432137,10.5875673656626));
#23964=CARTESIAN_POINT('Ctrl Pts',(-7.94010744001488,-1.03385284679102,
10.6193820479658));
#23965=CARTESIAN_POINT('Ctrl Pts',(-7.36253209998977,-0.51296646515663,
10.6511967302691));
#23966=CARTESIAN_POINT('Ctrl Pts',(-7.28038664382364,0.550507598009241,
10.6909650831481));
#23967=CARTESIAN_POINT('Ctrl Pts',(-8.30522797742683,1.32374287831698,10.738687106603));
#23968=CARTESIAN_POINT('Ctrl Pts',(-9.50709165300646,0.879450371618857,
10.7864091300578));
#23969=CARTESIAN_POINT('Ctrl Pts',(-9.78544264857298,-0.371306538996862,
10.8341311535127));
#23970=CARTESIAN_POINT('Ctrl Pts',(-8.88120717061705,-1.28265211460467,
10.8818531769676));
#23971=CARTESIAN_POINT('Ctrl Pts',(-7.83849039769771,-1.05800418902331,
10.9216215298466));
#23972=CARTESIAN_POINT('Ctrl Pts',(-7.4001512604151,-0.415528744587011,
10.9534362121499));
#23973=CARTESIAN_POINT('Ctrl Pts',(-7.30416297486433,0.356288685259149,
10.9852508944531));
#23974=CARTESIAN_POINT('Ctrl Pts',(-7.93784887050746,1.21429051780861,11.0250192473322));
#23975=CARTESIAN_POINT('Ctrl Pts',(-9.21880008209559,1.1285201773347,11.072741270787));
#23976=CARTESIAN_POINT('Ctrl Pts',(-9.83702225274205,0.00616841700861393,
11.1204632942419));
#23977=CARTESIAN_POINT('Ctrl Pts',(-9.22918222718139,-1.1218398407237,11.1681853176968));
#23978=CARTESIAN_POINT('Ctrl Pts',(-7.94907693849614,-1.21942573957288,
11.2159073411516));
#23979=CARTESIAN_POINT('Ctrl Pts',(-7.30750132044213,-0.367307387867063,
11.2556756940307));
#23980=CARTESIAN_POINT('Ctrl Pts',(-7.39636403717926,0.40536286104344,11.2874903763339));
#23981=CARTESIAN_POINT('Ctrl Pts',(-7.82875645784298,1.05185546775282,11.3193050586371));
#23982=CARTESIAN_POINT('Ctrl Pts',(-8.86935603952817,1.28611487437698,11.3590734115162));
#23983=CARTESIAN_POINT('Ctrl Pts',(-9.78196192035174,0.383151384494735,
11.4067954349711));
#23984=CARTESIAN_POINT('Ctrl Pts',(-9.51516338353789,-0.870120599928379,
11.4545174584259));
#23985=CARTESIAN_POINT('Ctrl Pts',(-8.31745031259649,-1.32548367032607,
11.5022394818808));
#23986=CARTESIAN_POINT('Ctrl Pts',(-7.28551804013416,-0.561737414803424,
11.5499615053357));
#23987=CARTESIAN_POINT('Ctrl Pts',(-7.35784742999161,0.502449325556585,
11.5897298582147));
#23988=CARTESIAN_POINT('Ctrl Pts',(-7.93059201648363,1.02864276396249,11.621544540518));
#23989=CARTESIAN_POINT('Ctrl Pts',(-8.68057670984098,1.23464969517349,11.6533592228212));
#23990=CARTESIAN_POINT('Ctrl Pts',(-9.62080459220198,0.730966770878588,
11.6931275757003));
#23991=CARTESIAN_POINT('Ctrl Pts',(-9.7201758360483,-0.549001163747355,
11.7408495991551));
#23992=CARTESIAN_POINT('Ctrl Pts',(-8.69841910664045,-1.32223160294096,
11.78857162261));
#23993=CARTESIAN_POINT('Ctrl Pts',(-7.49471015829369,-0.88296301328782,
11.8362936460648));
#23994=CARTESIAN_POINT('Ctrl Pts',(-7.21401103173468,0.369794169139481,
11.8840156695197));
#23995=CARTESIAN_POINT('Ctrl Pts',(-7.96498533229343,1.12726532957765,11.9237840223988));
#23996=CARTESIAN_POINT('Ctrl Pts',(-8.74240260626814,1.1504661507489,11.955598704702));
#23997=CARTESIAN_POINT('Ctrl Pts',(-9.44436701501593,0.815560395604711,
11.9874133870052));
#23998=CARTESIAN_POINT('Ctrl Pts',(-9.82586834953045,-0.180522779014172,
12.0271817398843));
#23999=CARTESIAN_POINT('Ctrl Pts',(-9.06356213495693,-1.21351929062335,
12.0749037633391));
#24000=CARTESIAN_POINT('Ctrl Pts',(-7.78494683297297,-1.12976348056592,
12.122625786794));
#24001=CARTESIAN_POINT('Ctrl Pts',(-7.16204212561228,-0.0100037510999278,
12.1703478102489));
#24002=CARTESIAN_POINT('Ctrl Pts',(-7.7694151050087,1.12105355145961,12.2180698337037));
#24003=CARTESIAN_POINT('Ctrl Pts',(-8.83293933202686,1.20254697168905,12.2578381865828));
#24004=CARTESIAN_POINT('Ctrl Pts',(-9.43604353531208,0.711444929383173,
12.289652868886));
#24005=CARTESIAN_POINT('Ctrl Pts',(-9.74778467198765,-0.00110918061939206,
12.3214675511893));
#24006=CARTESIAN_POINT('Ctrl Pts',(-9.38458009166091,-1.00400867300379,
12.3612359040683));
#24007=CARTESIAN_POINT('Ctrl Pts',(-8.13221563573533,-1.28645482239937,
12.4089579275232));
#24008=CARTESIAN_POINT('Ctrl Pts',(-7.22005822950576,-0.386543164264866,
12.456679950978));
#24009=CARTESIAN_POINT('Ctrl Pts',(-7.48161967120934,0.86783227331347,12.5044019744329));
#24010=CARTESIAN_POINT('Ctrl Pts',(-8.68097446271812,1.32580677244971,12.5521239978878));
#24011=CARTESIAN_POINT('Ctrl Pts',(-9.53858761847399,0.691594951312903,
12.5918923507668));
#24012=CARTESIAN_POINT('Ctrl Pts',(-9.67336945723156,-0.0744009702940164,
12.62370703307));
#24013=CARTESIAN_POINT('Ctrl Pts',(-9.44291558800347,-0.817238038657684,
12.6555217153733));
#24014=CARTESIAN_POINT('Ctrl Pts',(-8.51206491367397,-1.33804700660616,
12.6952900682523));
#24015=CARTESIAN_POINT('Ctrl Pts',(-7.38016157160731,-0.732252171705333,
12.7430120917072));
#24016=CARTESIAN_POINT('Ctrl Pts',(-7.27913273895857,0.545114377551169,
12.7907341151621));
#24017=CARTESIAN_POINT('Ctrl Pts',(-8.29765086394642,1.32260582783026,12.8384561386169));
#24018=CARTESIAN_POINT('Ctrl Pts',(-9.50430997171838,0.884237996659668,
12.8861781620718));
#24019=CARTESIAN_POINT('Ctrl Pts',(-9.73793133825872,-0.156505014890767,
12.9259465149508));
#24020=CARTESIAN_POINT('Ctrl Pts',(-9.3386855611913,-0.823976891055697,
12.9577611972541));
#24021=CARTESIAN_POINT('Ctrl Pts',(-8.67838141684562,-1.23496878019371,
12.9895758795573));
#24022=CARTESIAN_POINT('Ctrl Pts',(-7.63366817039504,-1.01979631056548,
13.0293442324364));
#24023=CARTESIAN_POINT('Ctrl Pts',(-7.17402130438394,0.178918549749654,
13.0770662558912));
#24024=CARTESIAN_POINT('Ctrl Pts',(-7.93337193029169,1.2110322804593,13.1247882793461));
#24025=CARTESIAN_POINT('Ctrl Pts',(-9.2123259166928,1.13261782481115,13.172510302801));
#24026=CARTESIAN_POINT('Ctrl Pts',(-9.83805103920895,0.01160906979348,13.2202323262558));
#24027=CARTESIAN_POINT('Ctrl Pts',(-9.33379175184362,-0.928309825697517,
13.2600006791349));
#24028=CARTESIAN_POINT('Ctrl Pts',(-8.59514802384834,-1.17186954952432,
13.2918153614381));
#24029=CARTESIAN_POINT('Ctrl Pts',(-7.82688748962083,-1.050660442912,13.3236300437414));
#24030=CARTESIAN_POINT('Ctrl Pts',(-7.17760244066937,-0.204401685673198,
13.3633983966204));
#24031=CARTESIAN_POINT('Ctrl Pts',(-7.61428684534256,1.00286766641413,13.4111204200753));
#24032=CARTESIAN_POINT('Ctrl Pts',(-8.86383854258517,1.286579989206,13.4588424435302));
#24033=CARTESIAN_POINT('Ctrl Pts',(-9.77974681566496,0.390486154002405,
13.506564466985));
#24034=CARTESIAN_POINT('Ctrl Pts',(-9.51950111118942,-0.866679201500273,
13.5542864904399));
#24035=CARTESIAN_POINT('Ctrl Pts',(-8.52318422368264,-1.24756976145673,
13.5940548433189));
#24036=CARTESIAN_POINT('Ctrl Pts',(-7.80522645676502,-0.948483585079513,
13.6258695256222));
#24037=CARTESIAN_POINT('Ctrl Pts',(-7.30353144101171,-0.354162117230974,
13.6576842079254));
#24038=CARTESIAN_POINT('Ctrl Pts',(-7.36619673896916,0.710637403536776,
13.6974525608045));
#24039=CARTESIAN_POINT('Ctrl Pts',(-8.48633166710459,1.33792545582631,13.7451745842593));
#24040=CARTESIAN_POINT('Ctrl Pts',(-9.61693628164932,0.734928497495645,
13.7928966077142));
#24041=CARTESIAN_POINT('Ctrl Pts',(-9.72329964090166,-0.542004923632641,
13.840618631169));
#24042=CARTESIAN_POINT('Ctrl Pts',(-8.70395116205371,-1.32246711774871,
13.8883406546239));
#24043=CARTESIAN_POINT('Ctrl Pts',(-7.70127454044465,-0.958647723716633,
13.9281090075029));
#24044=CARTESIAN_POINT('Ctrl Pts',(-7.35400237796188,-0.26271817186398,
13.9599236898062));
#24045=CARTESIAN_POINT('Ctrl Pts',(-7.36344586906573,0.514987888581172,
13.9917383721094));
#24046=CARTESIAN_POINT('Ctrl Pts',(-8.10751259734313,1.27924547792257,14.0315067249885));
#24047=CARTESIAN_POINT('Ctrl Pts',(-9.36503971038065,1.02075347079337,14.0792287484434));
#24048=CARTESIAN_POINT('Ctrl Pts',(-9.82553500107283,-0.174995756024761,
14.1269507718982));
#24049=CARTESIAN_POINT('Ctrl Pts',(-9.07050201522982,-1.21027220049496,
14.1746727953531));
#24050=CARTESIAN_POINT('Ctrl Pts',(-7.78897637587278,-1.13356109670482,
14.2223948188079));
#24051=CARTESIAN_POINT('Ctrl Pts',(-7.2687382143401,-0.202391287121085,
14.262163171687));
#24052=CARTESIAN_POINT('Ctrl Pts',(-7.4614445292402,0.551120605402827,14.2939778539902));
#24053=CARTESIAN_POINT('Ctrl Pts',(-7.97742288800319,1.13308471878577,14.3257925362935));
#24054=CARTESIAN_POINT('Ctrl Pts',(-9.04016345797176,1.22422987739303,14.3655608891725));
#24055=CARTESIAN_POINT('Ctrl Pts',(-9.82204663964461,0.205970947654117,
14.4132829126274));
#24056=CARTESIAN_POINT('Ctrl Pts',(-9.38794421045684,-0.999610740643557,
14.4610049360823));
#24057=CARTESIAN_POINT('Ctrl Pts',(-8.13958844588438,-1.28853981713142,
14.5087269595371));
#24058=CARTESIAN_POINT('Ctrl Pts',(-7.22062088448637,-0.392051569086001,
14.556448982992));
#24059=CARTESIAN_POINT('Ctrl Pts',(-7.43643383184107,0.652529557846704,
14.596217335871));
#24060=CARTESIAN_POINT('Ctrl Pts',(-8.07517557537772,1.09629174757525,14.6280320181743));
#24061=CARTESIAN_POINT('Ctrl Pts',(-8.84615277857736,1.19881027348058,14.6598467004775));
#24062=CARTESIAN_POINT('Ctrl Pts',(-9.70948822007665,0.572410341860612,
14.6996150533566));
#24063=CARTESIAN_POINT('Ctrl Pts',(-9.63456461195216,-0.709221044626205,
14.7473370768114));
#24064=CARTESIAN_POINT('Ctrl Pts',(-8.51748651405567,-1.33692212764019,
14.7950591002663));
#24065=CARTESIAN_POINT('Ctrl Pts',(-7.38437311583038,-0.738652830313837,
14.8427811237211));
#24066=CARTESIAN_POINT('Ctrl Pts',(-7.27595421509225,0.540580495017316,
14.890503147176));
#24067=CARTESIAN_POINT('Ctrl Pts',(-8.12261089372266,1.18934657651418,14.930271500055));
#24068=CARTESIAN_POINT('Ctrl Pts',(-8.89600570638269,1.10702794383491,14.9620861823583));
#24069=CARTESIAN_POINT('Ctrl Pts',(-9.54613549047543,0.680123780107426,
14.9939008646615));
#24070=CARTESIAN_POINT('Ctrl Pts',(-9.78919550284478,-0.358455431482166,
15.0336692175406));
#24071=CARTESIAN_POINT('Ctrl Pts',(-8.89398987797994,-1.27867249171216,
15.0813912409954));
#24072=CARTESIAN_POINT('Ctrl Pts',(-7.63850424481128,-1.02249284858274,
15.1291132644503));
#24073=CARTESIAN_POINT('Ctrl Pts',(-7.17301850815132,0.171322491751843,
15.1768352879052));
#24074=CARTESIAN_POINT('Ctrl Pts',(-7.92800168663425,1.20968318577025,15.22455731136));
#24075=CARTESIAN_POINT('Ctrl Pts',(-8.99276272638861,1.1463649888735,15.2643256642391));
#24076=CARTESIAN_POINT('Ctrl Pts',(-9.52378556829048,0.57809543448961,15.2961403465423));
#24077=CARTESIAN_POINT('Ctrl Pts',(-9.73613438343296,-0.170118697936061,
15.3279550288456));
#24078=CARTESIAN_POINT('Ctrl Pts',(-9.24042793398194,-1.11457622565287,
15.3677233817246));
#24079=CARTESIAN_POINT('Ctrl Pts',(-7.96134871130471,-1.22478015611113,
15.4154454051795));
#24080=CARTESIAN_POINT('Ctrl Pts',(-7.17949357668821,-0.209604062739865,
15.4631674286343));
#24081=CARTESIAN_POINT('Ctrl Pts',(-7.60856208280836,0.997777280360243,
15.5108894520892));
#24082=CARTESIAN_POINT('Ctrl Pts',(-8.85888755748251,1.28907723916839,15.5586114755441));
#24083=CARTESIAN_POINT('Ctrl Pts',(-9.6227081975725,0.544531299390886,15.5983798284232));
#24084=CARTESIAN_POINT('Ctrl Pts',(-9.6524604840685,-0.232645704807483,
15.6301945107264));
#24085=CARTESIAN_POINT('Ctrl Pts',(-9.32356561027203,-0.937451486115936,
15.6620091930296));
#24086=CARTESIAN_POINT('Ctrl Pts',(-8.33062250286166,-1.32730170138441,
15.7017775459087));
#24087=CARTESIAN_POINT('Ctrl Pts',(-7.29143763865007,-0.5738941464571,15.7494995693635));
#24088=CARTESIAN_POINT('Ctrl Pts',(-7.36396336164215,0.705608630834335,
15.7972215928184));
#24089=CARTESIAN_POINT('Ctrl Pts',(-8.47915970912695,1.33755299057857,15.8449436162733));
#24090=CARTESIAN_POINT('Ctrl Pts',(-9.61388803974747,0.74057287343333,15.8926656397281));
#24091=CARTESIAN_POINT('Ctrl Pts',(-9.72534585944743,-0.536397493182908,
15.940387663183));
#24092=CARTESIAN_POINT('Ctrl Pts',(-8.71120078832479,-1.32093775301502,
15.9881096866378));
#24093=CARTESIAN_POINT('Ctrl Pts',(-7.50338587949291,-0.891752812389831,
16.0358317100927));
#24094=CARTESIAN_POINT('Ctrl Pts',(-7.21028788424701,0.355837225553266,
16.0835537335475));
#24095=CARTESIAN_POINT('Ctrl Pts',(-8.10323378877393,1.27788697335254,16.1312757570025));
#24096=CARTESIAN_POINT('Ctrl Pts',(-9.14870221826696,1.06595545650804,16.1710441098815));
#24097=CARTESIAN_POINT('Ctrl Pts',(-9.59472863327079,0.428787139268216,
16.2028587921847));
#24098=CARTESIAN_POINT('Ctrl Pts',(-9.70006919023239,-0.3417922930199,16.234673474488));
#24099=CARTESIAN_POINT('Ctrl Pts',(-9.07678836300807,-1.20740862666961,
16.274441827367));
#24100=CARTESIAN_POINT('Ctrl Pts',(-7.79490301569173,-1.13712765515989,
16.3221638508219));
#24101=CARTESIAN_POINT('Ctrl Pts',(-7.16314844340014,-0.0223381454320956,
16.3698858742767));
#24102=CARTESIAN_POINT('Ctrl Pts',(-7.75730541764752,1.1129404292059,16.4176078977316));
#24103=CARTESIAN_POINT('Ctrl Pts',(-9.03613551984794,1.22599852877919,16.4653299211865));
#24104=CARTESIAN_POINT('Ctrl Pts',(-9.68796982707485,0.381701814578363,
16.5050982740655));
#24105=CARTESIAN_POINT('Ctrl Pts',(-9.60845727250044,-0.39198685725222,
16.5369129563688));
#24106=CARTESIAN_POINT('Ctrl Pts',(-9.18391479352499,-1.04366103090541,
16.568727638672));
#24107=CARTESIAN_POINT('Ctrl Pts',(-8.14622411834344,-1.29048754584716,
16.6084959915511));
#24108=CARTESIAN_POINT('Ctrl Pts',(-7.22276535703482,-0.398626319625968,
16.6562180150059));
#24109=CARTESIAN_POINT('Ctrl Pts',(-7.47438832997941,0.857780428739577,
16.7039400384608));
#24110=CARTESIAN_POINT('Ctrl Pts',(-8.6665070580179,1.32759435244441,16.7516620619156));
#24111=CARTESIAN_POINT('Ctrl Pts',(-9.70759996620601,0.576383260108618,
16.7993840853705));
#24112=CARTESIAN_POINT('Ctrl Pts',(-9.64814525244498,-0.488600347920483,
16.8391524382496));
#24113=CARTESIAN_POINT('Ctrl Pts',(-9.08180588707221,-1.02168160289158,
16.8709671205528));
#24114=CARTESIAN_POINT('Ctrl Pts',(-8.33436731254839,-1.23674315419589,
16.9027818028561));
#24115=CARTESIAN_POINT('Ctrl Pts',(-7.38811706486369,-0.744467389276554,
16.9425501557351));
#24116=CARTESIAN_POINT('Ctrl Pts',(-7.27327423010892,0.534205235745406,
16.9902721791899));
#24117=CARTESIAN_POINT('Ctrl Pts',(-8.28560544341343,1.31973540062158,17.0379942026448));
#24118=CARTESIAN_POINT('Ctrl Pts',(-9.49453851638878,0.895055578304513,
17.0857162260997));
#24119=CARTESIAN_POINT('Ctrl Pts',(-9.79036691067929,-0.354215456745108,
17.1334382495546));
#24120=CARTESIAN_POINT('Ctrl Pts',(-9.04860774557578,-1.12071288000705,
17.1732066024336));
#24121=CARTESIAN_POINT('Ctrl Pts',(-8.2715278914335,-1.15331343665304,17.2050212847369));
#24122=CARTESIAN_POINT('Ctrl Pts',(-7.56556474468814,-0.826921139859261,
17.2368359670401));
#24123=CARTESIAN_POINT('Ctrl Pts',(-7.1720455135375,0.164475639288519,17.2766043199192));
#24124=CARTESIAN_POINT('Ctrl Pts',(-7.92180379170907,1.20661530463984,17.324326343374));
#24125=CARTESIAN_POINT('Ctrl Pts',(-9.20133846749202,1.13832811952868,17.3720483668289));
#24126=CARTESIAN_POINT('Ctrl Pts',(-9.83773905932737,0.0261831591494336,
17.4197703902837));
#24127=CARTESIAN_POINT('Ctrl Pts',(-9.24408855175464,-1.11213649395089,
17.4674924137386));
#24128=CARTESIAN_POINT('Ctrl Pts',(-8.18162760790967,-1.20648532435476,
17.5072607666176));
#24129=CARTESIAN_POINT('Ctrl Pts',(-7.57262853067048,-0.722712629900904,
17.5390754489209));
#24130=CARTESIAN_POINT('Ctrl Pts',(-7.25229315869388,-0.0139805610356614,
17.5708901312241));
#24131=CARTESIAN_POINT('Ctrl Pts',(-7.60334295498851,0.993237885735805,
17.6106584841032));
#24132=CARTESIAN_POINT('Ctrl Pts',(-8.85220016516547,1.29080842588264,17.658380507558));
#24133=CARTESIAN_POINT('Ctrl Pts',(-9.77517364622778,0.401993439824491,
17.7061025310129));
#24134=CARTESIAN_POINT('Ctrl Pts',(-9.52880069492294,-0.8554533761686,17.7538245544678));
#24135=CARTESIAN_POINT('Ctrl Pts',(-8.33507196537348,-1.32789837616584,
17.8015465779226));
#24136=CARTESIAN_POINT('Ctrl Pts',(-7.46985189706413,-0.70410418543467,
17.8413149308017));
#24137=CARTESIAN_POINT('Ctrl Pts',(-7.32581660245188,0.0602057843310409,
17.8731296131049));
#24138=CARTESIAN_POINT('Ctrl Pts',(-7.54727037171921,0.805775448450091,
17.9049442954082));
#24139=CARTESIAN_POINT('Ctrl Pts',(-8.47175475110896,1.33780325905746,17.9447126482872));
#24140=CARTESIAN_POINT('Ctrl Pts',(-9.61090129709441,0.74574101187086,17.9924346717421));
#24141=CARTESIAN_POINT('Ctrl Pts',(-9.72737014095729,-0.53031037212398,
18.0401566951969));
#24142=CARTESIAN_POINT('Ctrl Pts',(-8.71832882409182,-1.32006207173862,
18.0878787186518));
#24143=CARTESIAN_POINT('Ctrl Pts',(-7.50645670057225,-0.896318618679687,
18.1356007421067));
#24144=CARTESIAN_POINT('Ctrl Pts',(-7.26026654510378,0.141523067872558,
18.1753690949857));
#24145=CARTESIAN_POINT('Ctrl Pts',(-7.65141128269188,0.81377427853301,18.207183777289));
#24146=CARTESIAN_POINT('Ctrl Pts',(-8.30669695137759,1.23272127803583,18.2389984595922));
#24147=CARTESIAN_POINT('Ctrl Pts',(-9.3539359184848,1.03019842804731,18.2787668124713));
#24148=CARTESIAN_POINT('Ctrl Pts',(-9.82804542427443,-0.162870192902072,
18.3264888359261));
#24149=CARTESIAN_POINT('Ctrl Pts',(-9.08123184303367,-1.2040913994957,18.374210859381));
#24150=CARTESIAN_POINT('Ctrl Pts',(-7.80142310145517,-1.14114927397414,
18.4219328828358));
#24151=CARTESIAN_POINT('Ctrl Pts',(-7.16218719604133,-0.0277894871109879,
18.4696549062907));
#24152=CARTESIAN_POINT('Ctrl Pts',(-7.65504301923606,0.918158765457952,
18.5094232591697));
#24153=CARTESIAN_POINT('Ctrl Pts',(-8.39068732707389,1.17063321629036,18.541237941473));
#24154=CARTESIAN_POINT('Ctrl Pts',(-9.16035748349834,1.05872367117993,18.5730526237762));
#24155=CARTESIAN_POINT('Ctrl Pts',(-9.81982899665625,0.220378704994469,
18.6128209766553));
#24156=CARTESIAN_POINT('Ctrl Pts',(-9.39777622677681,-0.992083260269288,
18.6605430001101));
#24157=CARTESIAN_POINT('Ctrl Pts',(-8.15174688163843,-1.29088586608082,
18.708265023565));
#24158=CARTESIAN_POINT('Ctrl Pts',(-7.22506897755392,-0.405933783611097,
18.7559870470198));
#24159=CARTESIAN_POINT('Ctrl Pts',(-7.47009254891817,0.854286834872094,
18.8037090704747));
#24160=CARTESIAN_POINT('Ctrl Pts',(-8.4617304100637,1.24719816244857,18.8434774233538));
#24161=CARTESIAN_POINT('Ctrl Pts',(-9.18325257355315,0.956816235375206,
18.875292105657));
#24162=CARTESIAN_POINT('Ctrl Pts',(-9.69209812790066,0.368605305692601,
18.9071067879602));
#24163=CARTESIAN_POINT('Ctrl Pts',(-9.64231420404793,-0.696874173190531,
18.9468751408393));
#24164=CARTESIAN_POINT('Ctrl Pts',(-8.52984708092943,-1.3376623267597,18.9945971642942));
#24165=CARTESIAN_POINT('Ctrl Pts',(-7.39203300266752,-0.748382045828093,
19.042319187749));
#24166=CARTESIAN_POINT('Ctrl Pts',(-7.27023526017598,0.527171730423539,
19.0900412112039));
#24167=CARTESIAN_POINT('Ctrl Pts',(-8.28007094449939,1.31990399824239,19.1377632346588));
#24168=CARTESIAN_POINT('Ctrl Pts',(-9.28707397183385,0.96823673798853,19.1775315875378));
#24169=CARTESIAN_POINT('Ctrl Pts',(-9.64273672796038,0.276557694007988,
19.2093462698411));
#24170=CARTESIAN_POINT('Ctrl Pts',(-9.64269885177062,-0.501205698382487,
19.2411609521443));
#24171=CARTESIAN_POINT('Ctrl Pts',(-8.90792882316648,-1.2744055199424,19.2809293050234));
#24172=CARTESIAN_POINT('Ctrl Pts',(-7.64736768134579,-1.03113989247751,
19.3286513284782));
#24173=CARTESIAN_POINT('Ctrl Pts',(-7.17244567679856,0.158953051700663,
19.3763733519331));
#24174=CARTESIAN_POINT('Ctrl Pts',(-7.914903686496,1.20328452686644,19.4240953753879));
#24175=CARTESIAN_POINT('Ctrl Pts',(-9.1972632940707,1.14207672805785,19.4718173988428));
#24176=CARTESIAN_POINT('Ctrl Pts',(-9.72872419935639,0.217266333896879,
19.5115857517218));
#24177=CARTESIAN_POINT('Ctrl Pts',(-9.54514431649316,-0.538520886546302,
19.5434004340251));
#24178=CARTESIAN_POINT('Ctrl Pts',(-9.03624147415713,-1.12668225304333,
19.5752151163283));
#24179=CARTESIAN_POINT('Ctrl Pts',(-7.97468085007939,-1.2306726391516,19.6149834692074));
#24180=CARTESIAN_POINT('Ctrl Pts',(-7.18054087470649,-0.221943608495227,
19.6627054926623));
#24181=CARTESIAN_POINT('Ctrl Pts',(-7.60003226709561,0.988799592145305,
19.7104275161171));
#24182=CARTESIAN_POINT('Ctrl Pts',(-8.84480267997769,1.29280410757097,19.7581495395719));
#24183=CARTESIAN_POINT('Ctrl Pts',(-9.77454441836398,0.407494637568213,
19.8058715630269));
#24184=CARTESIAN_POINT('Ctrl Pts',(-9.57137953974861,-0.639619965086357,
19.8456399159058));
#24185=CARTESIAN_POINT('Ctrl Pts',(-8.93805099162274,-1.09107411126967,
19.8774545982092));
#24186=CARTESIAN_POINT('Ctrl Pts',(-8.16836993911467,-1.20290869173274,
19.9092692805123));
#24187=CARTESIAN_POINT('Ctrl Pts',(-7.29752247389199,-0.586995019770082,
19.9490376333915));
#24188=CARTESIAN_POINT('Ctrl Pts',(-7.35694162901394,0.695448710683165,
19.9967596568463));
#24189=CARTESIAN_POINT('Ctrl Pts',(-8.46634715042567,1.33661289811648,20.0444816803011));
#24190=CARTESIAN_POINT('Ctrl Pts',(-9.60661265683251,0.752090271450374,
20.092203703756));
#24191=CARTESIAN_POINT('Ctrl Pts',(-9.73049360305648,-0.525738382531365,
20.1399257272109));
#24192=CARTESIAN_POINT('Ctrl Pts',(-8.8917444696308,-1.18469577885746,20.1796940800899));
#24193=CARTESIAN_POINT('Ctrl Pts',(-8.11741071746799,-1.11173595265972,
20.2115087623932));
#24194=CARTESIAN_POINT('Ctrl Pts',(-7.46216585637197,-0.692725131815518,
20.2433234446964));
#24195=CARTESIAN_POINT('Ctrl Pts',(-7.20656390593258,0.342838773468356,
20.2830917975755));
#24196=CARTESIAN_POINT('Ctrl Pts',(-8.09057574803475,1.27381440193415,20.3308138210303));
#24197=CARTESIAN_POINT('Ctrl Pts',(-9.34906757443192,1.03283629280933,20.3785358444852));
#24198=CARTESIAN_POINT('Ctrl Pts',(-9.82895631258486,-0.155262577310471,
20.42625786794));
#24199=CARTESIAN_POINT('Ctrl Pts',(-9.08658532806561,-1.20267743261765,
20.4739798913949));
#24200=CARTESIAN_POINT('Ctrl Pts',(-8.0211365721744,-1.1522402680952,20.5137482442739));
#24201=CARTESIAN_POINT('Ctrl Pts',(-7.48328017774149,-0.59043390025575,
20.5455629265772));
#24202=CARTESIAN_POINT('Ctrl Pts',(-7.26189902630817,0.155157329418629,
20.5773776088804));
#24203=CARTESIAN_POINT('Ctrl Pts',(-7.74614684401822,1.10554094146076,20.6171459617595));
#24204=CARTESIAN_POINT('Ctrl Pts',(-9.02380147086936,1.23120403174586,20.6648679852144));
#24205=CARTESIAN_POINT('Ctrl Pts',(-9.81787319462849,0.225558853906263,
20.7125900086692));
#24206=CARTESIAN_POINT('Ctrl Pts',(-9.40344259165754,-0.986925950743689,
20.7603120321241));
#24207=CARTESIAN_POINT('Ctrl Pts',(-8.15672060120297,-1.2933192213801,20.8080340555789));
#24208=CARTESIAN_POINT('Ctrl Pts',(-7.38397141561257,-0.558075278756529,
20.847802408458));
#24209=CARTESIAN_POINT('Ctrl Pts',(-7.34479379924817,0.218700757404031,
20.8796170907612));
#24210=CARTESIAN_POINT('Ctrl Pts',(-7.66519819859131,0.927401622973458,
20.9114317730645));
#24211=CARTESIAN_POINT('Ctrl Pts',(-8.65322818924572,1.32929924247707,20.9512001259435));
#24212=CARTESIAN_POINT('Ctrl Pts',(-9.70167745526272,0.588389872606148,
20.9989221493984));
#24213=CARTESIAN_POINT('Ctrl Pts',(-9.64422438454522,-0.691677028321677,
21.0466441728533));
#24214=CARTESIAN_POINT('Ctrl Pts',(-8.53750660713187,-1.33746947744374,
21.0943661963081));
#24215=CARTESIAN_POINT('Ctrl Pts',(-7.39420230150788,-0.753476478756427,
21.142088219763));
#24216=CARTESIAN_POINT('Ctrl Pts',(-7.29086278230429,0.308147702753215,
21.181856572642));
#24217=CARTESIAN_POINT('Ctrl Pts',(-7.76946277180434,0.921220248238589,
21.2136712549453));
#24218=CARTESIAN_POINT('Ctrl Pts',(-8.47545770507547,1.24754378427726,21.2454859372485));
#24219=CARTESIAN_POINT('Ctrl Pts',(-9.48561180981664,0.905032990768657,
21.2852542901276));
#24220=CARTESIAN_POINT('Ctrl Pts',(-9.79374366065181,-0.34126044188475,
21.3329763135824));
#24221=CARTESIAN_POINT('Ctrl Pts',(-8.91277378588204,-1.2717249527254,21.3806983370373));
#24222=CARTESIAN_POINT('Ctrl Pts',(-7.65328640071379,-1.03600551613202,
21.4284203604922));
#24223=CARTESIAN_POINT('Ctrl Pts',(-7.17075303613647,0.153681043363308,
21.476142383947));
#24224=CARTESIAN_POINT('Ctrl Pts',(-7.78720051264544,1.02415072560441,21.5159107368261));
#24225=CARTESIAN_POINT('Ctrl Pts',(-8.55026379154953,1.1746509859544,21.5477254191293));
#24226=CARTESIAN_POINT('Ctrl Pts',(-9.29768141734801,0.95951663578424,21.5795401014325));
#24227=CARTESIAN_POINT('Ctrl Pts',(-9.83751621862897,0.0395691664571907,
21.6193084543116));
#24228=CARTESIAN_POINT('Ctrl Pts',(-9.25511842332855,-1.10454855729479,
21.6670304777665));
#24229=CARTESIAN_POINT('Ctrl Pts',(-7.98009870786515,-1.23181540830285,
21.7147525012213));
#24230=CARTESIAN_POINT('Ctrl Pts',(-7.18183345085486,-0.229495745901632,
21.7624745246762));
#24231=CARTESIAN_POINT('Ctrl Pts',(-7.59530283801286,0.985920077451556,
21.810196548131));
#24232=CARTESIAN_POINT('Ctrl Pts',(-8.63102325931338,1.24088707119056,21.8499649010101));
#24233=CARTESIAN_POINT('Ctrl Pts',(-9.30656154672025,0.855447168968843,
21.8817795833133));
#24234=CARTESIAN_POINT('Ctrl Pts',(-9.73104073612964,0.203731499573318,
21.9135942656166));
#24235=CARTESIAN_POINT('Ctrl Pts',(-9.53739035341218,-0.845184363720151,
21.9533626184956));
#24236=CARTESIAN_POINT('Ctrl Pts',(-8.3483779694346,-1.32937658641915,22.0010846419505));
#24237=CARTESIAN_POINT('Ctrl Pts',(-7.30087205705786,-0.591404032917553,
22.0488066654053));
#24238=CARTESIAN_POINT('Ctrl Pts',(-7.35297793965443,0.688891676356153,
22.0965286888602));
#24239=CARTESIAN_POINT('Ctrl Pts',(-8.46088649819163,1.33752962135645,22.1442507123151));
#24240=CARTESIAN_POINT('Ctrl Pts',(-9.410973037202,0.85269921040183,22.1840190651941));
#24241=CARTESIAN_POINT('Ctrl Pts',(-9.66966590430475,0.11921853820421,22.2158337474974));
#24242=CARTESIAN_POINT('Ctrl Pts',(-9.56427587148831,-0.651371389682384,
22.2476484298006));
#24243=CARTESIAN_POINT('Ctrl Pts',(-8.73154358029947,-1.31791612952105,
22.2874167826797));
#24244=CARTESIAN_POINT('Ctrl Pts',(-7.51555224850724,-0.906142358160704,
22.3351388061345));
#24245=CARTESIAN_POINT('Ctrl Pts',(-7.20621231493002,0.337312880953408,
22.3828608295894));
#24246=CARTESIAN_POINT('Ctrl Pts',(-8.08328806540698,1.27144898137517,22.4305828530443));
#24247=CARTESIAN_POINT('Ctrl Pts',(-9.34553773074606,1.03710235749152,22.4783048764991));
#24248=CARTESIAN_POINT('Ctrl Pts',(-9.74682950929964,0.0488261473860323,
22.5180732293782));
#24249=CARTESIAN_POINT('Ctrl Pts',(-9.46256590138573,-0.675128338195107,
22.5498879116814));
#24250=CARTESIAN_POINT('Ctrl Pts',(-8.87868358743782,-1.18893505227754,
22.5817025939847));
#24251=CARTESIAN_POINT('Ctrl Pts',(-7.81282084949026,-1.14817253456714,
22.6214709468637));
#24252=CARTESIAN_POINT('Ctrl Pts',(-7.1626382686361,-0.0411697480629679,
22.6691929703186));
#24253=CARTESIAN_POINT('Ctrl Pts',(-7.74226547712604,1.1015920054815,22.7169149937735));
#24254=CARTESIAN_POINT('Ctrl Pts',(-9.01674249185626,1.23418335176844,22.7646370172283));
#24255=CARTESIAN_POINT('Ctrl Pts',(-9.81799493484566,0.231094581829405,
22.8123590406832));
#24256=CARTESIAN_POINT('Ctrl Pts',(-9.47486487590842,-0.778849338222097,
22.8521273935622));
#24257=CARTESIAN_POINT('Ctrl Pts',(-8.78622141401848,-1.14035463330573,
22.8839420758655));
#24258=CARTESIAN_POINT('Ctrl Pts',(-8.00848556937946,-1.1469007727004,22.9157567581687));
#24259=CARTESIAN_POINT('Ctrl Pts',(-7.2290933909427,-0.418702454117604,
22.9555251110478));
#24260=CARTESIAN_POINT('Ctrl Pts',(-7.46167925127839,0.843872840803867,
23.0032471345026));
#24261=CARTESIAN_POINT('Ctrl Pts',(-8.64770918704739,1.32885234309821,23.0509691579575));
#24262=CARTESIAN_POINT('Ctrl Pts',(-9.69828838525392,0.595261534485202,
23.0986911814123));
#24263=CARTESIAN_POINT('Ctrl Pts',(-9.64793836111807,-0.687570267756874,
23.1464132048672));
#24264=CARTESIAN_POINT('Ctrl Pts',(-8.72766008966769,-1.22684094384785,
23.1861815577462));
#24265=CARTESIAN_POINT('Ctrl Pts',(-7.97034588813662,-1.04966561786637,
23.2179962400495));
#24266=CARTESIAN_POINT('Ctrl Pts',(-7.37789757206185,-0.545759983091795,
23.2498109223527));
#24267=CARTESIAN_POINT('Ctrl Pts',(-7.26492446411792,0.514882292077699,
23.2895792752318));
#24268=CARTESIAN_POINT('Ctrl Pts',(-8.26689470335111,1.31753302400601,23.3373012986866));
#24269=CARTESIAN_POINT('Ctrl Pts',(-9.48114564923169,0.908305988469492,
23.3850233221415));
#24270=CARTESIAN_POINT('Ctrl Pts',(-9.79567664876958,-0.333846327679993,
23.4327453455963));
#24271=CARTESIAN_POINT('Ctrl Pts',(-8.9182694598961,-1.271049178021,23.4804673690513));
#24272=CARTESIAN_POINT('Ctrl Pts',(-7.86947252162285,-1.07675573689688,
23.5202357219303));
#24273=CARTESIAN_POINT('Ctrl Pts',(-7.4126732243127,-0.447271584630692,
23.5520504042335));
#24274=CARTESIAN_POINT('Ctrl Pts',(-7.29432705639192,0.321435173838232,
23.5838650865367));
#24275=CARTESIAN_POINT('Ctrl Pts',(-7.90284665879995,1.19746534025971,23.6236334394159));
#24276=CARTESIAN_POINT('Ctrl Pts',(-9.18574743946922,1.14890460784766,23.6713554628707));
#24277=CARTESIAN_POINT('Ctrl Pts',(-9.83628012328246,0.0449664965947858,
23.7190774863255));
#24278=CARTESIAN_POINT('Ctrl Pts',(-9.26143115070254,-1.10020632220142,
23.7667995097804));
#24279=CARTESIAN_POINT('Ctrl Pts',(-7.98469697473584,-1.23490005513938,
23.8145215332353));
#24280=CARTESIAN_POINT('Ctrl Pts',(-7.31866291190331,-0.40175925902985,
23.8542898861143));
#24281=CARTESIAN_POINT('Ctrl Pts',(-7.38506514261205,0.373164375745999,
23.8861045684176));
#24282=CARTESIAN_POINT('Ctrl Pts',(-7.79851409376019,1.03193281819888,23.9179192507208));
#24283=CARTESIAN_POINT('Ctrl Pts',(-8.83187714157381,1.29629198752846,23.9576876035999));
#24284=CARTESIAN_POINT('Ctrl Pts',(-9.77030285294977,0.420192825331216,
24.0054096270547));
#24285=CARTESIAN_POINT('Ctrl Pts',(-9.5399869115765,-0.840293863743771,
24.0531316505096));
#24286=CARTESIAN_POINT('Ctrl Pts',(-8.35599302339332,-1.33022304120804,
24.1008536739645));
#24287=CARTESIAN_POINT('Ctrl Pts',(-7.30233129222316,-0.596745356447589,
24.1485756974192));
#24288=CARTESIAN_POINT('Ctrl Pts',(-7.34374728727658,0.469092189498782,
24.1883440502984));
#24289=CARTESIAN_POINT('Ctrl Pts',(-7.90098039951627,1.01168518116105,24.2201587326016));
#24290=CARTESIAN_POINT('Ctrl Pts',(-8.64467085179622,1.23937006683619,24.2519734149049));
#24291=CARTESIAN_POINT('Ctrl Pts',(-9.59911972185314,0.763184899656127,
24.2917417677839));
#24292=CARTESIAN_POINT('Ctrl Pts',(-9.73559406180045,-0.513360168999922,
24.3394637912387));
#24293=CARTESIAN_POINT('Ctrl Pts',(-8.73670698711347,-1.31591654596616,
24.3871858146937));
#24294=CARTESIAN_POINT('Ctrl Pts',(-7.52075734081801,-0.911764861743639,
24.4349078381485));
#24295=CARTESIAN_POINT('Ctrl Pts',(-7.20382115093774,0.332318740478653,
24.4826298616033));
#24296=CARTESIAN_POINT('Ctrl Pts',(-7.9324971813356,1.11126431092559,24.5223982144824));
#24297=CARTESIAN_POINT('Ctrl Pts',(-8.70891373351908,1.15701617944249,24.5542128967856));
#24298=CARTESIAN_POINT('Ctrl Pts',(-9.42030153035235,0.842622638646819,
24.5860275790888));
#24299=CARTESIAN_POINT('Ctrl Pts',(-9.83054873707127,-0.141969758426454,
24.625795931968));
#24300=CARTESIAN_POINT('Ctrl Pts',(-9.09854137120265,-1.19665349020969,
24.6735179554228));
#24301=CARTESIAN_POINT('Ctrl Pts',(-7.81803397842269,-1.15003865113736,
24.7212399788777));
#24302=CARTESIAN_POINT('Ctrl Pts',(-7.16289595136489,-0.0488273672827691,
24.7689620023325));
#24303=CARTESIAN_POINT('Ctrl Pts',(-7.73718959054251,1.09937965837695,24.8166840257874));
#24304=CARTESIAN_POINT('Ctrl Pts',(-8.79790093066177,1.21170246077156,24.8564523786664));
#24305=CARTESIAN_POINT('Ctrl Pts',(-9.41500300984422,0.738309474082921,
24.8882670609697));
#24306=CARTESIAN_POINT('Ctrl Pts',(-9.74729132465791,0.0351022700416287,
24.9200817432729));
#24307=CARTESIAN_POINT('Ctrl Pts',(-9.41334407924803,-0.977915102108688,
24.9598500961519));
#24308=CARTESIAN_POINT('Ctrl Pts',(-8.16970373710478,-1.29658618201399,
25.0075721196068));
#24309=CARTESIAN_POINT('Ctrl Pts',(-7.23181487625983,-0.423524551377999,
25.0552941430617));
#24310=CARTESIAN_POINT('Ctrl Pts',(-7.45686390580615,0.837913144461989,
25.1030161665166));
#24311=CARTESIAN_POINT('Ctrl Pts',(-8.64242303887271,1.33050029388494,25.1507381899714));
#24312=CARTESIAN_POINT('Ctrl Pts',(-9.51807995467424,0.721443708004637,
25.1905065428505));
#24313=CARTESIAN_POINT('Ctrl Pts',(-9.67503439547865,-0.040318196719616,
25.2223212251537));
#24314=CARTESIAN_POINT('Ctrl Pts',(-9.46623488155447,-0.789530222091854,
25.2541359074569));
#24315=CARTESIAN_POINT('Ctrl Pts',(-8.55089024838259,-1.33713332792553,
25.293904260336));
#24316=CARTESIAN_POINT('Ctrl Pts',(-7.40188333764438,-0.764441720819265,
25.3416262837908));
#24317=CARTESIAN_POINT('Ctrl Pts',(-7.26382759980121,0.509454954517635,
25.3893483072458));
#24318=CARTESIAN_POINT('Ctrl Pts',(-8.25935377861649,1.31617656292992,25.4370703307005));
#24319=CARTESIAN_POINT('Ctrl Pts',(-9.47822620159528,0.913010872083186,
25.4847923541555));
#24320=CARTESIAN_POINT('Ctrl Pts',(-9.7419517619337,-0.120514061249036,
25.5245607070345));
#24321=CARTESIAN_POINT('Ctrl Pts',(-9.36224431681492,-0.799291014377719,
25.5563753893377));
#24322=CARTESIAN_POINT('Ctrl Pts',(-8.71414535053657,-1.22927197428909,
25.588190071641));
#24323=CARTESIAN_POINT('Ctrl Pts',(-7.66362775939689,-1.04450793638833,
25.62795842452));
#24324=CARTESIAN_POINT('Ctrl Pts',(-7.16938751840154,0.140363002556102,
25.6756804479749));
#24325=CARTESIAN_POINT('Ctrl Pts',(-7.89846615891949,1.19407855341712,25.7234024714298));
#24326=CARTESIAN_POINT('Ctrl Pts',(-9.17915708620039,1.15281264780359,25.7711244948846));
#24327=CARTESIAN_POINT('Ctrl Pts',(-9.83715058751881,0.050434713519313,
25.8188465183394));
#24328=CARTESIAN_POINT('Ctrl Pts',(-9.36038033315174,-0.903722025987354,
25.8586148712185));
#24329=CARTESIAN_POINT('Ctrl Pts',(-8.62911585993756,-1.16861477068243,
25.8904295535218));
#24330=CARTESIAN_POINT('Ctrl Pts',(-7.85766138328856,-1.06975180271418,
25.922244235825));
#24331=CARTESIAN_POINT('Ctrl Pts',(-7.18409118329007,-0.24269186252281,
25.9620125887041));
#24332=CARTESIAN_POINT('Ctrl Pts',(-7.58555644723375,0.976741694347291,
26.0097346121589));
#24333=CARTESIAN_POINT('Ctrl Pts',(-8.82634847073002,1.29659678749717,26.0574566356138));
#24334=CARTESIAN_POINT('Ctrl Pts',(-9.76787582459831,0.427460222794269,
26.1051786590687));
#24335=CARTESIAN_POINT('Ctrl Pts',(-9.54422294215118,-0.836728032944274,
26.1529006825235));
#24336=CARTESIAN_POINT('Ctrl Pts',(-8.55937920581306,-1.24637150474729,
26.1926690354026));
#24337=CARTESIAN_POINT('Ctrl Pts',(-7.83304427880943,-0.968246587143855,
26.2244837177057));
#24338=CARTESIAN_POINT('Ctrl Pts',(-7.31431322586505,-0.388734731623603,
26.2562984000091));
#24339=CARTESIAN_POINT('Ctrl Pts',(-7.34605141627337,0.677434882586455,
26.2960667528881));
#24340=CARTESIAN_POINT('Ctrl Pts',(-8.4475105351465,1.33696529676412,26.343788776343));
#24341=CARTESIAN_POINT('Ctrl Pts',(-9.595138070366,0.767032698475656,26.3915107997978));
#24342=CARTESIAN_POINT('Ctrl Pts',(-9.73851351856959,-0.506276222029613,
26.4392328232527));
#24343=CARTESIAN_POINT('Ctrl Pts',(-8.74224354725321,-1.31599142012546,
26.4869548467075));
#24344=CARTESIAN_POINT('Ctrl Pts',(-7.72943110998268,-0.981423152196046,
26.5267231995866));
#24345=CARTESIAN_POINT('Ctrl Pts',(-7.36210918245529,-0.295864622575958,
26.5585378818898));
#24346=CARTESIAN_POINT('Ctrl Pts',(-7.34897949659139,0.48178793951492,26.5903525641931));
#24347=CARTESIAN_POINT('Ctrl Pts',(-8.07055392035829,1.26731662133423,26.6301209170721));
#24348=CARTESIAN_POINT('Ctrl Pts',(-9.33505288858864,1.0454271959022,26.677842940527));
#24349=CARTESIAN_POINT('Ctrl Pts',(-9.83005513359837,-0.136454737127118,
26.7255649639818));
#24350=CARTESIAN_POINT('Ctrl Pts',(-9.10538409730576,-1.1932063708351,26.7732869874367));
#24351=CARTESIAN_POINT('Ctrl Pts',(-7.82217203182808,-1.15371772960008,
26.8210090108916));
#24352=CARTESIAN_POINT('Ctrl Pts',(-7.27513023062585,-0.238037530659098,
26.8607773637706));
#24353=CARTESIAN_POINT('Ctrl Pts',(-7.44588830282998,0.520749380637105,
26.8925920460739));
#24354=CARTESIAN_POINT('Ctrl Pts',(-7.94476061870995,1.11744218973226,26.9244067283771));
#24355=CARTESIAN_POINT('Ctrl Pts',(-9.00440853628265,1.23938992353288,26.9641750812562));
#24356=CARTESIAN_POINT('Ctrl Pts',(-9.81551250449702,0.244250279803835,
27.011897104711));
#24357=CARTESIAN_POINT('Ctrl Pts',(-9.41657915220431,-0.973421394587272,
27.0596191281659));
#24358=CARTESIAN_POINT('Ctrl Pts',(-8.17713394900972,-1.29845633803764,
27.1073411516208));
#24359=CARTESIAN_POINT('Ctrl Pts',(-7.23253714937687,-0.429014307826603,
27.1550631750756));
#24360=CARTESIAN_POINT('Ctrl Pts',(-7.4179452293806,0.621389806247837,27.1948315279547));
#24361=CARTESIAN_POINT('Ctrl Pts',(-8.04353987513476,1.08350151912796,27.2266462102579));
#24362=CARTESIAN_POINT('Ctrl Pts',(-8.81121725181817,1.20835079347835,27.2584608925612));
#24363=CARTESIAN_POINT('Ctrl Pts',(-9.69236734058681,0.607268868897116,
27.2982292454402));
#24364=CARTESIAN_POINT('Ctrl Pts',(-9.65466851088711,-0.675997025613207,
27.3459512688951));
#24365=CARTESIAN_POINT('Ctrl Pts',(-8.55627692118636,-1.33585158675565,
27.3936732923499));
#24366=CARTESIAN_POINT('Ctrl Pts',(-7.40627885639209,-0.770717463599528,
27.4413953158048));
#24367=CARTESIAN_POINT('Ctrl Pts',(-7.26078198928205,0.504830739893935,
27.4891173392597));
#24368=CARTESIAN_POINT('Ctrl Pts',(-8.08825474279979,1.17789373930847,27.5288856921387));
#24369=CARTESIAN_POINT('Ctrl Pts',(-8.86371272692307,1.11805386266439,27.5607003744419));
#24370=CARTESIAN_POINT('Ctrl Pts',(-9.52595754148374,0.71019641015823,27.5925150567452));
#24371=CARTESIAN_POINT('Ctrl Pts',(-9.79905498496199,-0.320891726404749,
27.6322834096242));
#24372=CARTESIAN_POINT('Ctrl Pts',(-8.93093128646595,-1.26670027039429,
27.6800054330791));
#24373=CARTESIAN_POINT('Ctrl Pts',(-7.66854006482953,-1.04706300187818,
27.727727456534));
#24374=CARTESIAN_POINT('Ctrl Pts',(-7.16860555779351,0.132741055946924,
27.7754494799888));
#24375=CARTESIAN_POINT('Ctrl Pts',(-7.89313737966605,1.19257415453759,27.8231715034437));
#24376=CARTESIAN_POINT('Ctrl Pts',(-8.95928733467085,1.16018229694298,27.8629398563227));
#24377=CARTESIAN_POINT('Ctrl Pts',(-9.50657803978175,0.607562373237274,
27.894754538626));
#24378=CARTESIAN_POINT('Ctrl Pts',(-9.74055034314229,-0.134174006642727,
27.9265692209292));
#24379=CARTESIAN_POINT('Ctrl Pts',(-9.27246195129652,-1.09261973615198,
27.9663375738083));
#24380=CARTESIAN_POINT('Ctrl Pts',(-7.99711792174184,-1.23989554561622,
28.0140595972632));
#24381=CARTESIAN_POINT('Ctrl Pts',(-7.18613440507626,-0.247838157214425,
28.061781620718));
#24382=CARTESIAN_POINT('Ctrl Pts',(-7.5799782078733,0.971489192263182,28.1095036441729));
#24383=CARTESIAN_POINT('Ctrl Pts',(-8.82133426723954,1.29894558882478,28.1572256676277));
#24384=CARTESIAN_POINT('Ctrl Pts',(-9.60642040105378,0.57688968968145,28.1969940205068));
#24385=CARTESIAN_POINT('Ctrl Pts',(-9.65874324301241,-0.19911173827254,
28.22880870281));
#24386=CARTESIAN_POINT('Ctrl Pts',(-9.35038309111296,-0.913135486265807,
28.2606233851133));
#24387=CARTESIAN_POINT('Ctrl Pts',(-8.36929884635634,-1.33170288070013,
28.3003917379923));
#24388=CARTESIAN_POINT('Ctrl Pts',(-7.30845623048737,-0.608649976596389,
28.3481137614472));
#24389=CARTESIAN_POINT('Ctrl Pts',(-7.3442294973634,0.672206143179074,28.395835784902));
#24390=CARTESIAN_POINT('Ctrl Pts',(-8.43985537167285,1.33664279908731,28.4435578083569));
#24391=CARTESIAN_POINT('Ctrl Pts',(-9.59288283354739,0.77208967496468,28.4912798318118));
#24392=CARTESIAN_POINT('Ctrl Pts',(-9.71418086973746,-0.287632810134326,
28.5310481846908));
#24393=CARTESIAN_POINT('Ctrl Pts',(-9.24602881059754,-0.908720199684553,
28.5628628669941));
#24394=CARTESIAN_POINT('Ctrl Pts',(-8.54565972958893,-1.24694948055712,
28.5946775492973));
#24395=CARTESIAN_POINT('Ctrl Pts',(-7.52985168590447,-0.921589714816851,
28.6344459021763));
#24396=CARTESIAN_POINT('Ctrl Pts',(-7.20066421359191,0.319308413860887,
28.6821679256312));
#24397=CARTESIAN_POINT('Ctrl Pts',(-8.0657550343786,1.26455441305737,28.7298899490861));
#24398=CARTESIAN_POINT('Ctrl Pts',(-9.32905264186954,1.05019191790068,28.7776119725409));
#24399=CARTESIAN_POINT('Ctrl Pts',(-9.83165827738984,-0.131154827519194,
28.8253339959958));
#24400=CARTESIAN_POINT('Ctrl Pts',(-9.23003622620806,-1.01193622592216,
28.8651023488749));
#24401=CARTESIAN_POINT('Ctrl Pts',(-8.46963028970779,-1.1753335976729,28.8969170311781));
#24402=CARTESIAN_POINT('Ctrl Pts',(-7.71867754763184,-0.972883886508505,
28.9287317134813));
#24403=CARTESIAN_POINT('Ctrl Pts',(-7.16334539739647,-0.0622076783419375,
28.9685000663604));
#24404=CARTESIAN_POINT('Ctrl Pts',(-7.72628974401962,1.09160606477463,29.0162220898152));
#24405=CARTESIAN_POINT('Ctrl Pts',(-8.99897214403931,1.24044081982536,29.0639441132701));
#24406=CARTESIAN_POINT('Ctrl Pts',(-9.81409218726597,0.251779422282355,
29.111666136725));
#24407=CARTESIAN_POINT('Ctrl Pts',(-9.42125928897337,-0.970462165325127,
29.1593881601799));
#24408=CARTESIAN_POINT('Ctrl Pts',(-8.39000353594678,-1.24292755198914,
29.1991565130589));
#24409=CARTESIAN_POINT('Ctrl Pts',(-7.70803711420451,-0.868979538690246,
29.2309711953621));
#24410=CARTESIAN_POINT('Ctrl Pts',(-7.2725841095908,-0.224544184030418,
29.2627858776653));
#24411=CARTESIAN_POINT('Ctrl Pts',(-7.44845097068834,0.827500878887188,
29.3025542305445));
#24412=CARTESIAN_POINT('Ctrl Pts',(-8.62909116778061,1.33175184955349,29.3502762539992));
#24413=CARTESIAN_POINT('Ctrl Pts',(-9.68894861733642,0.611622684002498,
29.3979982774542));
#24414=CARTESIAN_POINT('Ctrl Pts',(-9.65851111003362,-0.669377881206477,
29.445720300909));
#24415=CARTESIAN_POINT('Ctrl Pts',(-8.56177118348423,-1.33666768258405,
29.4934423243639));
#24416=CARTESIAN_POINT('Ctrl Pts',(-7.60356077414914,-0.868013858452832,
29.533210677243));
#24417=CARTESIAN_POINT('Ctrl Pts',(-7.33256413054386,-0.138985158650351,
29.5650253595461));
#24418=CARTESIAN_POINT('Ctrl Pts',(-7.42474175056611,0.633214111788515,
29.5968400418494));
#24419=CARTESIAN_POINT('Ctrl Pts',(-8.24640486169936,1.31390426831433,29.6366083947285));
#24420=CARTESIAN_POINT('Ctrl Pts',(-9.46858362546016,0.922516240590384,
29.6843304181833));
#24421=CARTESIAN_POINT('Ctrl Pts',(-9.8000120392334,-0.315061926833937,
29.7320524416382));
#24422=CARTESIAN_POINT('Ctrl Pts',(-8.93684997703512,-1.26478329921426,
29.7797744650931));
#24423=CARTESIAN_POINT('Ctrl Pts',(-7.88515752754028,-1.08587738685972,
29.8195428179721));
#24424=CARTESIAN_POINT('Ctrl Pts',(-7.41918288393529,-0.462897910902516,
29.8513575002754));
#24425=CARTESIAN_POINT('Ctrl Pts',(-7.29010085348255,0.303653650183876,
29.8831721825785));
#24426=CARTESIAN_POINT('Ctrl Pts',(-7.8848103649759,1.18921135372836,29.9229405354577));
#24427=CARTESIAN_POINT('Ctrl Pts',(-9.17027425724991,1.15778987946344,29.9706625589125));
#24428=CARTESIAN_POINT('Ctrl Pts',(-9.72243084515013,0.248331434474197,
30.0104309117915));
#24429=CARTESIAN_POINT('Ctrl Pts',(-9.55852849210566,-0.515011305712282,
30.0422455940948));
#24430=CARTESIAN_POINT('Ctrl Pts',(-9.31003111705877,-0.811448288777166,
30.0581529352464));
#24431=CARTESIAN_POINT('Ctrl Pts',(-9.15663776199785,-0.920831852263732,
30.0661066058222));
#24432=CARTESIAN_POINT('Ctrl Pts',(-9.0118388111672,1.0723337549513,1.79999999999999));
#24433=CARTESIAN_POINT('Ctrl Pts',(-9.19046954816081,0.987070987050382,
1.8079536705758));
#24434=CARTESIAN_POINT('Ctrl Pts',(-9.50155426450738,0.725568290707912,
1.82386101172742));
#24435=CARTESIAN_POINT('Ctrl Pts',(-9.81008998255101,-0.0344549071383838,
1.85567569403066));
#24436=CARTESIAN_POINT('Ctrl Pts',(-9.40429116407483,-1.07600298498373,
1.89544404690971));
#24437=CARTESIAN_POINT('Ctrl Pts',(-8.07989827787013,-1.34249070178545,
1.94316607036458));
#24438=CARTESIAN_POINT('Ctrl Pts',(-7.30334704707155,-0.534421386282276,
1.98293442324363));
#24439=CARTESIAN_POINT('Ctrl Pts',(-7.29738792476634,0.282249903129412,
2.01474910554687));
#24440=CARTESIAN_POINT('Ctrl Pts',(-7.66615515840917,1.01168221201408,2.04656378785011));
#24441=CARTESIAN_POINT('Ctrl Pts',(-8.72181247099373,1.38822684395207,2.08633214072916));
#24442=CARTESIAN_POINT('Ctrl Pts',(-9.78781926187509,0.562627888122653,
2.13405416418403));
#24443=CARTESIAN_POINT('Ctrl Pts',(-9.67013820971537,-0.778260502859383,
2.18177618763889));
#24444=CARTESIAN_POINT('Ctrl Pts',(-8.4767481821154,-1.40569864308939,2.22949821109375));
#24445=CARTESIAN_POINT('Ctrl Pts',(-7.50264969202872,-0.850921733780454,
2.2692665639728));
#24446=CARTESIAN_POINT('Ctrl Pts',(-7.26671790307987,-0.0686793482260387,
2.30108124627604));
#24447=CARTESIAN_POINT('Ctrl Pts',(-7.41443229219623,0.734996509964761,
2.33289592857928));
#24448=CARTESIAN_POINT('Ctrl Pts',(-8.32062191059588,1.39433769122372,2.37266428145833));
#24449=CARTESIAN_POINT('Ctrl Pts',(-9.57691242085731,0.903494929509702,
2.4203863049132));
#24450=CARTESIAN_POINT('Ctrl Pts',(-9.84156959790808,-0.416458701888548,
2.46810832836806));
#24451=CARTESIAN_POINT('Ctrl Pts',(-8.87597493033133,-1.35451113192682,
2.51583035182292));
#24452=CARTESIAN_POINT('Ctrl Pts',(-7.5625456899844,-1.04764123587607,2.56355237527778));
#24453=CARTESIAN_POINT('Ctrl Pts',(-7.18908148385554,0.00893409317419132,
2.60332072815684));
#24454=CARTESIAN_POINT('Ctrl Pts',(-7.52236165481741,0.755012087082508,
2.63513541046008));
#24455=CARTESIAN_POINT('Ctrl Pts',(-8.15995042754744,1.26607722708645,2.66695009276332));
#24456=CARTESIAN_POINT('Ctrl Pts',(-9.27661796922437,1.17185321198702,2.70671844564237));
#24457=CARTESIAN_POINT('Ctrl Pts',(-9.90556259985949,-0.0213388321026141,
2.75444046909723));
#24458=CARTESIAN_POINT('Ctrl Pts',(-9.24208297580843,-1.19270436179778,
2.8021624925521));
#24459=CARTESIAN_POINT('Ctrl Pts',(-7.89810602223727,-1.27034854887012,
2.84988451600696));
#24460=CARTESIAN_POINT('Ctrl Pts',(-7.10559639405835,-0.178924052943307,
2.89760653946182));
#24461=CARTESIAN_POINT('Ctrl Pts',(-7.51445941986352,0.864462087680646,
2.93737489234087));
#24462=CARTESIAN_POINT('Ctrl Pts',(-8.25464604367347,1.21062885803132,2.96918957464412));
#24463=CARTESIAN_POINT('Ctrl Pts',(-9.07120418959933,1.17996215792738,3.00100425694735));
#24464=CARTESIAN_POINT('Ctrl Pts',(-9.85403869080924,0.378093235837854,
3.04077260982641));
#24465=CARTESIAN_POINT('Ctrl Pts',(-9.54899988060095,-0.935767616312688,
3.08849463328127));
#24466=CARTESIAN_POINT('Ctrl Pts',(-8.2808413597343,-1.38751585434482,3.13621665673613));
#24467=CARTESIAN_POINT('Ctrl Pts',(-7.21365340752345,-0.566898780222384,
3.183938680191));
#24468=CARTESIAN_POINT('Ctrl Pts',(-7.32841139752292,0.777016997712263,
3.23166070364585));
#24469=CARTESIAN_POINT('Ctrl Pts',(-8.32028099515215,1.29857075310548,3.27142905652491));
#24470=CARTESIAN_POINT('Ctrl Pts',(-9.10653920532774,1.07607201936986,3.30324373882815));
#24471=CARTESIAN_POINT('Ctrl Pts',(-9.70399944158484,0.518623433827907,
3.33505842113139));
#24472=CARTESIAN_POINT('Ctrl Pts',(-9.77137469231307,-0.599984716647835,
3.37482677401044));
#24473=CARTESIAN_POINT('Ctrl Pts',(-8.681056610743,-1.3940158845331,3.4225487974653));
#24474=CARTESIAN_POINT('Ctrl Pts',(-7.42643816511771,-0.905922591771324,
3.47027082092017));
#24475=CARTESIAN_POINT('Ctrl Pts',(-7.15628619215633,0.412910384032477,
3.51799284437503));
#24476=CARTESIAN_POINT('Ctrl Pts',(-8.12236807704563,1.35416741919452,3.56571486782989));
#24477=CARTESIAN_POINT('Ctrl Pts',(-9.21371438567086,1.09963480172637,3.60548322070895));
#24478=CARTESIAN_POINT('Ctrl Pts',(-9.66274853496778,0.416937216961904,
3.63729790301218));
#24479=CARTESIAN_POINT('Ctrl Pts',(-9.74985295977625,-0.39554076960521,
3.66911258531543));
#24480=CARTESIAN_POINT('Ctrl Pts',(-9.0689239756906,-1.2855741045648,3.70888093819448));
#24481=CARTESIAN_POINT('Ctrl Pts',(-7.7248494450175,-1.17269066668865,3.75660296164935));
#24482=CARTESIAN_POINT('Ctrl Pts',(-7.09538923568223,0.0173019179194368,
3.8043249851042));
#24483=CARTESIAN_POINT('Ctrl Pts',(-7.7539705342453,1.19142847827895,3.85204700855907));
#24484=CARTESIAN_POINT('Ctrl Pts',(-9.10041781121801,1.27117021693212,3.89976903201393));
#24485=CARTESIAN_POINT('Ctrl Pts',(-9.75921675296556,0.364634187278776,
3.93953738489298));
#24486=CARTESIAN_POINT('Ctrl Pts',(-9.65212567573532,-0.4454517098057,3.97135206719623));
#24487=CARTESIAN_POINT('Ctrl Pts',(-9.18641146043698,-1.1168814746706,4.00316674949946));
#24488=CARTESIAN_POINT('Ctrl Pts',(-8.08912659919642,-1.34445465410894,
4.04293510237852));
#24489=CARTESIAN_POINT('Ctrl Pts',(-7.14652302700508,-0.379686536765321,
4.09065712583338));
#24490=CARTESIAN_POINT('Ctrl Pts',(-7.449078725721,0.932091857527417,4.13837914928824));
#24491=CARTESIAN_POINT('Ctrl Pts',(-8.71533928644708,1.38913310173676,4.1861011727431));
#24492=CARTESIAN_POINT('Ctrl Pts',(-9.7857678498451,0.568485975858496,4.23382319619797));
#24493=CARTESIAN_POINT('Ctrl Pts',(-9.69085931574868,-0.548123171902275,
4.27359154907701));
#24494=CARTESIAN_POINT('Ctrl Pts',(-9.07984920094099,-1.09068588632358,
4.30540623138026));
#24495=CARTESIAN_POINT('Ctrl Pts',(-8.28834893264812,-1.29374987813349,
4.33722091368349));
#24496=CARTESIAN_POINT('Ctrl Pts',(-7.30962727695085,-0.747922488406148,
4.37698926656256));
#24497=CARTESIAN_POINT('Ctrl Pts',(-7.22800764477856,0.598412258302363,
4.42471129001741));
#24498=CARTESIAN_POINT('Ctrl Pts',(-8.31508535771834,1.39249320668754,4.47243331347228));
#24499=CARTESIAN_POINT('Ctrl Pts',(-9.57173156659136,0.909644563442217,
4.52015533692714));
#24500=CARTESIAN_POINT('Ctrl Pts',(-9.84431460056008,-0.411331403085193,
4.567877360382));
#24501=CARTESIAN_POINT('Ctrl Pts',(-9.04196587069652,-1.19367412491089,
4.60764571326105));
#24502=CARTESIAN_POINT('Ctrl Pts',(-8.22490009151298,-1.20421793659114,
4.63946039556429));
#24503=CARTESIAN_POINT('Ctrl Pts',(-7.49346489460161,-0.839923807902976,
4.67127507786754));
#24504=CARTESIAN_POINT('Ctrl Pts',(-7.11042675183102,0.213216923381422,
4.71104343074659));
#24505=CARTESIAN_POINT('Ctrl Pts',(-7.92958008831927,1.28478905155145,4.75876545420144));
#24506=CARTESIAN_POINT('Ctrl Pts',(-9.27123664979505,1.17406336524653,4.80648747765632));
#24507=CARTESIAN_POINT('Ctrl Pts',(-9.90566182547761,-0.0132896585079293,
4.85420950111116));
#24508=CARTESIAN_POINT('Ctrl Pts',(-9.24751691120311,-1.19062745470968,
4.90193152456605));
#24509=CARTESIAN_POINT('Ctrl Pts',(-8.1288676629186,-1.25731686931103,4.94169987744508));
#24510=CARTESIAN_POINT('Ctrl Pts',(-7.50406036051186,-0.730701740078402,
4.97351455974834));
#24511=CARTESIAN_POINT('Ctrl Pts',(-7.18926003595645,0.0233595406788859,
5.00532924205156));
#24512=CARTESIAN_POINT('Ctrl Pts',(-7.58863395692623,1.07041450101124,5.04509759493063));
#24513=CARTESIAN_POINT('Ctrl Pts',(-8.90922845059994,1.3448397145563,5.09281961838548));
#24514=CARTESIAN_POINT('Ctrl Pts',(-9.85141519694107,0.383285430296794,
5.14054164184035));
#24515=CARTESIAN_POINT('Ctrl Pts',(-9.55434127955645,-0.929745260193144,
5.18826366529521));
#24516=CARTESIAN_POINT('Ctrl Pts',(-8.28630969195433,-1.3895005292156,5.23598568875008));
#24517=CARTESIAN_POINT('Ctrl Pts',(-7.39669400474826,-0.708025989864192,
5.27575404162911));
#24518=CARTESIAN_POINT('Ctrl Pts',(-7.26873458964617,0.0990267020737063,
5.30756872393238));
#24519=CARTESIAN_POINT('Ctrl Pts',(-7.52403220505333,0.875255268312366,
5.3393834062356));
#24520=CARTESIAN_POINT('Ctrl Pts',(-8.51112605556492,1.40579211810661,5.37915175911467));
#24521=CARTESIAN_POINT('Ctrl Pts',(-9.68938066093212,0.749289947903339,
5.42687378256952));
#24522=CARTESIAN_POINT('Ctrl Pts',(-9.77278781043502,-0.594341606493356,
5.47459580602438));
#24523=CARTESIAN_POINT('Ctrl Pts',(-8.68903636181648,-1.39295622204702,
5.52231782947925));
#24524=CARTESIAN_POINT('Ctrl Pts',(-7.42927507874336,-0.911001323513343,
5.5700398529341));
#24525=CARTESIAN_POINT('Ctrl Pts',(-7.20237469211957,0.186422857584081,
5.60980820581317));
#24526=CARTESIAN_POINT('Ctrl Pts',(-7.63364252939566,0.880480284609163,
5.6416228881164));
#24527=CARTESIAN_POINT('Ctrl Pts',(-8.33458219270634,1.30046986528399,5.67343757041965));
#24528=CARTESIAN_POINT('Ctrl Pts',(-9.42819427600473,1.05585541360318,5.7132059232987));
#24529=CARTESIAN_POINT('Ctrl Pts',(-9.88971769783222,-0.211533692257875,
5.76092794675356));
#24530=CARTESIAN_POINT('Ctrl Pts',(-9.07368481902778,-1.28223105718826,
5.80864997020842));
#24531=CARTESIAN_POINT('Ctrl Pts',(-7.73157747309663,-1.17711027638694,
5.85637199366328));
#24532=CARTESIAN_POINT('Ctrl Pts',(-7.09421175387495,0.0116049773688213,
5.90409401711815));
#24533=CARTESIAN_POINT('Ctrl Pts',(-7.64063909944886,0.98999180000924,5.94386236999719));
#24534=CARTESIAN_POINT('Ctrl Pts',(-8.42089398251533,1.23270557573781,5.97567705230044));
#24535=CARTESIAN_POINT('Ctrl Pts',(-9.22577226286207,1.09171403945432,6.00749173460368));
#24536=CARTESIAN_POINT('Ctrl Pts',(-9.89277395110486,0.191196206988666,
6.04726008748273));
#24537=CARTESIAN_POINT('Ctrl Pts',(-9.41257658626577,-1.06923606225557,
6.0949821109376));
#24538=CARTESIAN_POINT('Ctrl Pts',(-8.09491428823142,-1.34504138290316,
6.14270413439245));
#24539=CARTESIAN_POINT('Ctrl Pts',(-7.14871946308653,-0.38743088827196,
6.19042615784733));
#24540=CARTESIAN_POINT('Ctrl Pts',(-7.44446086304004,0.928553928853288,
6.23814818130217));
#24541=CARTESIAN_POINT('Ctrl Pts',(-8.49783623871218,1.31094631454484,6.27791653418124));
#24542=CARTESIAN_POINT('Ctrl Pts',(-9.24670909380938,0.983995085190856,
6.30973121648447));
#24543=CARTESIAN_POINT('Ctrl Pts',(-9.76315317478435,0.350754869551153,
6.34154589878773));
#24544=CARTESIAN_POINT('Ctrl Pts',(-9.67838557456485,-0.766669880783481,
6.38131425166676));
#24545=CARTESIAN_POINT('Ctrl Pts',(-8.49056044938906,-1.40569295278612,
6.42903627512164));
#24546=CARTESIAN_POINT('Ctrl Pts',(-7.3136203517155,-0.752152966980432,
6.47675829857649));
#24547=CARTESIAN_POINT('Ctrl Pts',(-7.22460174085939,0.591118484916007,
6.52448032203136));
#24548=CARTESIAN_POINT('Ctrl Pts',(-8.30927829155303,1.39283900662287,6.57220234548622));
#24549=CARTESIAN_POINT('Ctrl Pts',(-9.35608819723364,0.992823206839408,
6.61197069836527));
#24550=CARTESIAN_POINT('Ctrl Pts',(-9.70850848082631,0.25559352540361,6.6437853806685));
#24551=CARTESIAN_POINT('Ctrl Pts',(-9.68475530270078,-0.561194969866995,
6.67560006297176));
#24552=CARTESIAN_POINT('Ctrl Pts',(-8.88954205617756,-1.35078949318983,
6.7153684158508));
#24553=CARTESIAN_POINT('Ctrl Pts',(-7.57314603074635,-1.05688386415305,
6.76309043930567));
#24554=CARTESIAN_POINT('Ctrl Pts',(-7.11067861489593,0.207405025237098,
6.81081246276052));
#24555=CARTESIAN_POINT('Ctrl Pts',(-7.92223219994117,1.28150152237267,6.8585344862154));
#24556=CARTESIAN_POINT('Ctrl Pts',(-9.26707128633578,1.17812431861932,6.90625650967024));
#24557=CARTESIAN_POINT('Ctrl Pts',(-9.79700284495402,0.190705379218312,
6.94602486254932));
#24558=CARTESIAN_POINT('Ctrl Pts',(-9.58116800924214,-0.597408180600789,
6.97783954485253));
#24559=CARTESIAN_POINT('Ctrl Pts',(-9.02879708860554,-1.19956598841578,
7.0096542271558));
#24560=CARTESIAN_POINT('Ctrl Pts',(-7.91079937238375,-1.27640819836747,
7.04942258003484));
#24561=CARTESIAN_POINT('Ctrl Pts',(-7.10756676680328,-0.192850910595855,
7.09714460348971));
#24562=CARTESIAN_POINT('Ctrl Pts',(-7.58502182671985,1.06585444504493,7.14486662694456));
#24563=CARTESIAN_POINT('Ctrl Pts',(-8.90152062454935,1.34716107822704,7.19258865039943));
#24564=CARTESIAN_POINT('Ctrl Pts',(-9.85092212321177,0.389081849306921,
7.24031067385429));
#24565=CARTESIAN_POINT('Ctrl Pts',(-9.60563721925922,-0.704380054282014,
7.28007902673334));
#24566=CARTESIAN_POINT('Ctrl Pts',(-8.92676531327588,-1.15917736599793,
7.31189370903659));
#24567=CARTESIAN_POINT('Ctrl Pts',(-8.11505380559897,-1.25315655402578,
7.34370839133982));
#24568=CARTESIAN_POINT('Ctrl Pts',(-7.21928808162424,-0.579786383570173,
7.38347674421888));
#24569=CARTESIAN_POINT('Ctrl Pts',(-7.32078945678287,0.765195581138472,
7.43119876767373));
#24570=CARTESIAN_POINT('Ctrl Pts',(-8.50541082157443,1.4047069013182,7.47892079112861));
#24571=CARTESIAN_POINT('Ctrl Pts',(-9.68507041122039,0.756088555050457,
7.52664281458347));
#24572=CARTESIAN_POINT('Ctrl Pts',(-9.77620739660413,-0.58963543761884,
7.57436483803832));
#24573=CARTESIAN_POINT('Ctrl Pts',(-8.875280791801,-1.25608488916428,7.61413319091738));
#24574=CARTESIAN_POINT('Ctrl Pts',(-8.06431736127027,-1.15585528366093,
7.64594787322062));
#24575=CARTESIAN_POINT('Ctrl Pts',(-7.38896923590437,-0.695841621861376,
7.67776255552386));
#24576=CARTESIAN_POINT('Ctrl Pts',(-7.15211534576237,0.399477442809727,
7.71753090840292));
#24577=CARTESIAN_POINT('Ctrl Pts',(-8.10886945534902,1.350214308793,7.76525293185777));
#24578=CARTESIAN_POINT('Ctrl Pts',(-9.42316207684519,1.05877407197001,7.81297495531264));
#24579=CARTESIAN_POINT('Ctrl Pts',(-9.8909062425691,-0.203572117468501,
7.8606969787675));
#24580=CARTESIAN_POINT('Ctrl Pts',(-9.07935003954765,-1.28090936452164,
7.90841900222236));
#24581=CARTESIAN_POINT('Ctrl Pts',(-7.9619774706096,-1.19545668233942,7.94818735510142));
#24582=CARTESIAN_POINT('Ctrl Pts',(-7.41426180224206,-0.589061426666821,
7.98000203740465));
#24583=CARTESIAN_POINT('Ctrl Pts',(-7.204504785262,0.200691479820453,8.01181671970791));
#24584=CARTESIAN_POINT('Ctrl Pts',(-7.74202742743127,1.18399866878161,8.05158507258693));
#24585=CARTESIAN_POINT('Ctrl Pts',(-9.08762299690323,1.27701252779242,8.09930709604183));
#24586=CARTESIAN_POINT('Ctrl Pts',(-9.89087795044728,0.196695913939951,
8.14702911949667));
#24587=CARTESIAN_POINT('Ctrl Pts',(-9.41868451778527,-1.06399273466032,
8.19475114295154));
#24588=CARTESIAN_POINT('Ctrl Pts',(-8.10006338572175,-1.34774848284193,
8.24247316640639));
#24589=CARTESIAN_POINT('Ctrl Pts',(-7.31095655944527,-0.55205128199777,
8.28224151928546));
#24590=CARTESIAN_POINT('Ctrl Pts',(-7.29349640414644,0.264895963823187,
8.31405620158869));
#24591=CARTESIAN_POINT('Ctrl Pts',(-7.65158564831681,0.999388817898019,
8.34587088389193));
#24592=CARTESIAN_POINT('Ctrl Pts',(-8.70144610447083,1.39132840675256,8.385639236771));
#24593=CARTESIAN_POINT('Ctrl Pts',(-9.77991422991853,0.581275620235635,
8.43336126022583));
#24594=CARTESIAN_POINT('Ctrl Pts',(-9.68055006013832,-0.761270195862498,
8.48108328368072));
#24595=CARTESIAN_POINT('Ctrl Pts',(-8.49861019163866,-1.4057239597663,8.52880530713557));
#24596=CARTESIAN_POINT('Ctrl Pts',(-7.31574317534535,-0.75756916628252,
8.57652733059043));
#24597=CARTESIAN_POINT('Ctrl Pts',(-7.23958642901857,0.360475452100957,
8.61629568346948));
#24598=CARTESIAN_POINT('Ctrl Pts',(-7.76089349654227,0.989718331144719,
8.64811036577273));
#24599=CARTESIAN_POINT('Ctrl Pts',(-8.51226287342945,1.31089074427157,8.67992504807597));
#24600=CARTESIAN_POINT('Ctrl Pts',(-9.56266114340054,0.920394786355142,
8.71969340095502));
#24601=CARTESIAN_POINT('Ctrl Pts',(-9.84825577586161,-0.397829291888031,
8.76741542440989));
#24602=CARTESIAN_POINT('Ctrl Pts',(-8.89471185563952,-1.34812214083839,
8.81513744786473));
#24603=CARTESIAN_POINT('Ctrl Pts',(-7.57921338783839,-1.06217409001174,
8.86285947131962));
#24604=CARTESIAN_POINT('Ctrl Pts',(-7.10874030224357,0.20192008776204,8.91058149477447));
#24605=CARTESIAN_POINT('Ctrl Pts',(-7.78265954393772,1.09727279724685,8.95034984765352));
#24606=CARTESIAN_POINT('Ctrl Pts',(-8.58860010090821,1.23205958483201,8.98216452995677));
#24607=CARTESIAN_POINT('Ctrl Pts',(-9.36696202918395,0.983342138543273,
9.01397921226));
#24608=CARTESIAN_POINT('Ctrl Pts',(-9.90583593214038,0.000774820025180653,
9.05374756513906));
#24609=CARTESIAN_POINT('Ctrl Pts',(-9.25933158494685,-1.18299506623249,
9.10146958859392));
#24610=CARTESIAN_POINT('Ctrl Pts',(-7.91645424282956,-1.27777349514281,
9.14919161204877));
#24611=CARTESIAN_POINT('Ctrl Pts',(-7.10869394244917,-0.200821405359748,
9.19691363550366));
#24612=CARTESIAN_POINT('Ctrl Pts',(-7.57996729233084,1.06297463999009,9.24463565895849));
#24613=CARTESIAN_POINT('Ctrl Pts',(-8.67543136727172,1.29915694081153,9.28440401183757));
#24614=CARTESIAN_POINT('Ctrl Pts',(-9.37311474448176,0.873779973120195,
9.3162186941408));
#24615=CARTESIAN_POINT('Ctrl Pts',(-9.79902295327563,0.17642077072913,9.34803337644404));
#24616=CARTESIAN_POINT('Ctrl Pts',(-9.56367504023093,-0.919222865921435,
9.3878017293231));
#24617=CARTESIAN_POINT('Ctrl Pts',(-8.30023828915245,-1.39145860215371,
9.43552375277796));
#24618=CARTESIAN_POINT('Ctrl Pts',(-7.22267131126601,-0.584518756361346,
9.48324577623282));
#24619=CARTESIAN_POINT('Ctrl Pts',(-7.31642696034088,0.758430380734061,
9.53096779968769));
#24620=CARTESIAN_POINT('Ctrl Pts',(-8.49970411739585,1.4058361145228,9.57868982314254));
#24621=CARTESIAN_POINT('Ctrl Pts',(-9.48268156411455,0.867710703536009,
9.6184581760216));
#24622=CARTESIAN_POINT('Ctrl Pts',(-9.73199174854549,0.0895384273551449,
9.65027285832483));
#24623=CARTESIAN_POINT('Ctrl Pts',(-9.59781881456104,-0.716504551190982,
9.68208754062809));
#24624=CARTESIAN_POINT('Ctrl Pts',(-8.70297963016015,-1.3911055093641,9.72185589350711));
#24625=CARTESIAN_POINT('Ctrl Pts',(-7.43852750076266,-0.921595310313144,
9.76957791696201));
#24626=CARTESIAN_POINT('Ctrl Pts',(-7.15157763261807,0.393684994310346,
9.81729994041685));
#24627=CARTESIAN_POINT('Ctrl Pts',(-8.10114397486295,1.34795239301698,9.86502196387172));
#24628=CARTESIAN_POINT('Ctrl Pts',(-9.4195851832654,1.06336181949601,9.91274398732657));
#24629=CARTESIAN_POINT('Ctrl Pts',(-9.81088102451861,0.0132612608230292,
9.95251234020565));
#24630=CARTESIAN_POINT('Ctrl Pts',(-9.49028095694926,-0.738352507113669,
9.98432702250886));
#24631=CARTESIAN_POINT('Ctrl Pts',(-8.86143529445072,-1.26013866276967,
10.0161417048121));
#24632=CARTESIAN_POINT('Ctrl Pts',(-7.74333299839028,-1.184833455435,10.0559100576912));
#24633=CARTESIAN_POINT('Ctrl Pts',(-7.09427750642714,-0.00246042508328673,
10.103632081146));
#24634=CARTESIAN_POINT('Ctrl Pts',(-7.7378309030877,1.17996992474936,10.1513541046009));
#24635=CARTESIAN_POINT('Ctrl Pts',(-9.08030065280452,1.28035656556405,10.1990761280558));
#24636=CARTESIAN_POINT('Ctrl Pts',(-9.89117457933197,0.202505699336026,
10.2467981515106));
#24637=CARTESIAN_POINT('Ctrl Pts',(-9.50003469113584,-0.847652958472063,
10.2865665043897));
#24638=CARTESIAN_POINT('Ctrl Pts',(-8.76581477537552,-1.20630149782277,
10.3183811866929));
#24639=CARTESIAN_POINT('Ctrl Pts',(-7.94885446861643,-1.18946354493003,
10.3501958689961));
#24640=CARTESIAN_POINT('Ctrl Pts',(-7.15255650481893,-0.400962960555315,
10.3899642218752));
#24641=CARTESIAN_POINT('Ctrl Pts',(-7.43530789219255,0.917873901034805,
10.43768624533));
#24642=CARTESIAN_POINT('Ctrl Pts',(-8.69563654667604,1.39102735314794,10.4854082687849));
#24643=CARTESIAN_POINT('Ctrl Pts',(-9.77656461632702,0.588595415349269,
10.5331302922398));
#24644=CARTESIAN_POINT('Ctrl Pts',(-9.68457560687616,-0.757070604393695,
10.5808523156946));
#24645=CARTESIAN_POINT('Ctrl Pts',(-8.70167808713493,-1.2953419898433,10.6206206685737));
#24646=CARTESIAN_POINT('Ctrl Pts',(-7.91176565610344,-1.08618651948824,
10.6524353508769));
#24647=CARTESIAN_POINT('Ctrl Pts',(-7.30495342912999,-0.538932848259806,
10.6842500331802));
#24648=CARTESIAN_POINT('Ctrl Pts',(-7.21864976666804,0.578374314767913,
10.7240183860592));
#24649=CARTESIAN_POINT('Ctrl Pts',(-8.29536860980847,1.39075079607261,10.7717404095141));
#24650=CARTESIAN_POINT('Ctrl Pts',(-9.55807067299778,0.923968184811093,
10.8194624329689));
#24651=CARTESIAN_POINT('Ctrl Pts',(-9.85051180715808,-0.390102090938935,
10.8671844564238));
#24652=CARTESIAN_POINT('Ctrl Pts',(-8.90050389292981,-1.34758001624808,
10.9149064798787));
#24653=CARTESIAN_POINT('Ctrl Pts',(-7.80500475501606,-1.11156040363594,
10.9546748327577));
#24654=CARTESIAN_POINT('Ctrl Pts',(-7.34447687296949,-0.436562826354961,
10.986489515061));
#24655=CARTESIAN_POINT('Ctrl Pts',(-7.24362965654256,0.374324032840834,
11.0183041973642));
#24656=CARTESIAN_POINT('Ctrl Pts',(-7.90939275771686,1.27575795267197,11.0580725502433));
#24657=CARTESIAN_POINT('Ctrl Pts',(-9.25518577116924,1.18564591411257,11.1057945736981));
#24658=CARTESIAN_POINT('Ctrl Pts',(-9.90470237296531,0.00648066252564181,
11.153516597153));
#24659=CARTESIAN_POINT('Ctrl Pts',(-9.26609346085678,-1.17862741859367,
11.2012386206079));
#24660=CARTESIAN_POINT('Ctrl Pts',(-7.92118919095866,-1.28115311956846,
11.2489606440627));
#24661=CARTESIAN_POINT('Ctrl Pts',(-7.24713698930774,-0.385900502617859,
11.2887289969418));
#24662=CARTESIAN_POINT('Ctrl Pts',(-7.34049794034117,0.425882345377609,
11.320543679245));
#24663=CARTESIAN_POINT('Ctrl Pts',(-7.79477808273445,1.10510043384748,11.3523583615483));
#24664=CARTESIAN_POINT('Ctrl Pts',(-8.88805285710864,1.35121806105931,11.3921267144273));
#24665=CARTESIAN_POINT('Ctrl Pts',(-9.84685488433432,0.402546522992234,
11.4398487378822));
#24666=CARTESIAN_POINT('Ctrl Pts',(-9.5665509948533,-0.914166139702461,
11.487570761337));
#24667=CARTESIAN_POINT('Ctrl Pts',(-8.30820964007592,-1.3925797070432,11.5352927847919));
#24668=CARTESIAN_POINT('Ctrl Pts',(-7.22404091446613,-0.590172585339807,
11.5830148082467));
#24669=CARTESIAN_POINT('Ctrl Pts',(-7.30003162094818,0.527883330630275,
11.6227831611258));
#24670=CARTESIAN_POINT('Ctrl Pts',(-7.90176856145037,1.08071270205741,11.6545978434291));
#24671=CARTESIAN_POINT('Ctrl Pts',(-8.68971751015799,1.29714771241407,11.6864125257323));
#24672=CARTESIAN_POINT('Ctrl Pts',(-9.67753976575011,0.767968338227732,
11.7261808786114));
#24673=CARTESIAN_POINT('Ctrl Pts',(-9.78194118595766,-0.576791624743086,
11.7739029020662));
#24674=CARTESIAN_POINT('Ctrl Pts',(-8.70846308980102,-1.38916301987625,
11.8216249255211));
#24675=CARTESIAN_POINT('Ctrl Pts',(-7.44382234606286,-0.927658636542655,
11.8693469489759));
#24676=CARTESIAN_POINT('Ctrl Pts',(-7.14891421842479,0.38851316485853,11.9170689724308));
#24677=CARTESIAN_POINT('Ctrl Pts',(-7.93790286829016,1.18432754591167,11.9568373253098));
#24678=CARTESIAN_POINT('Ctrl Pts',(-8.75467303594958,1.20870279358393,11.9886520076131));
#24679=CARTESIAN_POINT('Ctrl Pts',(-9.49217091130871,0.856844095640773,
12.0204666899163));
#24680=CARTESIAN_POINT('Ctrl Pts',(-9.89298385872439,-0.189660849350548,
12.0602350427954));
#24681=CARTESIAN_POINT('Ctrl Pts',(-9.09208967290089,-1.27494768593557,
12.1079570662503));
#24682=CARTESIAN_POINT('Ctrl Pts',(-7.74875081289082,-1.18695215340337,
12.1556790897051));
#24683=CARTESIAN_POINT('Ctrl Pts',(-7.0943146441837,-0.0105101413829567,
12.20340111316));
#24684=CARTESIAN_POINT('Ctrl Pts',(-7.73243286823234,1.1778013273354,12.2511231366148));
#24685=CARTESIAN_POINT('Ctrl Pts',(-8.84979273440854,1.26341994777532,12.2908914894939));
#24686=CARTESIAN_POINT('Ctrl Pts',(-9.48342609672741,0.747458300330454,
12.3227061717971));
#24687=CARTESIAN_POINT('Ctrl Pts',(-9.810947582283,-0.00116532738706759,
12.3545208541004));
#24688=CARTESIAN_POINT('Ctrl Pts',(-9.42935757148806,-1.05483163242336,
12.3942892069794));
#24689=CARTESIAN_POINT('Ctrl Pts',(-8.11359837641989,-1.35157521726427,
12.4420112304343));
#24690=CARTESIAN_POINT('Ctrl Pts',(-7.15526752559027,-0.406109994790781,
12.4897332538891));
#24691=CARTESIAN_POINT('Ctrl Pts',(-7.43006921799579,0.911761977902243,
12.537455277344));
#24692=CARTESIAN_POINT('Ctrl Pts',(-8.69013539730176,1.39291916460934,12.5851773007989));
#24693=CARTESIAN_POINT('Ctrl Pts',(-9.59116096550439,0.726603515571681,
12.6249456536779));
#24694=CARTESIAN_POINT('Ctrl Pts',(-9.73276546636217,-0.0781671504036021,
12.6567603359812));
#24695=CARTESIAN_POINT('Ctrl Pts',(-9.49064601300238,-0.858606661052731,
12.6885750182844));
#24696=CARTESIAN_POINT('Ctrl Pts',(-8.51267564008941,-1.40577899991123,
12.7283433711635));
#24697=CARTESIAN_POINT('Ctrl Pts',(-7.32347530531005,-0.76931880609604,
12.7760653946183));
#24698=CARTESIAN_POINT('Ctrl Pts',(-7.21733238908827,0.572708089273282,
12.8237874180732));
#24699=CARTESIAN_POINT('Ctrl Pts',(-8.28740794253882,1.3895561880445,12.871509441528));
#24700=CARTESIAN_POINT('Ctrl Pts',(-9.55514818289102,0.928998159624082,
12.9192314649829));
#24701=CARTESIAN_POINT('Ctrl Pts',(-9.80059547240428,-0.164427305040956,
12.958999817862));
#24702=CARTESIAN_POINT('Ctrl Pts',(-9.38113985803971,-0.865686634430231,
12.9908145001652));
#24703=CARTESIAN_POINT('Ctrl Pts',(-8.68741109134266,-1.29748294953088,
13.0226291824684));
#24704=CARTESIAN_POINT('Ctrl Pts',(-7.58981441832717,-1.07141844083344,
13.0623975353475));
#24705=CARTESIAN_POINT('Ctrl Pts',(-7.1069002094667,0.187975413936122,13.1101195588023));
#24706=CARTESIAN_POINT('Ctrl Pts',(-7.90468919460728,1.27233478321696,13.1578415822572));
#24707=CARTESIAN_POINT('Ctrl Pts',(-9.24838388325329,1.18995098466913,13.2055636057121));
#24708=CARTESIAN_POINT('Ctrl Pts',(-9.90578323664456,0.012196721373359,
13.253285629167));
#24709=CARTESIAN_POINT('Ctrl Pts',(-9.37599832386594,-0.975300906421013,
13.293053982046));
#24710=CARTESIAN_POINT('Ctrl Pts',(-8.59996442064334,-1.23118963326647,
13.3248686643492));
#24711=CARTESIAN_POINT('Ctrl Pts',(-7.7928145072655,-1.10384491680104,13.3566833466525));
#24712=CARTESIAN_POINT('Ctrl Pts',(-7.11066262301496,-0.214748507225108,
13.3964516995315));
#24713=CARTESIAN_POINT('Ctrl Pts',(-7.56945200982095,1.05363286803423,13.4441737229864));
#24714=CARTESIAN_POINT('Ctrl Pts',(-8.88225606424844,1.35170672001969,13.4918957464413));
#24715=CARTESIAN_POINT('Ctrl Pts',(-9.84452765095915,0.410252578827465,
13.5396177698961));
#24716=CARTESIAN_POINT('Ctrl Pts',(-9.57110829845308,-0.910550537547473,
13.587339793351));
#24717=CARTESIAN_POINT('Ctrl Pts',(-8.52435781001808,-1.31072179297237,
13.62710814623));
#24718=CARTESIAN_POINT('Ctrl Pts',(-7.77005699205511,-0.996495862314412,
13.6589228285333));
#24719=CARTESIAN_POINT('Ctrl Pts',(-7.24296615442084,-0.372089817853327,
13.6907375108365));
#24720=CARTESIAN_POINT('Ctrl Pts',(-7.30880357228206,0.746609897493391,
13.7305058637156));
#24721=CARTESIAN_POINT('Ctrl Pts',(-8.48563977554364,1.40565129622601,13.7782278871704));
#24722=CARTESIAN_POINT('Ctrl Pts',(-9.67347564116168,0.772130607605528,
13.8259499106253));
#24723=CARTESIAN_POINT('Ctrl Pts',(-9.78522311793835,-0.569441234672302,
13.8736719340801));
#24724=CARTESIAN_POINT('Ctrl Pts',(-8.71427517808187,-1.38941045645305,
13.921393957535));
#24725=CARTESIAN_POINT('Ctrl Pts',(-7.66084302554854,-1.00717451005825,
13.9611623104141));
#24726=CARTESIAN_POINT('Ctrl Pts',(-7.29599193222992,-0.276016976292999,
13.9929769927173));
#24727=CARTESIAN_POINT('Ctrl Pts',(-7.30591345323344,0.541056596219603,
14.0247916750205));
#24728=CARTESIAN_POINT('Ctrl Pts',(-8.08764486923065,1.34400093548008,14.0645600278996));
#24729=CARTESIAN_POINT('Ctrl Pts',(-9.40882805532143,1.07242405255057,14.1122820513545));
#24730=CARTESIAN_POINT('Ctrl Pts',(-9.8926336361544,-0.183854048235054,
14.1600040748093));
#24731=CARTESIAN_POINT('Ctrl Pts',(-9.09938085019241,-1.27153622797425,
14.2077260982642));
#24732=CARTESIAN_POINT('Ctrl Pts',(-7.75298433141432,-1.190942005024,14.2554481217191));
#24733=CARTESIAN_POINT('Ctrl Pts',(-7.20641169321538,-0.212636342217414,
14.2952164745981));
#24734=CARTESIAN_POINT('Ctrl Pts',(-7.40887280952849,0.579018352620409,
14.3270311569013));
#24735=CARTESIAN_POINT('Ctrl Pts',(-7.95097001357033,1.19044151283563,14.3588458392046));
#24736=CARTESIAN_POINT('Ctrl Pts',(-9.06750655394557,1.28620044303833,14.3986141920836));
#24737=CARTESIAN_POINT('Ctrl Pts',(-9.88896869373039,0.216397205310634,
14.4463362155385));
#24738=CARTESIAN_POINT('Ctrl Pts',(-9.43289198211277,-1.05021107655012,
14.4940582389934));
#24739=CARTESIAN_POINT('Ctrl Pts',(-8.1213443985153,-1.35376575451354,14.5417802624482));
#24740=CARTESIAN_POINT('Ctrl Pts',(-7.15585866218863,-0.411897235285569,
14.5895022859031));
#24741=CARTESIAN_POINT('Ctrl Pts',(-7.38259606962084,0.685560630316758,
14.6292706387821));
#24742=CARTESIAN_POINT('Ctrl Pts',(-8.0536709459124,1.15178607994221,14.6610853210854));
#24743=CARTESIAN_POINT('Ctrl Pts',(-8.86367504615505,1.25949409775321,14.6929000033886));
#24744=CARTESIAN_POINT('Ctrl Pts',(-9.77071256243562,0.601385776394011,
14.7326683562677));
#24745=CARTESIAN_POINT('Ctrl Pts',(-9.69199631825355,-0.745121842437787,
14.7803903797225));
#24746=CARTESIAN_POINT('Ctrl Pts',(-8.51837168210054,-1.40459717952675,
14.8281124031774));
#24747=CARTESIAN_POINT('Ctrl Pts',(-7.32790003807112,-0.776043466300811,
14.8758344266323));
#24748=CARTESIAN_POINT('Ctrl Pts',(-7.21399296821595,0.567944701423163,
14.9235564500871));
#24749=CARTESIAN_POINT('Ctrl Pts',(-8.10350744198034,1.2495513480657,14.9633248029662));
#24750=CARTESIAN_POINT('Ctrl Pts',(-8.91605153117148,1.1630657428884,14.9951394852694));
#24751=CARTESIAN_POINT('Ctrl Pts',(-9.5990909110902,0.714551673218286,15.0269541675726));
#24752=CARTESIAN_POINT('Ctrl Pts',(-9.85445463106407,-0.376600459844835,
15.0667225204517));
#24753=CARTESIAN_POINT('Ctrl Pts',(-8.91393366145371,-1.34339894468464,
15.1144445439066));
#24754=CARTESIAN_POINT('Ctrl Pts',(-7.5948952950249,-1.07425147771361,15.1621665673614));
#24755=CARTESIAN_POINT('Ctrl Pts',(-7.10584665164846,0.179994843176864,
15.2098885908163));
#24756=CARTESIAN_POINT('Ctrl Pts',(-7.89904710899984,1.27091739730048,15.2576106142712));
#24757=CARTESIAN_POINT('Ctrl Pts',(-9.0177063954227,1.20439403072938,15.2973789671502));
#24758=CARTESIAN_POINT('Ctrl Pts',(-9.57560963494508,0.607358648640619,
15.3291936494535));
#24759=CARTESIAN_POINT('Ctrl Pts',(-9.79870755565295,-0.178730113269691,
15.3610083317567));
#24760=CARTESIAN_POINT('Ctrl Pts',(-9.27790842578802,-1.17099611903574,
15.4007766846358));
#24761=CARTESIAN_POINT('Ctrl Pts',(-7.93408216140049,-1.28677857688729,
15.4484987080906));
#24762=CARTESIAN_POINT('Ctrl Pts',(-7.11264948841516,-0.220214228828185,
15.4962207315455));
#24763=CARTESIAN_POINT('Ctrl Pts',(-7.56343745957694,1.0482848064335,15.5439427550003));
#24764=CARTESIAN_POINT('Ctrl Pts',(-8.87705446008071,1.35433038087565,15.5916647784552));
#24765=CARTESIAN_POINT('Ctrl Pts',(-9.67953973170108,0.572095495672879,
15.6314331313343));
#24766=CARTESIAN_POINT('Ctrl Pts',(-9.71079808013641,-0.244422239744446,
15.6632478136375));
#24767=CARTESIAN_POINT('Ctrl Pts',(-9.36525453459661,-0.98490531805759,
15.6950624959407));
#24768=CARTESIAN_POINT('Ctrl Pts',(-8.32204860714223,-1.39448976690685,
15.7348308488198));
#24769=CARTESIAN_POINT('Ctrl Pts',(-7.23026016329708,-0.602944691238868,
15.7825528722746));
#24770=CARTESIAN_POINT('Ctrl Pts',(-7.3064571413049,0.741326568114441,15.8302748957295));
#24771=CARTESIAN_POINT('Ctrl Pts',(-8.47810477276462,1.40525997677245,15.8779969191844));
#24772=CARTESIAN_POINT('Ctrl Pts',(-9.67027309713215,0.778060702080256,
15.9257189426392));
#24773=CARTESIAN_POINT('Ctrl Pts',(-9.78737291614922,-0.563549955867611,
15.9734409660941));
#24774=CARTESIAN_POINT('Ctrl Pts',(-8.72189178072646,-1.387803675215,16.021162989549));
#24775=CARTESIAN_POINT('Ctrl Pts',(-7.45293723261821,-0.93689337562883,
16.0688850130038));
#24776=CARTESIAN_POINT('Ctrl Pts',(-7.14500260506151,0.373849720226483,
16.1166070364587));
#24777=CARTESIAN_POINT('Ctrl Pts',(-8.08314946719955,1.34257366335405,16.1643290599135));
#24778=CARTESIAN_POINT('Ctrl Pts',(-9.1815395506535,1.11991416460064,16.2040974127926));
#24779=CARTESIAN_POINT('Ctrl Pts',(-9.65014384072878,0.450492361508324,
16.2359120950958));
#24780=CARTESIAN_POINT('Ctrl Pts',(-9.76081674092163,-0.359093832643231,
16.2677267773991));
#24781=CARTESIAN_POINT('Ctrl Pts',(-9.1059854131481,-1.26852769992666,16.3074951302781));
#24782=CARTESIAN_POINT('Ctrl Pts',(-7.75921097797935,-1.19468910281155,
16.355217153733));
#24783=CARTESIAN_POINT('Ctrl Pts',(-7.09547696382248,-0.0234689032524444,
16.4029391771879));
#24784=CARTESIAN_POINT('Ctrl Pts',(-7.71971018800974,1.16927751850682,16.4506612006427));
#24785=CARTESIAN_POINT('Ctrl Pts',(-9.06327472143189,1.28805862362881,16.4983832240976));
#24786=CARTESIAN_POINT('Ctrl Pts',(-9.74810490751436,0.401023575788387,
16.5381515769766));
#24787=CARTESIAN_POINT('Ctrl Pts',(-9.66456742422846,-0.411829247736352,
16.5699662592799));
#24788=CARTESIAN_POINT('Ctrl Pts',(-9.21853458788756,-1.09649119427719,
16.6017809415831));
#24789=CARTESIAN_POINT('Ctrl Pts',(-8.12831596898121,-1.35581207733523,
16.6415492944622));
#24790=CARTESIAN_POINT('Ctrl Pts',(-7.15811168802375,-0.418804799962375,
16.6892713179171));
#24791=CARTESIAN_POINT('Ctrl Pts',(-7.42247182598189,0.901201308551626,
16.7369933413719));
#24792=CARTESIAN_POINT('Ctrl Pts',(-8.67493565199357,1.39479723197529,16.7847153648268));
#24793=CARTESIAN_POINT('Ctrl Pts',(-9.7687287250781,0.605559803923564,16.8324373882816));
#24794=CARTESIAN_POINT('Ctrl Pts',(-9.70626441131446,-0.513333317189079,
16.8722057411607));
#24795=CARTESIAN_POINT('Ctrl Pts',(-9.11125692448223,-1.07339916673304,
16.9040204234639));
#24796=CARTESIAN_POINT('Ctrl Pts',(-8.32598297924596,-1.2993471424164,16.9358351057672));
#24797=CARTESIAN_POINT('Ctrl Pts',(-7.33183350595512,-0.782152358472143,
16.9756034586462));
#24798=CARTESIAN_POINT('Ctrl Pts',(-7.21117732228494,0.561246726270426,
17.0233254821011));
#24799=CARTESIAN_POINT('Ctrl Pts',(-8.27475278233387,1.38654045969504,17.0710475055559));
#24800=CARTESIAN_POINT('Ctrl Pts',(-9.5448820960995,0.940363327686985,17.1187695290108));
#24801=CARTESIAN_POINT('Ctrl Pts',(-9.85568533561032,-0.37214585741601,
17.1664915524657));
#24802=CARTESIAN_POINT('Ctrl Pts',(-9.07637829172762,-1.17744341108019,
17.2062599053447));
#24803=CARTESIAN_POINT('Ctrl Pts',(-8.25996262410618,-1.21169420921509,
17.2380745876479));
#24804=CARTESIAN_POINT('Ctrl Pts',(-7.51826359447111,-0.86877992122654,
17.2698892699512));
#24805=CARTESIAN_POINT('Ctrl Pts',(-7.10482440400817,0.172801402766392,
17.3096576228303));
#24806=CARTESIAN_POINT('Ctrl Pts',(-7.89253547638418,1.26769421990383,17.3573796462851));
#24807=CARTESIAN_POINT('Ctrl Pts',(-9.23684024893197,1.19595033473499,17.40510166974));
#24808=CARTESIAN_POINT('Ctrl Pts',(-9.90545546432878,0.0275085517188402,
17.4528236931948));
#24809=CARTESIAN_POINT('Ctrl Pts',(-9.28175434417965,-1.16843288801686,
17.5005457166497));
#24810=CARTESIAN_POINT('Ctrl Pts',(-8.16551158461359,-1.26755766001141,
17.5403140695287));
#24811=CARTESIAN_POINT('Ctrl Pts',(-7.52568494958409,-0.759296372301703,
17.572128751832));
#24812=CARTESIAN_POINT('Ctrl Pts',(-7.18913418819074,-0.0146882575976357,
17.6039434341352));
#24813=CARTESIAN_POINT('Ctrl Pts',(-7.55795413929691,1.04351562747055,17.6437117870143));
#24814=CARTESIAN_POINT('Ctrl Pts',(-8.87002855169553,1.35614920033101,17.6914338104691));
#24815=CARTESIAN_POINT('Ctrl Pts',(-9.8397229875011,0.42234236392081,17.739155833924));
#24816=CARTESIAN_POINT('Ctrl Pts',(-9.58087862748931,-0.898756460485886,
17.7868778573788));
#24817=CARTESIAN_POINT('Ctrl Pts',(-8.3267233016254,-1.39511664538973,17.8345998808337));
#24818=CARTESIAN_POINT('Ctrl Pts',(-7.41770575864982,-0.739745967627945,
17.8743682337128));
#24819=CARTESIAN_POINT('Ctrl Pts',(-7.26637939162968,0.063253403556096,
17.906182916016));
#24820=CARTESIAN_POINT('Ctrl Pts',(-7.49904315960666,0.846563834067683,
17.9379975983193));
#24821=CARTESIAN_POINT('Ctrl Pts',(-8.47032497547387,1.40552291385181,17.9777659511983));
#24822=CARTESIAN_POINT('Ctrl Pts',(-9.66713516544579,0.783490451893412,
18.0254879746532));
#24823=CARTESIAN_POINT('Ctrl Pts',(-9.78949966687058,-0.557154704495792,
18.073209998108));
#24824=CARTESIAN_POINT('Ctrl Pts',(-8.72938063795075,-1.38688366691717,
18.1209320215629));
#24825=CARTESIAN_POINT('Ctrl Pts',(-7.45616349878414,-0.941690303216765,
18.1686540450177));
#24826=CARTESIAN_POINT('Ctrl Pts',(-7.1975111877415,0.148686971261949,18.2084223978968));
#24827=CARTESIAN_POINT('Ctrl Pts',(-7.60845568768243,0.854967565251188,
18.2402370802));
#24828=CARTESIAN_POINT('Ctrl Pts',(-8.29691194327969,1.29512167872335,18.2720517625033));
#24829=CARTESIAN_POINT('Ctrl Pts',(-9.39716218903309,1.08234711392068,18.3118201153823));
#24830=CARTESIAN_POINT('Ctrl Pts',(-9.89527113707947,-0.171114688619274,
18.3595421388372));
#24831=CARTESIAN_POINT('Ctrl Pts',(-9.11065382231136,-1.26504255457975,
18.4072641622921));
#24832=CARTESIAN_POINT('Ctrl Pts',(-7.76606111074645,-1.19891429613197,
18.4549861857469));
#24833=CARTESIAN_POINT('Ctrl Pts',(-7.0944670580837,-0.0291961920664319,
18.5027082092018));
#24834=CARTESIAN_POINT('Ctrl Pts',(-7.61227126287659,0.96463599910374,18.5424765620808));
#24835=CARTESIAN_POINT('Ctrl Pts',(-8.38515391517273,1.22989071679447,18.5742912443841));
#24836=CARTESIAN_POINT('Ctrl Pts',(-9.1937848058798,1.11231630600828,18.6061059266873));
#24837=CARTESIAN_POINT('Ctrl Pts',(-9.88663879356476,0.23153428390719,18.6458742795664));
#24838=CARTESIAN_POINT('Ctrl Pts',(-9.4432216954944,-1.04230255481647,18.6935963030212));
#24839=CARTESIAN_POINT('Ctrl Pts',(-8.13411829477636,-1.35623056055514,
18.7413183264762));
#24840=CARTESIAN_POINT('Ctrl Pts',(-7.1605319179062,-0.42648216806842,18.7890403499309));
#24841=CARTESIAN_POINT('Ctrl Pts',(-7.4179585923105,0.897530868822023,18.8367623733859));
#24842=CARTESIAN_POINT('Ctrl Pts',(-8.45979320188161,1.31033138360747,18.8765307262648));
#24843=CARTESIAN_POINT('Ctrl Pts',(-9.21783884631427,1.0052503117033,18.9083454085682));
#24844=CARTESIAN_POINT('Ctrl Pts',(-9.75244218309404,0.387264121095941,
18.9401600908714));
#24845=CARTESIAN_POINT('Ctrl Pts',(-9.70013819501298,-0.732149971873314,
18.9799284437504));
#24846=CARTESIAN_POINT('Ctrl Pts',(-8.53135794136673,-1.40537484755547,
19.0276504672053));
#24847=CARTESIAN_POINT('Ctrl Pts',(-7.33594766868813,-0.786265175095812,
19.0753724906601));
#24848=CARTESIAN_POINT('Ctrl Pts',(-7.20798451957174,0.553857184626204,
19.123094514115));
#24849=CARTESIAN_POINT('Ctrl Pts',(-8.26893812686215,1.3867175917342,19.1708165375699));
#24850=CARTESIAN_POINT('Ctrl Pts',(-9.32691568795275,1.01724892061836,19.2105848904489));
#24851=CARTESIAN_POINT('Ctrl Pts',(-9.70058210710294,0.290557055604711,
19.2423995727522));
#24852=CARTESIAN_POINT('Ctrl Pts',(-9.70054231361888,-0.526576750998593,
19.2742142550554));
#24853=CARTESIAN_POINT('Ctrl Pts',(-8.92857819660635,-1.33891597863224,
19.3139826079344));
#24854=CARTESIAN_POINT('Ctrl Pts',(-7.60420739907338,-1.08333623531821,
19.3617046313893));
#24855=CARTESIAN_POINT('Ctrl Pts',(-7.10524482354957,0.16699926157266,19.4094266548442));
#24856=CARTESIAN_POINT('Ctrl Pts',(-7.88528608756766,1.26419483802554,19.457148678299));
#24857=CARTESIAN_POINT('Ctrl Pts',(-9.23255879006808,1.19988869797871,19.5048707017539));
#24858=CARTESIAN_POINT('Ctrl Pts',(-9.79092226776038,0.228264364459435,
19.5446390546329));
#24859=CARTESIAN_POINT('Ctrl Pts',(-9.59804956384096,-0.565780835488472,
19.5764537369362));
#24860=CARTESIAN_POINT('Ctrl Pts',(-9.06338603915228,-1.18371495401972,
19.6082684192394));
#24861=CARTESIAN_POINT('Ctrl Pts',(-7.94808917357633,-1.29296933765633,
19.6480367721185));
#24862=CARTESIAN_POINT('Ctrl Pts',(-7.11374980070125,-0.233178402886113,
19.6957587955734));
#24863=CARTESIAN_POINT('Ctrl Pts',(-7.55447586424967,1.03885266727995,19.7434808190282));
#24864=CARTESIAN_POINT('Ctrl Pts',(-8.86225660550994,1.3582459035067,19.7912028424831));
#24865=CARTESIAN_POINT('Ctrl Pts',(-9.83906190809751,0.42812203251564,19.8389248659379));
#24866=CARTESIAN_POINT('Ctrl Pts',(-9.62561281515307,-0.671997553451521,
19.878693218817));
#24867=CARTESIAN_POINT('Ctrl Pts',(-8.96022515044173,-1.14630432667693,
19.9105079011202));
#24868=CARTESIAN_POINT('Ctrl Pts',(-8.15158281209082,-1.26379997810217,
19.9423225834235));
#24869=CARTESIAN_POINT('Ctrl Pts',(-7.23665301314377,-0.616708731286011,
19.9820909363026));
#24870=CARTESIAN_POINT('Ctrl Pts',(-7.29907996828855,0.730652352396478,
20.0298129597574));
#24871=CARTESIAN_POINT('Ctrl Pts',(-8.46464364182645,1.40427229679211,20.0775349832123));
#24872=CARTESIAN_POINT('Ctrl Pts',(-9.66262943404131,0.790161111248278,
20.1252570066671));
#24873=CARTESIAN_POINT('Ctrl Pts',(-9.79278123874688,-0.552351280606063,
20.172979030122));
#24874=CARTESIAN_POINT('Ctrl Pts',(-8.91157459044358,-1.24466512684449,
20.212747383001));
#24875=CARTESIAN_POINT('Ctrl Pts',(-8.09804403259428,-1.16801207130933,
20.2445620653043));
#24876=CARTESIAN_POINT('Ctrl Pts',(-7.40963065026857,-0.727790905856804,
20.2763767476075));
#24877=CARTESIAN_POINT('Ctrl Pts',(-7.141090118815,0.360193285974096,20.3161451004866));
#24878=CARTESIAN_POINT('Ctrl Pts',(-8.06985067592889,1.33829493820663,20.3638671239414));
#24879=CARTESIAN_POINT('Ctrl Pts',(-9.39204740920843,1.08511850750307,20.4115891473963));
#24880=CARTESIAN_POINT('Ctrl Pts',(-9.89622813459281,-0.163121975220366,
20.4593111708511));
#24881=CARTESIAN_POINT('Ctrl Pts',(-9.116278300971,-1.26355701264145,20.507033194306));
#24882=CARTESIAN_POINT('Ctrl Pts',(-7.99689648619272,-1.21056671682166,
20.5468015471851));
#24883=CARTESIAN_POINT('Ctrl Pts',(-7.43181377943531,-0.620321688040228,
20.5786162294883));
#24884=CARTESIAN_POINT('Ctrl Pts',(-7.19922630521013,0.163011399675998,
20.6104309117915));
#24885=CARTESIAN_POINT('Ctrl Pts',(-7.70798676693442,1.16150346839434,20.6501992646706));
#24886=CARTESIAN_POINT('Ctrl Pts',(-9.05031632239779,1.29352762936509,20.6979212881254));
#24887=CARTESIAN_POINT('Ctrl Pts',(-9.88458398875966,0.2369766521653,20.7456433115803));
#24888=CARTESIAN_POINT('Ctrl Pts',(-9.44917489199335,-1.0368841820752,20.7933653350352));
#24889=CARTESIAN_POINT('Ctrl Pts',(-8.13934378422536,-1.35878709239757,
20.84108735849));
#24890=CARTESIAN_POINT('Ctrl Pts',(-7.32747800377215,-0.586325071818895,
20.8808557113691));
#24891=CARTESIAN_POINT('Ctrl Pts',(-7.28631721489128,0.229771398542417,
20.9126703936723));
#24892=CARTESIAN_POINT('Ctrl Pts',(-7.62294049781938,0.974346730438525,
20.9444850759756));
#24893=CARTESIAN_POINT('Ctrl Pts',(-8.66098460634993,1.39658842360999,20.9842534288546));
#24894=CARTESIAN_POINT('Ctrl Pts',(-9.76250641639258,0.618174191628754,
21.0319754523095));
#24895=CARTESIAN_POINT('Ctrl Pts',(-9.70214506892388,-0.726689747322114,
21.0796974757644));
#24896=CARTESIAN_POINT('Ctrl Pts',(-8.5394051930937,-1.40517223619938,21.1274194992192));
#24897=CARTESIAN_POINT('Ctrl Pts',(-7.33822677752304,-0.791617488423931,
21.1751415226741));
#24898=CARTESIAN_POINT('Ctrl Pts',(-7.22965620770004,0.3237461518637,21.2149098755531));
#24899=CARTESIAN_POINT('Ctrl Pts',(-7.73248294792305,0.967852454265888,
21.2467245578564));
#24900=CARTESIAN_POINT('Ctrl Pts',(-8.47421537311915,1.31069450082703,21.2785392401596));
#24901=CARTESIAN_POINT('Ctrl Pts',(-9.53550351928153,0.950845797171466,
21.3183075930387));
#24902=CARTESIAN_POINT('Ctrl Pts',(-9.85923301680232,-0.358535059182232,
21.3660296164935));
#24903=CARTESIAN_POINT('Ctrl Pts',(-8.93366841152947,-1.33609972099487,
21.4137516399484));
#24904=CARTESIAN_POINT('Ctrl Pts',(-7.61042572425391,-1.08844815703786,
21.4614736634032));
#24905=CARTESIAN_POINT('Ctrl Pts',(-7.10346650134907,0.161460383961172,
21.5091956868581));
#24906=CARTESIAN_POINT('Ctrl Pts',(-7.75111857391915,1.07599327653694,21.5489640397371));
#24907=CARTESIAN_POINT('Ctrl Pts',(-8.55280814670003,1.23411186612053,21.5807787220404));
#24908=CARTESIAN_POINT('Ctrl Pts',(-9.33806008278557,1.00808740648967,21.6125934043437));
#24909=CARTESIAN_POINT('Ctrl Pts',(-9.9052213434253,0.0415721592550428,
21.6523617572227));
#24910=CARTESIAN_POINT('Ctrl Pts',(-9.29334254829634,-1.16046084970195,
21.7000837806776));
#24911=CARTESIAN_POINT('Ctrl Pts',(-7.95378128354117,-1.29416995382799,
21.7478058041324));
#24912=CARTESIAN_POINT('Ctrl Pts',(-7.11510780710624,-0.241112829791858,
21.7955278275873));
#24913=CARTESIAN_POINT('Ctrl Pts',(-7.5495070312765,1.03582739143655,21.8432498510421));
#24914=CARTESIAN_POINT('Ctrl Pts',(-8.63765566197109,1.30370082465606,21.8830182039212));
#24915=CARTESIAN_POINT('Ctrl Pts',(-9.34738972466389,0.898749939077283,
21.9148328862245));
#24916=CARTESIAN_POINT('Ctrl Pts',(-9.79335606771826,0.214044396277898,
21.9466475685277));
#24917=CARTESIAN_POINT('Ctrl Pts',(-9.58990309483685,-0.887967630214171,
21.9864159214067));
#24918=CARTESIAN_POINT('Ctrl Pts',(-8.34070285614741,-1.39666968270552,
22.0341379448616));
#24919=CARTESIAN_POINT('Ctrl Pts',(-7.24017215234422,-0.621340928856387,
22.0818599683165));
#24920=CARTESIAN_POINT('Ctrl Pts',(-7.29491563681422,0.723763400728039,
22.1295819917713));
#24921=CARTESIAN_POINT('Ctrl Pts',(-8.45890657115661,1.40523542459937,22.1773040152262));
#24922=CARTESIAN_POINT('Ctrl Pts',(-9.45708652899441,0.895862878737048,
22.2170723681053));
#24923=CARTESIAN_POINT('Ctrl Pts',(-9.72887443943722,0.125253385404268,
22.2488870504085));
#24924=CARTESIAN_POINT('Ctrl Pts',(-9.61814955891965,-0.684343835633367,
22.2807017327117));
#24925=CARTESIAN_POINT('Ctrl Pts',(-8.74326432564931,-1.38462909701821,
22.3204700855908));
#24926=CARTESIAN_POINT('Ctrl Pts',(-7.46571946372151,-0.95201132078553,
22.3681921090456));
#24927=CARTESIAN_POINT('Ctrl Pts',(-7.14072073026172,0.354387672557732,
22.4159141325005));
#24928=CARTESIAN_POINT('Ctrl Pts',(-8.06219409051336,1.33580977996379,22.4636361559554));
#24929=CARTESIAN_POINT('Ctrl Pts',(-9.38833888469312,1.08960052055111,22.5113581794102));
#24930=CARTESIAN_POINT('Ctrl Pts',(-9.80994406922133,0.0512977289309273,
22.5511265322893));
#24931=CARTESIAN_POINT('Ctrl Pts',(-9.51129102603857,-0.709303361835555,
22.5829412145925));
#24932=CARTESIAN_POINT('Ctrl Pts',(-8.89785256586858,-1.24911899245564,
22.6147558968957));
#24933=CARTESIAN_POINT('Ctrl Pts',(-7.7780358132456,-1.20629307445875,22.6545242497748));
#24934=CARTESIAN_POINT('Ctrl Pts',(-7.09494096399137,-0.0432537623660983,
22.7022462732296));
#24935=CARTESIAN_POINT('Ctrl Pts',(-7.70390892509399,1.15735463711693,22.7499682966846));
#24936=CARTESIAN_POINT('Ctrl Pts',(-9.04290001758308,1.29665776268707,22.7976903201394));
#24937=CARTESIAN_POINT('Ctrl Pts',(-9.88471189147151,0.24279259885862,22.8454123435943));
#24938=CARTESIAN_POINT('Ctrl Pts',(-9.52421257514643,-0.818274723056693,
22.8851806964733));
#24939=CARTESIAN_POINT('Ctrl Pts',(-8.80070995351091,-1.19807943072104,
22.9169953787766));
#24940=CARTESIAN_POINT('Ctrl Pts',(-7.98360508912736,-1.20495693595516,
22.9488100610798));
#24941=CARTESIAN_POINT('Ctrl Pts',(-7.16476004726262,-0.439897189189659,
22.9885784139589));
#24942=CARTESIAN_POINT('Ctrl Pts',(-7.40911941320573,0.8865897179551,23.0363004374137));
#24943=CARTESIAN_POINT('Ctrl Pts',(-8.65518623203828,1.39611890216659,23.0840224608686));
#24944=CARTESIAN_POINT('Ctrl Pts',(-9.75894579152361,0.625393697308581,
23.1317444843234));
#24945=CARTESIAN_POINT('Ctrl Pts',(-9.70604704714024,-0.722375102372304,
23.1794665077783));
#24946=CARTESIAN_POINT('Ctrl Pts',(-8.73918425256553,-1.28894368178221,
23.2192348606573));
#24947=CARTESIAN_POINT('Ctrl Pts',(-7.9435347756856,-1.10279973367158,23.2510495429606));
#24948=CARTESIAN_POINT('Ctrl Pts',(-7.32109670201655,-0.573386375392157,
23.2828642252638));
#24949=CARTESIAN_POINT('Ctrl Pts',(-7.20240489080355,0.540945654416883,
23.3226325781429));
#24950=CARTESIAN_POINT('Ctrl Pts',(-8.25509490385685,1.38422659868659,23.3703546015978));
#24951=CARTESIAN_POINT('Ctrl Pts',(-9.53081128146812,0.954284474147591,
23.4180766250526));
#24952=CARTESIAN_POINT('Ctrl Pts',(-9.86126385285633,-0.350745642218154,
23.4657986485075));
#24953=CARTESIAN_POINT('Ctrl Pts',(-8.93944227678327,-1.33538973854775,
23.5135206719623));
#24954=CARTESIAN_POINT('Ctrl Pts',(-7.83755519530068,-1.13126115561726,
23.5532890248414));
#24955=CARTESIAN_POINT('Ctrl Pts',(-7.35763269918339,-0.469912490238693,
23.5851037071446));
#24956=CARTESIAN_POINT('Ctrl Pts',(-7.23329584348133,0.337706235269606,
23.6169183894479));
#24957=CARTESIAN_POINT('Ctrl Pts',(-7.87261873264457,1.25808108395866,23.6566867423269));
#24958=CARTESIAN_POINT('Ctrl Pts',(-9.22046000244338,1.20706220531818,23.7044087657818));
#24959=CARTESIAN_POINT('Ctrl Pts',(-9.90392267688262,0.047242702461344,
23.7521307892367));
#24960=CARTESIAN_POINT('Ctrl Pts',(-9.29997482618396,-1.15589881049347,
23.7998528126915));
#24961=CARTESIAN_POINT('Ctrl Pts',(-7.95861231486585,-1.29741074561148,
23.8475748361464));
#24962=CARTESIAN_POINT('Ctrl Pts',(-7.25886358097769,-0.422096328884932,
23.8873431890254));
#24963=CARTESIAN_POINT('Ctrl Pts',(-7.32862709527643,0.392053971459042,
23.9191578713287));
#24964=CARTESIAN_POINT('Ctrl Pts',(-7.76300484896508,1.08416929897163,23.9509725536319));
#24965=CARTESIAN_POINT('Ctrl Pts',(-8.84867677583206,1.36191034008796,23.990740906511));
#24966=CARTESIAN_POINT('Ctrl Pts',(-9.83460563447141,0.441463003054064,
24.0384629299658));
#24967=CARTESIAN_POINT('Ctrl Pts',(-9.59263109087989,-0.882829572932237,
24.0861849534207));
#24968=CARTESIAN_POINT('Ctrl Pts',(-8.34870338444389,-1.39755898506989,
24.1339069768756));
#24969=CARTESIAN_POINT('Ctrl Pts',(-7.24170525405229,-0.626952630398398,
24.1816290003304));
#24970=CARTESIAN_POINT('Ctrl Pts',(-7.28521772844163,0.492837655003246,
24.2213973532095));
#24971=CARTESIAN_POINT('Ctrl Pts',(-7.87065800324083,1.06289672573235,24.2532120355127));
#24972=CARTESIAN_POINT('Ctrl Pts',(-8.65199409613447,1.30210702948024,24.2850267178159));
#24973=CARTESIAN_POINT('Ctrl Pts',(-9.65475720639185,0.801817349980151,
24.324795070695));
#24974=CARTESIAN_POINT('Ctrl Pts',(-9.79813988291764,-0.539346481407673,
24.3725170941499));
#24975=CARTESIAN_POINT('Ctrl Pts',(-8.74868910432396,-1.38252829446333,
24.4202391176047));
#24976=CARTESIAN_POINT('Ctrl Pts',(-7.47118803801445,-0.957918435726028,
24.4679611410596));
#24977=CARTESIAN_POINT('Ctrl Pts',(-7.13820852545198,0.349140728491224,
24.5156831645144));
#24978=CARTESIAN_POINT('Ctrl Pts',(-7.9037701658238,1.16751655505172,24.5554515173935));
#24979=CARTESIAN_POINT('Ctrl Pts',(-8.71948895511468,1.21558438499351,24.5872661996968));
#24980=CARTESIAN_POINT('Ctrl Pts',(-9.46688723084328,0.885276230514411,
24.619080882));
#24981=CARTESIAN_POINT('Ctrl Pts',(-9.89790116767083,-0.149156273309663,
24.658849234879));
#24982=CARTESIAN_POINT('Ctrl Pts',(-9.1288395594926,-1.25722813802644,24.7065712583339));
#24983=CARTESIAN_POINT('Ctrl Pts',(-7.78351283097435,-1.20825365392482,
24.7542932817887));
#24984=CARTESIAN_POINT('Ctrl Pts',(-7.09521169063023,-0.0512990105788772,
24.8020153052436));
#24985=CARTESIAN_POINT('Ctrl Pts',(-7.69857609692742,1.15503030091294,24.8497373286984));
#24986=CARTESIAN_POINT('Ctrl Pts',(-8.81298068775674,1.27303888808352,24.8895056815776));
#24987=CARTESIAN_POINT('Ctrl Pts',(-9.46132049901386,0.775682729363686,
24.9213203638807));
#24988=CARTESIAN_POINT('Ctrl Pts',(-9.8104292616916,0.0368791483632278,
24.9531350461841));
#24989=CARTESIAN_POINT('Ctrl Pts',(-9.45957759328401,-1.02741720391978,
24.992903399063));
#24990=CARTESIAN_POINT('Ctrl Pts',(-8.15298412698885,-1.36221942671018,
25.0406254225179));
#24991=CARTESIAN_POINT('Ctrl Pts',(-7.167619294276,-0.444963381207372,25.0883474459728));
#24992=CARTESIAN_POINT('Ctrl Pts',(-7.40406031475195,0.880328341544631,
25.1360694694276));
#24993=CARTESIAN_POINT('Ctrl Pts',(-8.64963249883034,1.39785027228844,25.1837914928825));
#24994=CARTESIAN_POINT('Ctrl Pts',(-9.56961520293805,0.757963217527989,
25.2235598457616));
#24995=CARTESIAN_POINT('Ctrl Pts',(-9.73451468385032,-0.0423591054596894,
25.2553745280648));
#24996=CARTESIAN_POINT('Ctrl Pts',(-9.51514573013107,-0.829496273697633,
25.2871892103681));
#24997=CARTESIAN_POINT('Ctrl Pts',(-8.55346631480298,-1.40481907077904,
25.3269575632471));
#24998=CARTESIAN_POINT('Ctrl Pts',(-7.34629662801778,-0.80313779148113,
25.374679586702));
#24999=CARTESIAN_POINT('Ctrl Pts',(-7.20125250317102,0.535243584811184,
25.4224016101568));
#25000=CARTESIAN_POINT('Ctrl Pts',(-8.24717225720877,1.38280147349625,25.4701236336117));
#25001=CARTESIAN_POINT('Ctrl Pts',(-9.52774405127491,0.959227519159094,
25.5178456570666));
#25002=CARTESIAN_POINT('Ctrl Pts',(-9.80481941008746,-0.126614487877935,
25.5576140099456));
#25003=CARTESIAN_POINT('Ctrl Pts',(-9.40589115882078,-0.839751157681684,
25.5894286922489));
#25004=CARTESIAN_POINT('Ctrl Pts',(-8.72498539679587,-1.29149777108218,
25.6212433745521));
#25005=CARTESIAN_POINT('Ctrl Pts',(-7.62129056292958,-1.09738097014961,
25.6610117274311));
#25006=CARTESIAN_POINT('Ctrl Pts',(-7.10203186105147,0.147468183392511,
25.708733750886));
#25007=CARTESIAN_POINT('Ctrl Pts',(-7.8680164916839,1.25452285782985,25.7564557743409));
#25008=CARTESIAN_POINT('Ctrl Pts',(-9.21353604522699,1.2111680704139,25.8041777977957));
#25009=CARTESIAN_POINT('Ctrl Pts',(-9.90483720405359,0.0529877207465818,
25.8518998212506));
#25010=CARTESIAN_POINT('Ctrl Pts',(-9.40393282022959,-0.94946847130034,
25.8916681741296));
#25011=CARTESIAN_POINT('Ctrl Pts',(-8.63565170996194,-1.22777009738866,
25.9234828564329));
#25012=CARTESIAN_POINT('Ctrl Pts',(-7.82514617666876,-1.12390268200446,
25.9552975387361));
#25013=CARTESIAN_POINT('Ctrl Pts',(-7.11747982604816,-0.254976934367291,
25.9950658916152));
#25014=CARTESIAN_POINT('Ctrl Pts',(-7.53926727780403,1.0261843982103,26.04278791507));
#25015=CARTESIAN_POINT('Ctrl Pts',(-8.84286824344772,1.36223056904334,26.0905099385249));
#25016=CARTESIAN_POINT('Ctrl Pts',(-9.83205574984714,0.44909827646907,26.1382319619798));
#25017=CARTESIAN_POINT('Ctrl Pts',(-9.59708154949269,-0.879083239634216,
26.1859539854346));
#25018=CARTESIAN_POINT('Ctrl Pts',(-8.56238498360011,-1.30946288046009,
26.2257223383137));
#25019=CARTESIAN_POINT('Ctrl Pts',(-7.79928295337053,-1.01725926833834,
26.2575370206169));
#25020=CARTESIAN_POINT('Ctrl Pts',(-7.25429371365722,-0.408412499377393,
26.2893517029202));
#25021=CARTESIAN_POINT('Ctrl Pts',(-7.28763849254092,0.711726663596802,
26.3291200557992));
#25022=CARTESIAN_POINT('Ctrl Pts',(-8.44485351632405,1.40464253387347,26.3768420792541));
#25023=CARTESIAN_POINT('Ctrl Pts',(-9.65057400354622,0.805859924530725,
26.4245641027089));
#25024=CARTESIAN_POINT('Ctrl Pts',(-9.8012071227059,-0.531903944756735,
26.4722861261638));
#25025=CARTESIAN_POINT('Ctrl Pts',(-8.7545059253607,-1.38260695875558,26.5200081496186));
#25026=CARTESIAN_POINT('Ctrl Pts',(-7.69042488176934,-1.03110283164356,
26.5597765024977));
#25027=CARTESIAN_POINT('Ctrl Pts',(-7.30450910349292,-0.310841301673525,
26.591591184801));
#25028=CARTESIAN_POINT('Ctrl Pts',(-7.29071479240244,0.506176064395959,
26.6234058671042));
#25029=CARTESIAN_POINT('Ctrl Pts',(-8.04881534252997,1.33146823969133,26.6631742199833));
#25030=CARTESIAN_POINT('Ctrl Pts',(-9.3773232994039,1.09834676261705,26.7108962434381));
#25031=CARTESIAN_POINT('Ctrl Pts',(-9.89738257797027,-0.143362081410278,
26.758618266893));
#25032=CARTESIAN_POINT('Ctrl Pts',(-9.13602866466635,-1.25360652533043,
26.8063402903478));
#25033=CARTESIAN_POINT('Ctrl Pts',(-7.78786035280959,-1.21211896748734,
26.8540623138027));
#25034=CARTESIAN_POINT('Ctrl Pts',(-7.21312727362265,-0.250087000037398,
26.8938306666818));
#25035=CARTESIAN_POINT('Ctrl Pts',(-7.39252912631154,0.54710973523519,26.925645348985));
#25036=CARTESIAN_POINT('Ctrl Pts',(-7.91665437889142,1.17400715833212,26.9574600312882));
#25037=CARTESIAN_POINT('Ctrl Pts',(-9.02994171668213,1.30212789132369,26.9972283841673));
#25038=CARTESIAN_POINT('Ctrl Pts',(-9.88210380039875,0.256614238793779,
27.0449504076221));
#25039=CARTESIAN_POINT('Ctrl Pts',(-9.46297642576351,-1.02269602474285,
27.092672431077));
#25040=CARTESIAN_POINT('Ctrl Pts',(-8.16079045651933,-1.36418425010698,
27.1403944545319));
#25041=CARTESIAN_POINT('Ctrl Pts',(-7.16837812888729,-0.450731029348263,
27.1881164779867));
#25042=CARTESIAN_POINT('Ctrl Pts',(-7.36317157335998,0.652844583239182,
27.2278848308658));
#25043=CARTESIAN_POINT('Ctrl Pts',(-8.02043384525043,1.13834840961636,27.259699513169));
#25044=CARTESIAN_POINT('Ctrl Pts',(-8.82697108162581,1.26951755925708,27.2915141954723));
#25045=CARTESIAN_POINT('Ctrl Pts',(-9.75272502333722,0.638008843471489,
27.3312825483513));
#25046=CARTESIAN_POINT('Ctrl Pts',(-9.71311787736138,-0.710216022245723,
27.3790045718062));
#25047=CARTESIAN_POINT('Ctrl Pts',(-8.55912566120076,-1.40347244781957,
27.4267265952611));
#25048=CARTESIAN_POINT('Ctrl Pts',(-7.35091464810136,-0.809731212613409,
27.4744486187159));
#25049=CARTESIAN_POINT('Ctrl Pts',(-7.19805272372483,0.530385292257197,
27.5221706421708));
#25050=CARTESIAN_POINT('Ctrl Pts',(-8.06741218131559,1.23751876777988,27.5619389950498));
#25051=CARTESIAN_POINT('Ctrl Pts',(-8.88212387979244,1.17464979417261,27.593753677353));
#25052=CARTESIAN_POINT('Ctrl Pts',(-9.57789155350878,0.74614658101211,27.6255683596563));
#25053=CARTESIAN_POINT('Ctrl Pts',(-9.86481320056272,-0.337135278505183,
27.6653367125353));
#25054=CARTESIAN_POINT('Ctrl Pts',(-8.95274504552348,-1.33082068904202,
27.7130587359902));
#25055=CARTESIAN_POINT('Ctrl Pts',(-7.62645152946083,-1.10006537315734,
27.7607807594451));
#25056=CARTESIAN_POINT('Ctrl Pts',(-7.10121031756601,0.139460413539338,
27.8085027829));
#25057=CARTESIAN_POINT('Ctrl Pts',(-7.86241796941027,1.25294230621852,27.8562248063548));
#25058=CARTESIAN_POINT('Ctrl Pts',(-8.98253647802948,1.21891077148923,27.8959931592339));
#25059=CARTESIAN_POINT('Ctrl Pts',(-9.55753106065096,0.638317205013169,
27.927807841537));
#25060=CARTESIAN_POINT('Ctrl Pts',(-9.80334705142044,-0.140965900257004,
27.9596225238404));
#25061=CARTESIAN_POINT('Ctrl Pts',(-9.3115640063478,-1.14792819115299,27.9993908767193));
#25062=CARTESIAN_POINT('Ctrl Pts',(-7.97166201070898,-1.30265910801723,
28.0471129001743));
#25063=CARTESIAN_POINT('Ctrl Pts',(-7.11962647580337,-0.260383734703235,
28.0948349236291));
#25064=CARTESIAN_POINT('Ctrl Pts',(-7.53340666774274,1.02066601425938,28.142556947084));
#25065=CARTESIAN_POINT('Ctrl Pts',(-8.83760022077483,1.36469826678866,28.1902789705388));
#25066=CARTESIAN_POINT('Ctrl Pts',(-9.66242744626732,0.606091868981755,
28.2300473234179));
#25067=CARTESIAN_POINT('Ctrl Pts',(-9.71739887259082,-0.209190782474407,
28.2618620057211));
#25068=CARTESIAN_POINT('Ctrl Pts',(-9.3934295173966,-0.959358441316799,
28.2936766880244));
#25069=CARTESIAN_POINT('Ctrl Pts',(-8.36268274870058,-1.39911373409659,
28.3334450409034));
#25070=CARTESIAN_POINT('Ctrl Pts',(-7.24814023693788,-0.639459862898064,
28.3811670643583));
#25071=CARTESIAN_POINT('Ctrl Pts',(-7.28572434802244,0.706233245190266,
28.4288890878131));
#25072=CARTESIAN_POINT('Ctrl Pts',(-8.43681084816737,1.40430371135129,28.4766111112681));
#25073=CARTESIAN_POINT('Ctrl Pts',(-9.64820460654916,0.811172885373071,
28.5243331347228));
#25074=CARTESIAN_POINT('Ctrl Pts',(-9.77564275421098,-0.302192794555114,
28.564101487602));
#25075=CARTESIAN_POINT('Ctrl Pts',(-9.28379281900323,-0.954719652751162,
28.5959161699052));
#25076=CARTESIAN_POINT('Ctrl Pts',(-8.54797102693755,-1.31007011342867,
28.6277308522084));
#25077=CARTESIAN_POINT('Ctrl Pts',(-7.48074273921507,-0.968240623257071,
28.6674992050875));
#25078=CARTESIAN_POINT('Ctrl Pts',(-7.13489178381066,0.335471818616655,
28.7152212285423));
#25079=CARTESIAN_POINT('Ctrl Pts',(-8.04377353674895,1.32856620832038,28.7629432519972));
#25080=CARTESIAN_POINT('Ctrl Pts',(-9.37101931995447,1.10335267503478,28.810665275452));
#25081=CARTESIAN_POINT('Ctrl Pts',(-9.89906687296496,-0.137793890164783,
28.8583872989069));
#25082=CARTESIAN_POINT('Ctrl Pts',(-9.26699068934855,-1.06316047838938,
28.8981556517859));
#25083=CARTESIAN_POINT('Ctrl Pts',(-8.46809297375091,-1.23482903167168,
28.9299703340892));
#25084=CARTESIAN_POINT('Ctrl Pts',(-7.67912697365966,-1.02213130798338,
28.9617850163925));
#25085=CARTESIAN_POINT('Ctrl Pts',(-7.09568388763803,-0.0653566335221624,
29.0015533692715));
#25086=CARTESIAN_POINT('Ctrl Pts',(-7.68712449973501,1.14686320768974,29.0492753927264));
#25087=CARTESIAN_POINT('Ctrl Pts',(-9.02423013404472,1.30323198402877,29.0969974161812));
#25088=CARTESIAN_POINT('Ctrl Pts',(-9.88061158665234,0.264524506767463,
29.1447194396361));
#25089=CARTESIAN_POINT('Ctrl Pts',(-9.4678934712441,-1.0195869991764,29.1924414630909));
#25090=CARTESIAN_POINT('Ctrl Pts',(-8.38443551051107,-1.30584459467476,
29.23220981597));
#25091=CARTESIAN_POINT('Ctrl Pts',(-7.6679479210642,-0.912967317898404,
29.2640244982733));
#25092=CARTESIAN_POINT('Ctrl Pts',(-7.21045226783838,-0.235910619659525,
29.2958391805765));
#25093=CARTESIAN_POINT('Ctrl Pts',(-7.39522151652002,0.869389006667542,
29.3356075334556));
#25094=CARTESIAN_POINT('Ctrl Pts',(-8.63562576788721,1.39916518175529,29.3833295569103));
#25095=CARTESIAN_POINT('Ctrl Pts',(-9.74913324417835,0.642583048872662,
29.4310515803653));
#25096=CARTESIAN_POINT('Ctrl Pts',(-9.71715498903128,-0.703261816482831,
29.4787736038201));
#25097=CARTESIAN_POINT('Ctrl Pts',(-8.56489804327719,-1.40432985445164,
29.526495627275));
#25098=CARTESIAN_POINT('Ctrl Pts',(-7.55818298447205,-0.911952754888512,
29.566263980154));
#25099=CARTESIAN_POINT('Ctrl Pts',(-7.27346847986514,-0.14602059297262,
29.5980786624573));
#25100=CARTESIAN_POINT('Ctrl Pts',(-7.37031213472133,0.66526743560203,29.6298933447605));
#25101=CARTESIAN_POINT('Ctrl Pts',(-8.23356786559638,1.38041415523581,29.6696616976396));
#25102=CARTESIAN_POINT('Ctrl Pts',(-9.51761336754789,0.969214049802536,
29.7173837210944));
#25103=CARTESIAN_POINT('Ctrl Pts',(-9.86581870095987,-0.33101037424556,
29.7651057445493));
#25104=CARTESIAN_POINT('Ctrl Pts',(-8.95896334044735,-1.32880668070373,
29.8128277680042));
#25105=CARTESIAN_POINT('Ctrl Pts',(-7.85403417684868,-1.14084454386819,
29.8525961208832));
#25106=CARTESIAN_POINT('Ctrl Pts',(-7.36447187803796,-0.486329821775057,
29.8844108031865));
#25107=CARTESIAN_POINT('Ctrl Pts',(-7.22885571001066,0.319024610172502,
29.9162254854897));
#25108=CARTESIAN_POINT('Ctrl Pts',(-7.85366944090153,1.24940928029703,29.9559938383688));
#25109=CARTESIAN_POINT('Ctrl Pts',(-9.20420356711764,1.21639724974061,30.0037158618236));
#25110=CARTESIAN_POINT('Ctrl Pts',(-9.78431034371099,0.260901981677749,
30.0434842147027));
#25111=CARTESIAN_POINT('Ctrl Pts',(-9.61211124696142,-0.541081198726826,
30.0752988970059));
#25112=CARTESIAN_POINT('Ctrl Pts',(-9.3510349247924,-0.852523833800324,
30.0912062381575));
#25113=CARTESIAN_POINT('Ctrl Pts',(-9.18987679192715,-0.967444397671153,
30.0991599087333));
#25114=CARTESIAN_POINT('',(-9.01183881116714,1.07233375495133,30.));
#25115=CARTESIAN_POINT('Ctrl Pts',(-9.01356946732976,1.07334645743585,30.));
#25116=CARTESIAN_POINT('Ctrl Pts',(-9.0404013004879,1.05836761542857,30.));
#25117=CARTESIAN_POINT('Ctrl Pts',(-9.06653941803383,1.04232411727425,30.));
#25118=CARTESIAN_POINT('Ctrl Pts',(-9.09191232737533,1.02521683657113,30.));
#25119=CARTESIAN_POINT('Ctrl Pts',(-9.13297340585366,0.9975320572639,30.));
#25120=CARTESIAN_POINT('Ctrl Pts',(-9.17203266553443,0.967063261291628,
30.));
#25121=CARTESIAN_POINT('Ctrl Pts',(-9.20897145121856,0.9341121128447,30.));
#25122=CARTESIAN_POINT('Ctrl Pts',(-9.23971661511987,0.906685968726147,
30.));
#25123=CARTESIAN_POINT('Ctrl Pts',(-9.2689923033626,0.877538967782025,30.));
#25124=CARTESIAN_POINT('Ctrl Pts',(-9.29670822146099,0.846828311807377,
30.));
#25125=CARTESIAN_POINT('Ctrl Pts',(-9.30970173078921,0.832430838360316,
30.));
#25126=CARTESIAN_POINT('Ctrl Pts',(-9.32235212446905,0.817689530036482,
30.));
#25127=CARTESIAN_POINT('Ctrl Pts',(-9.33464839610017,0.802619887632117,
30.));
#25128=CARTESIAN_POINT('Ctrl Pts',(-9.34095951606682,0.794885321909954,
30.));
#25129=CARTESIAN_POINT('Ctrl Pts',(-9.34717733114601,0.78706425754689,30.));
#25130=CARTESIAN_POINT('Ctrl Pts',(-9.35330023379542,0.779158763052844,
30.));
#25131=CARTESIAN_POINT('Ctrl Pts',(-9.35900505310472,0.77179307063187,30.));
#25132=CARTESIAN_POINT('Ctrl Pts',(-9.36462187785631,0.764361279806068,
30.));
#25133=CARTESIAN_POINT('Ctrl Pts',(-9.37014824198907,0.756867742145807,
30.));
#25134=CARTESIAN_POINT('Ctrl Pts',(-9.39935024489035,0.717270946994591,
30.));
#25135=CARTESIAN_POINT('Ctrl Pts',(-9.42604623385499,0.675931375532437,
30.));
#25136=CARTESIAN_POINT('Ctrl Pts',(-9.45011051308741,0.633132080589728,
30.));
#25137=CARTESIAN_POINT('Ctrl Pts',(-9.47490181921347,0.589039738880434,
30.));
#25138=CARTESIAN_POINT('Ctrl Pts',(-9.49690076359938,0.543396988540731,
30.));
#25139=CARTESIAN_POINT('Ctrl Pts',(-9.51591602634924,0.496493124727175,
30.));
#25140=CARTESIAN_POINT('Ctrl Pts',(-9.52463388565747,0.474989278521212,
30.));
#25141=CARTESIAN_POINT('Ctrl Pts',(-9.53272379643383,0.453220191416638,
30.));
#25142=CARTESIAN_POINT('Ctrl Pts',(-9.5401630139613,0.431213428814737,30.));
#25143=CARTESIAN_POINT('Ctrl Pts',(-9.5449227151396,0.41713323644234,30.));
#25144=CARTESIAN_POINT('Ctrl Pts',(-9.54941599265901,0.402955749296612,
30.));
#25145=CARTESIAN_POINT('Ctrl Pts',(-9.55363626349372,0.388688248405426,
30.));
#25146=CARTESIAN_POINT('Ctrl Pts',(-9.55641171336528,0.379305264453263,
30.));
#25147=CARTESIAN_POINT('Ctrl Pts',(-9.55906701928206,0.369890069837169,
30.));
#25148=CARTESIAN_POINT('Ctrl Pts',(-9.56159885895017,0.360452578677009,
30.));
#25149=CARTESIAN_POINT('Ctrl Pts',(-9.57396435642608,0.314359899669795,
30.));
#25150=CARTESIAN_POINT('Ctrl Pts',(-9.58340587491649,0.267678796348387,
30.));
#25151=CARTESIAN_POINT('Ctrl Pts',(-9.58977429414167,0.220657430411709,
30.));
#25152=CARTESIAN_POINT('Ctrl Pts',(-9.59595307893544,0.175036234545199,
30.));
#25153=CARTESIAN_POINT('Ctrl Pts',(-9.59923915769065,0.129093821702756,
30.));
#25154=CARTESIAN_POINT('Ctrl Pts',(-9.59944739469354,0.0830577788125183,
30.));
#25155=CARTESIAN_POINT('Ctrl Pts',(-9.59949272984566,0.0730352997219751,
30.));
#25156=CARTESIAN_POINT('Ctrl Pts',(-9.59939199084664,0.0630084152088303,
30.));
#25157=CARTESIAN_POINT('Ctrl Pts',(-9.59914293971342,0.0529795432812796,
30.));
#25158=CARTESIAN_POINT('Ctrl Pts',(-9.59854500970755,0.0289019035901314,
30.));
#25159=CARTESIAN_POINT('Ctrl Pts',(-9.59709240210605,0.0048126867034857,
30.));
#25160=CARTESIAN_POINT('Ctrl Pts',(-9.59479829199329,-0.0192454360586858,
30.));
#25161=CARTESIAN_POINT('Ctrl Pts',(-9.59353734581922,-0.0324688631660106,
30.));
#25162=CARTESIAN_POINT('Ctrl Pts',(-9.5920210560175,-0.0456892788046415,
30.));
#25163=CARTESIAN_POINT('Ctrl Pts',(-9.59025657526382,-0.0588641198083392,
30.));
#25164=CARTESIAN_POINT('Ctrl Pts',(-9.58407424635836,-0.105025688979562,
30.));
#25165=CARTESIAN_POINT('Ctrl Pts',(-9.57484586966463,-0.150694655922387,
30.));
#25166=CARTESIAN_POINT('Ctrl Pts',(-9.56272960679499,-0.195579451729583,
30.));
#25167=CARTESIAN_POINT('Ctrl Pts',(-9.55017158310486,-0.24210075414254,
30.));
#25168=CARTESIAN_POINT('Ctrl Pts',(-9.53451086275111,-0.287781072722504,
30.));
#25169=CARTESIAN_POINT('Ctrl Pts',(-9.51587014765823,-0.332272113111234,
30.));
#25170=CARTESIAN_POINT('Ctrl Pts',(-9.50654979011179,-0.354517633305599,
30.));
#25171=CARTESIAN_POINT('Ctrl Pts',(-9.49648365210744,-0.376465335235619,
30.));
#25172=CARTESIAN_POINT('Ctrl Pts',(-9.48568282591157,-0.398067850774574,
30.));
#25173=CARTESIAN_POINT('Ctrl Pts',(-9.48055176124769,-0.408330390150984,
30.));
#25174=CARTESIAN_POINT('Ctrl Pts',(-9.47525485138614,-0.418514982656314,
30.));
#25175=CARTESIAN_POINT('Ctrl Pts',(-9.46979309127951,-0.428616291644545,
30.));
#25176=CARTESIAN_POINT('Ctrl Pts',(-9.46522229892417,-0.437069791066159,
30.));
#25177=CARTESIAN_POINT('Ctrl Pts',(-9.46053625618582,-0.44546432784445,
30.));
#25178=CARTESIAN_POINT('Ctrl Pts',(-9.45574246837851,-0.453785377323363,
30.));
#25179=CARTESIAN_POINT('Ctrl Pts',(-9.45420664198032,-0.456451262415496,
30.));
#25180=CARTESIAN_POINT('Ctrl Pts',(-9.45265958743055,-0.459109921130538,
30.));
#25181=CARTESIAN_POINT('Ctrl Pts',(-9.45110134197801,-0.461761264311804,
30.));
#25182=CARTESIAN_POINT('Ctrl Pts',(-9.42910351919434,-0.499190398049958,
30.));
#25183=CARTESIAN_POINT('Ctrl Pts',(-9.40487798623216,-0.53516396160983,
30.));
#25184=CARTESIAN_POINT('Ctrl Pts',(-9.37856312896001,-0.56950997033306,
30.));
#25185=CARTESIAN_POINT('Ctrl Pts',(-9.35643733060892,-0.598388442114831,
30.));
#25186=CARTESIAN_POINT('Ctrl Pts',(-9.332833692907,-0.626116038782497,30.));
#25187=CARTESIAN_POINT('Ctrl Pts',(-9.30782041440045,-0.652572448466639,
30.));
#25188=CARTESIAN_POINT('Ctrl Pts',(-9.30064609642426,-0.660160685871532,
30.));
#25189=CARTESIAN_POINT('Ctrl Pts',(-9.2933564227585,-0.667643328887313,
30.));
#25190=CARTESIAN_POINT('Ctrl Pts',(-9.28596221946619,-0.675008596291465,
30.));
#25191=CARTESIAN_POINT('Ctrl Pts',(-9.25445294625133,-0.706394563617926,
30.));
#25192=CARTESIAN_POINT('Ctrl Pts',(-9.22100504610438,-0.735698182988929,
30.));
#25193=CARTESIAN_POINT('Ctrl Pts',(-9.185756453621,-0.762712472111516,30.));
#25194=CARTESIAN_POINT('Ctrl Pts',(-9.15521777370757,-0.786117115261243,
30.));
#25195=CARTESIAN_POINT('Ctrl Pts',(-9.12332669441508,-0.807803020376991,
30.));
#25196=CARTESIAN_POINT('Ctrl Pts',(-9.09015970213924,-0.82760676144889,
30.));
#25197=CARTESIAN_POINT('Ctrl Pts',(-9.68829027239597,-0.000978575593966811,
29.7537368763048));
#25198=CARTESIAN_POINT('Ctrl Pts',(-9.68913288765981,-0.0952583801369799,
29.757526499053));
#25199=CARTESIAN_POINT('Ctrl Pts',(-9.67882321668234,-0.189362368800223,
29.7613161218011));
#25200=CARTESIAN_POINT('Ctrl Pts',(-9.65664191863911,-0.280605687980609,
29.7651057445493));
#25201=CARTESIAN_POINT('Ctrl Pts',(-9.56353358078901,-0.663609143064989,
29.7810130857009));
#25202=CARTESIAN_POINT('Ctrl Pts',(-9.26124846061824,-0.996207911884316,
29.7969204268525));
#25203=CARTESIAN_POINT('Ctrl Pts',(-8.88912006781309,-1.12491486892692,
29.8128277680042));
#25204=CARTESIAN_POINT('Ctrl Pts',(-8.51699167500794,-1.25362182596952,
29.8287351091558));
#25205=CARTESIAN_POINT('Ctrl Pts',(-8.07502000956843,-1.1784369712353,29.8446424503074));
#25206=CARTESIAN_POINT('Ctrl Pts',(-7.76450868815171,-0.935203778959528,
29.860549791459));
#25207=CARTESIAN_POINT('Ctrl Pts',(-7.60925302744333,-0.81358718282163,
29.8685034620348));
#25208=CARTESIAN_POINT('Ctrl Pts',(-7.48686245274063,-0.649958502298315,
29.8764571326107));
#25209=CARTESIAN_POINT('Ctrl Pts',(-7.40871514438587,-0.467474858043207,
29.8844108031865));
#25210=CARTESIAN_POINT('Ctrl Pts',(-7.33056783603113,-0.284991213788141,
29.8923644737623));
#25211=CARTESIAN_POINT('Ctrl Pts',(-7.29666379402431,-0.0836526058012479,
29.9003181443381));
#25212=CARTESIAN_POINT('Ctrl Pts',(-7.31571534807915,0.11259877753163,29.9082718149139));
#25213=CARTESIAN_POINT('Ctrl Pts',(-7.35381845618883,0.505101544197385,
29.9241791560655));
#25214=CARTESIAN_POINT('Ctrl Pts',(-7.60374394854509,0.877255412247096,
29.9400864972171));
#25215=CARTESIAN_POINT('Ctrl Pts',(-7.95379571575922,1.0578303411793,29.9559938383687));
#25216=CARTESIAN_POINT('Ctrl Pts',(-8.2765908013847,1.2243448544765,29.9706625589125));
#25217=CARTESIAN_POINT('Ctrl Pts',(-8.68452661087086,1.22795338154701,29.9853312794563));
#25218=CARTESIAN_POINT('Ctrl Pts',(-9.01356946732952,1.07334645743597,30.));
#25219=CARTESIAN_POINT('Ctrl Pts',(-9.09176790333495,-0.828203493281094,
1.8));
#25220=CARTESIAN_POINT('Ctrl Pts',(-8.83745586871391,-1.007228726393,1.81466872054375));
#25221=CARTESIAN_POINT('Ctrl Pts',(-8.11993078322208,-1.12691245974044,
1.84524478223913));
#25222=CARTESIAN_POINT('Ctrl Pts',(-7.47631525146516,-0.457174338716646,
1.88377451451031));
#25223=CARTESIAN_POINT('Ctrl Pts',(-7.47121748055022,0.241452561832278,
1.91558919681355));
#25224=CARTESIAN_POINT('Ctrl Pts',(-7.78668186971636,0.865450294731047,
1.94740387911679));
#25225=CARTESIAN_POINT('Ctrl Pts',(-8.6897509574811,1.18756791113319,1.98717223199585));
#25226=CARTESIAN_POINT('Ctrl Pts',(-9.42307202460602,0.619626775593939,
2.02554781833935));
#25227=CARTESIAN_POINT('Ctrl Pts',(-9.51573132444702,0.140538355580566,
2.04801606353124));
#25228=CARTESIAN_POINT('Ctrl Pts',(-9.51515984464673,0.000434573109195022,
2.05457696757151));
#25229=CARTESIAN_POINT('Origin',(-8.5,0.,1.24542303242842));
#25230=CARTESIAN_POINT('Ctrl Pts',(-7.9098402978609,-0.827606761448989,
1.8));
#25231=CARTESIAN_POINT('Ctrl Pts',(-7.69350384516205,-0.673338983038085,
1.81248093324819));
#25232=CARTESIAN_POINT('Ctrl Pts',(-7.54189267616637,-0.43110531180156,
1.82496186649638));
#25233=CARTESIAN_POINT('Ctrl Pts',(-7.49768958341452,-0.169101314096706,
1.83744279974457));
#25234=CARTESIAN_POINT('Ctrl Pts',(-7.45348649066266,0.0929026836081468,
1.84992373299276));
#25235=CARTESIAN_POINT('Ctrl Pts',(-7.51723259935484,0.371469608550013,
1.86240466624095));
#25236=CARTESIAN_POINT('Ctrl Pts',(-7.67098159359225,0.588175065318269,
1.87488559948914));
#25237=CARTESIAN_POINT('Ctrl Pts',(-7.82473058782966,0.804880522086524,
1.88736653273733));
#25238=CARTESIAN_POINT('Ctrl Pts',(-8.06660030394209,0.957071646902186,
1.89984746598552));
#25239=CARTESIAN_POINT('Ctrl Pts',(-8.32849763913847,1.00190237340967,1.91232839923372));
#25240=CARTESIAN_POINT('Ctrl Pts',(-8.59039497433485,1.04673309991714,1.92480933248191));
#25241=CARTESIAN_POINT('Ctrl Pts',(-8.86911383512443,0.983654619552456,
1.9372902657301));
#25242=CARTESIAN_POINT('Ctrl Pts',(-9.0861870518979,0.830425292131839,1.94977119897829));
#25243=CARTESIAN_POINT('Ctrl Pts',(-9.30326026867136,0.677195964711223,
1.96225213222648));
#25244=CARTESIAN_POINT('Ctrl Pts',(-9.45603047560713,0.435691592250255,
1.97473306547467));
#25245=CARTESIAN_POINT('Ctrl Pts',(-9.50148857850568,0.173902423064403,
1.98721399872286));
#25246=CARTESIAN_POINT('Ctrl Pts',(-9.51145490317781,0.11650724620064,1.9899503432914));
#25247=CARTESIAN_POINT('Ctrl Pts',(-9.51647499999999,0.0582540466810683,
1.99268668785994));
#25248=CARTESIAN_POINT('Ctrl Pts',(-9.516475,2.33298725921038E-13,1.99542303242848));
#25249=CARTESIAN_POINT('Ctrl Pts',(-7.81012320807277,-0.967444397671095,
1.70084009126668));
#25250=CARTESIAN_POINT('Ctrl Pts',(-7.64896507520752,-0.852523833800245,
1.70879376184249));
#25251=CARTESIAN_POINT('Ctrl Pts',(-7.38788875303855,-0.541081198726736,
1.72470110299411));
#25252=CARTESIAN_POINT('Ctrl Pts',(-7.21568965628902,0.260901981677851,
1.75651578529735));
#25253=CARTESIAN_POINT('Ctrl Pts',(-7.79579643288244,1.21639724974065,1.79628413817641));
#25254=CARTESIAN_POINT('Ctrl Pts',(-9.14633055909857,1.24940928029698,1.84400616163127));
#25255=CARTESIAN_POINT('Ctrl Pts',(-9.77114428998937,0.319024610172379,
1.88377451451032));
#25256=CARTESIAN_POINT('Ctrl Pts',(-9.63552812196199,-0.486329821775173,
1.91558919681356));
#25257=CARTESIAN_POINT('Ctrl Pts',(-9.14596582315122,-1.14084454386822,
1.9474038791168));
#25258=CARTESIAN_POINT('Ctrl Pts',(-8.0410366595526,-1.32880668070371,1.98717223199586));
#25259=CARTESIAN_POINT('Ctrl Pts',(-7.13418129904012,-0.331010374245513,
2.03489425545072));
#25260=CARTESIAN_POINT('Ctrl Pts',(-7.48238663245215,0.969214049802592,
2.08261627890558));
#25261=CARTESIAN_POINT('Ctrl Pts',(-8.7664321344037,1.3804141552358,2.13033830236044));
#25262=CARTESIAN_POINT('Ctrl Pts',(-9.62968786527869,0.665267435601966,
2.17010665523949));
#25263=CARTESIAN_POINT('Ctrl Pts',(-9.72653152013487,-0.146020592972697,
2.20192133754273));
#25264=CARTESIAN_POINT('Ctrl Pts',(-9.44181701552787,-0.911952754888573,
2.23373601984598));
#25265=CARTESIAN_POINT('Ctrl Pts',(-8.4351019567227,-1.40432985445164,2.27350437272503));
#25266=CARTESIAN_POINT('Ctrl Pts',(-7.28284501096867,-0.703261816482742,
2.32122639617989));
#25267=CARTESIAN_POINT('Ctrl Pts',(-7.25086675582171,0.64258304887272,2.36894841963475));
#25268=CARTESIAN_POINT('Ctrl Pts',(-8.36437423211283,1.3991651817553,2.41667044308961));
#25269=CARTESIAN_POINT('Ctrl Pts',(-9.60477848348003,0.869389006667507,
2.46439246654448));
#25270=CARTESIAN_POINT('Ctrl Pts',(-9.78954773216159,-0.235910619659578,
2.50416081942353));
#25271=CARTESIAN_POINT('Ctrl Pts',(-9.33205207893577,-0.912967317898448,
2.53597550172677));
#25272=CARTESIAN_POINT('Ctrl Pts',(-8.61556448948887,-1.30584459467476,
2.56779018403001));
#25273=CARTESIAN_POINT('Ctrl Pts',(-7.53210652875583,-1.01958699917634,
2.60755853690906));
#25274=CARTESIAN_POINT('Ctrl Pts',(-7.11938841334767,0.264524506767542,
2.65528056036393));
#25275=CARTESIAN_POINT('Ctrl Pts',(-7.97576986595538,1.30323198402881,2.70300258381879));
#25276=CARTESIAN_POINT('Ctrl Pts',(-9.31287550026506,1.14686320768969,2.75072460727365));
#25277=CARTESIAN_POINT('Ctrl Pts',(-9.90431611236195,-0.0653566335222347,
2.79844663072851));
#25278=CARTESIAN_POINT('Ctrl Pts',(-9.32087302634031,-1.02213130798339,
2.83821498360756));
#25279=CARTESIAN_POINT('Ctrl Pts',(-8.53190702624905,-1.23482903167169,
2.87002966591081));
#25280=CARTESIAN_POINT('Ctrl Pts',(-7.73300931065141,-1.06316047838934,
2.90184434821405));
#25281=CARTESIAN_POINT('Ctrl Pts',(-7.10093312703504,-0.137793890164714,
2.9416127010931));
#25282=CARTESIAN_POINT('Ctrl Pts',(-7.62898068004556,1.10335267503482,2.98933472454796));
#25283=CARTESIAN_POINT('Ctrl Pts',(-8.95622646325114,1.32856620832035,3.03705674800283));
#25284=CARTESIAN_POINT('Ctrl Pts',(-9.86510821618935,0.335471818616583,
3.08477877145768));
#25285=CARTESIAN_POINT('Ctrl Pts',(-9.51925726078488,-0.968240623257094,
3.13250079491255));
#25286=CARTESIAN_POINT('Ctrl Pts',(-8.45202897306244,-1.31007011342866,
3.1722691477916));
#25287=CARTESIAN_POINT('Ctrl Pts',(-7.71620718099674,-0.954719652751151,
3.20408383009485));
#25288=CARTESIAN_POINT('Ctrl Pts',(-7.22435724578901,-0.302192794555079,
3.23589851239808));
#25289=CARTESIAN_POINT('Ctrl Pts',(-7.35179539345088,0.811172885373114,
3.27566686527714));
#25290=CARTESIAN_POINT('Ctrl Pts',(-8.56318915183267,1.40430371135129,3.32338888873199));
#25291=CARTESIAN_POINT('Ctrl Pts',(-9.7142756519776,0.706233245190208,3.37111091218687));
#25292=CARTESIAN_POINT('Ctrl Pts',(-9.75185976306211,-0.639459862898116,
3.41883293564172));
#25293=CARTESIAN_POINT('Ctrl Pts',(-8.63731725129933,-1.3991137340966,3.46655495909659));
#25294=CARTESIAN_POINT('Ctrl Pts',(-7.60657048260336,-0.959358441316762,
3.50632331197563));
#25295=CARTESIAN_POINT('Ctrl Pts',(-7.28260112740917,-0.209190782474353,
3.53813799427888));
#25296=CARTESIAN_POINT('Ctrl Pts',(-7.33757255373269,0.606091868981768,
3.56995267658212));
#25297=CARTESIAN_POINT('Ctrl Pts',(-8.1623997792252,1.36469826678867,3.60972102946117));
#25298=CARTESIAN_POINT('Ctrl Pts',(-9.46659333225728,1.02066601425937,3.65744305291603));
#25299=CARTESIAN_POINT('Ctrl Pts',(-9.88037352419663,-0.260383734703279,
3.7051650763709));
#25300=CARTESIAN_POINT('Ctrl Pts',(-9.028337989291,-1.30265910801724,3.75288709982575));
#25301=CARTESIAN_POINT('Ctrl Pts',(-7.68843599365213,-1.14792819115296,
3.80060912328062));
#25302=CARTESIAN_POINT('Ctrl Pts',(-7.19665294857957,-0.140965900256968,
3.84037747615968));
#25303=CARTESIAN_POINT('Ctrl Pts',(-7.44246893934906,0.638317205013197,
3.87219215846291));
#25304=CARTESIAN_POINT('Ctrl Pts',(-8.01746352197057,1.21891077148926,3.90400684076616));
#25305=CARTESIAN_POINT('Ctrl Pts',(-9.13758203058977,1.25294230621849,3.9437751936452));
#25306=CARTESIAN_POINT('Ctrl Pts',(-9.89878968243401,0.139460413539292,
3.99149721710008));
#25307=CARTESIAN_POINT('Ctrl Pts',(-9.37354847053911,-1.10006537315735,
4.03921924055493));
#25308=CARTESIAN_POINT('Ctrl Pts',(-8.04725495447656,-1.33082068904202,
4.0869412640098));
#25309=CARTESIAN_POINT('Ctrl Pts',(-7.13518679943722,-0.337135278505145,
4.13466328746465));
#25310=CARTESIAN_POINT('Ctrl Pts',(-7.42210844649126,0.746146581012124,
4.17443164034372));
#25311=CARTESIAN_POINT('Ctrl Pts',(-8.11787612020756,1.17464979417261,4.20624632264694));
#25312=CARTESIAN_POINT('Ctrl Pts',(-8.93258781868444,1.23751876777989,4.2380610049502));
#25313=CARTESIAN_POINT('Ctrl Pts',(-9.80194727627518,0.530385292257153,
4.27782935782925));
#25314=CARTESIAN_POINT('Ctrl Pts',(-9.64908535189861,-0.809731212613409,
4.3255513812841));
#25315=CARTESIAN_POINT('Ctrl Pts',(-8.44087433879924,-1.40347244781957,
4.37327340473898));
#25316=CARTESIAN_POINT('Ctrl Pts',(-7.28688212263863,-0.710216022245734,
4.42099542819382));
#25317=CARTESIAN_POINT('Ctrl Pts',(-7.24727497666278,0.638008843471503,
4.4687174516487));
#25318=CARTESIAN_POINT('Ctrl Pts',(-8.17302891837419,1.26951755925708,4.50848580452774));
#25319=CARTESIAN_POINT('Ctrl Pts',(-8.97956615474956,1.13834840961636,4.54030048683099));
#25320=CARTESIAN_POINT('Ctrl Pts',(-9.63682842664003,0.652844583239195,
4.57211516913422));
#25321=CARTESIAN_POINT('Ctrl Pts',(-9.83162187111272,-0.450731029348286,
4.61188352201329));
#25322=CARTESIAN_POINT('Ctrl Pts',(-8.83920954348061,-1.364184250107,4.65960554546813));
#25323=CARTESIAN_POINT('Ctrl Pts',(-7.53702357423647,-1.02269602474283,
4.70732756892301));
#25324=CARTESIAN_POINT('Ctrl Pts',(-7.11789619960128,0.256614238793786,
4.75504959237787));
#25325=CARTESIAN_POINT('Ctrl Pts',(-7.97005828331786,1.30212789132369,4.80277161583273));
#25326=CARTESIAN_POINT('Ctrl Pts',(-9.08334562110853,1.17400715833213,4.84253996871178));
#25327=CARTESIAN_POINT('Ctrl Pts',(-9.60747087368845,0.547109735235215,
4.87435465101502));
#25328=CARTESIAN_POINT('Ctrl Pts',(-9.78687272637736,-0.250087000037372,
4.90616933331827));
#25329=CARTESIAN_POINT('Ctrl Pts',(-9.21213964719043,-1.21211896748734,
4.94593768619731));
#25330=CARTESIAN_POINT('Ctrl Pts',(-7.86397133533361,-1.25360652533042,
4.99365970965218));
#25331=CARTESIAN_POINT('Ctrl Pts',(-7.10261742202974,-0.143362081410263,
5.04138173310704));
#25332=CARTESIAN_POINT('Ctrl Pts',(-7.62267670059613,1.09834676261708,5.0891037565619));
#25333=CARTESIAN_POINT('Ctrl Pts',(-8.95118465747005,1.33146823969133,5.13682578001676));
#25334=CARTESIAN_POINT('Ctrl Pts',(-9.70928520759754,0.506176064395958,
5.17659413289582));
#25335=CARTESIAN_POINT('Ctrl Pts',(-9.69549089650709,-0.310841301673474,
5.20840881519905));
#25336=CARTESIAN_POINT('Ctrl Pts',(-9.30957511823071,-1.03110283164355,
5.2402234975023));
#25337=CARTESIAN_POINT('Ctrl Pts',(-8.24549407463932,-1.38260695875559,
5.27999185038136));
#25338=CARTESIAN_POINT('Ctrl Pts',(-7.1987928772941,-0.531903944756733,
5.32771387383621));
#25339=CARTESIAN_POINT('Ctrl Pts',(-7.34942599645375,0.805859924530717,
5.37543589729107));
#25340=CARTESIAN_POINT('Ctrl Pts',(-8.55514648367598,1.40464253387348,5.42315792074594));
#25341=CARTESIAN_POINT('Ctrl Pts',(-9.71236150745908,0.711726663596795,
5.47087994420079));
#25342=CARTESIAN_POINT('Ctrl Pts',(-9.74570628634277,-0.408412499377414,
5.51064829707986));
#25343=CARTESIAN_POINT('Ctrl Pts',(-9.20071704662944,-1.01725926833835,
5.54246297938309));
#25344=CARTESIAN_POINT('Ctrl Pts',(-8.43761501639986,-1.30946288046008,
5.57427766168634));
#25345=CARTESIAN_POINT('Ctrl Pts',(-7.40291845050727,-0.879083239634173,
5.61404601456539));
#25346=CARTESIAN_POINT('Ctrl Pts',(-7.16794425015288,0.44909827646911,5.66176803802024));
#25347=CARTESIAN_POINT('Ctrl Pts',(-8.15713175655234,1.36223056904336,5.70949006147512));
#25348=CARTESIAN_POINT('Ctrl Pts',(-9.46073272219602,1.02618439821026,5.75721208492997));
#25349=CARTESIAN_POINT('Ctrl Pts',(-9.88252017395179,-0.254976934367327,
5.80493410838483));
#25350=CARTESIAN_POINT('Ctrl Pts',(-9.17485382333125,-1.12390268200446,
5.84470246126389));
#25351=CARTESIAN_POINT('Ctrl Pts',(-8.36434829003804,-1.22777009738866,
5.87651714356712));
#25352=CARTESIAN_POINT('Ctrl Pts',(-7.59606717977041,-0.949468471300325,
5.90833182587037));
#25353=CARTESIAN_POINT('Ctrl Pts',(-7.09516279594638,0.0529877207466158,
5.94810017874943));
#25354=CARTESIAN_POINT('Ctrl Pts',(-7.78646395477307,1.21116807041393,5.99582220220428));
#25355=CARTESIAN_POINT('Ctrl Pts',(-9.13198350831614,1.25452285782982,6.04354422565915));
#25356=CARTESIAN_POINT('Ctrl Pts',(-9.89796813894857,0.147468183392425,
6.09126624911401));
#25357=CARTESIAN_POINT('Ctrl Pts',(-9.37870943707034,-1.09738097014965,
6.13898827256887));
#25358=CARTESIAN_POINT('Ctrl Pts',(-8.2750146032041,-1.29149777108216,6.17875662544793));
#25359=CARTESIAN_POINT('Ctrl Pts',(-7.59410884117921,-0.839751157681671,
6.21057130775117));
#25360=CARTESIAN_POINT('Ctrl Pts',(-7.19518058991253,-0.12661448787792,
6.2423859900544));
#25361=CARTESIAN_POINT('Ctrl Pts',(-7.47225594872512,0.959227519159126,
6.28215434293346));
#25362=CARTESIAN_POINT('Ctrl Pts',(-8.75282774279127,1.38280147349625,6.32987636638832));
#25363=CARTESIAN_POINT('Ctrl Pts',(-9.79874749682902,0.535243584811133,
6.37759838984319));
#25364=CARTESIAN_POINT('Ctrl Pts',(-9.65370337198217,-0.803137791481188,
6.42532041329804));
#25365=CARTESIAN_POINT('Ctrl Pts',(-8.44653368519695,-1.40481907077903,
6.47304243675291));
#25366=CARTESIAN_POINT('Ctrl Pts',(-7.48485426986889,-0.82949627369758,
6.51281078963196));
#25367=CARTESIAN_POINT('Ctrl Pts',(-7.26548531614969,-0.0423591054596432,
6.5446254719352));
#25368=CARTESIAN_POINT('Ctrl Pts',(-7.43038479706196,0.757963217528006,
6.57644015423845));
#25369=CARTESIAN_POINT('Ctrl Pts',(-8.35036750116968,1.39785027228845,6.61620850711748));
#25370=CARTESIAN_POINT('Ctrl Pts',(-9.59593968524807,0.880328341544614,
6.66393053057237));
#25371=CARTESIAN_POINT('Ctrl Pts',(-9.83238070572399,-0.444963381207409,
6.7116525540272));
#25372=CARTESIAN_POINT('Ctrl Pts',(-8.84701587301111,-1.3622194267102,6.75937457748209));
#25373=CARTESIAN_POINT('Ctrl Pts',(-7.54042240671594,-1.02741720391975,
6.80709660093693));
#25374=CARTESIAN_POINT('Ctrl Pts',(-7.1895707383084,0.0368791483633014,
6.846864953816));
#25375=CARTESIAN_POINT('Ctrl Pts',(-7.53867950098618,0.775682729363746,
6.87867963611924));
#25376=CARTESIAN_POINT('Ctrl Pts',(-8.18701931224334,1.27303888808354,6.91049431842248));
#25377=CARTESIAN_POINT('Ctrl Pts',(-9.30142390307262,1.1550303009129,6.95026267130153));
#25378=CARTESIAN_POINT('Ctrl Pts',(-9.90478830936975,-0.0512990105789078,
6.9979846947564));
#25379=CARTESIAN_POINT('Ctrl Pts',(-9.21648716902564,-1.20825365392484,
7.04570671821125));
#25380=CARTESIAN_POINT('Ctrl Pts',(-7.87116044050737,-1.25722813802644,
7.09342874166612));
#25381=CARTESIAN_POINT('Ctrl Pts',(-7.10209883232916,-0.149156273309624,
7.14115076512098));
#25382=CARTESIAN_POINT('Ctrl Pts',(-7.53311276915676,0.885276230514455,
7.18091911800003));
#25383=CARTESIAN_POINT('Ctrl Pts',(-8.28051104488537,1.21558438499352,7.21273380030327));
#25384=CARTESIAN_POINT('Ctrl Pts',(-9.09622983417627,1.16751655505169,7.24454848260651));
#25385=CARTESIAN_POINT('Ctrl Pts',(-9.86179147454805,0.349140728491166,
7.28431683548556));
#25386=CARTESIAN_POINT('Ctrl Pts',(-9.52881196198549,-0.957918435726067,
7.33203885894043));
#25387=CARTESIAN_POINT('Ctrl Pts',(-8.25131089567602,-1.38252829446331,
7.37976088239529));
#25388=CARTESIAN_POINT('Ctrl Pts',(-7.20186011708233,-0.539346481407665,
7.42748290585015));
#25389=CARTESIAN_POINT('Ctrl Pts',(-7.34524279360816,0.801817349980164,
7.47520492930502));
#25390=CARTESIAN_POINT('Ctrl Pts',(-8.34800590386557,1.30210702948025,7.51497328218407));
#25391=CARTESIAN_POINT('Ctrl Pts',(-9.12934199675921,1.06289672573233,7.54678796448731));
#25392=CARTESIAN_POINT('Ctrl Pts',(-9.71478227155839,0.492837655003186,
7.57860264679055));
#25393=CARTESIAN_POINT('Ctrl Pts',(-9.75829474594768,-0.626952630398444,
7.61837099966961));
#25394=CARTESIAN_POINT('Ctrl Pts',(-8.65129661555606,-1.39755898506989,
7.66609302312447));
#25395=CARTESIAN_POINT('Ctrl Pts',(-7.40736890912006,-0.882829572932191,
7.71381504657932));
#25396=CARTESIAN_POINT('Ctrl Pts',(-7.16539436552863,0.441463003054117,
7.76153707003419));
#25397=CARTESIAN_POINT('Ctrl Pts',(-8.15132322416797,1.36191034008795,7.80925909348904));
#25398=CARTESIAN_POINT('Ctrl Pts',(-9.23699515103494,1.08416929897162,7.84902744636811));
#25399=CARTESIAN_POINT('Ctrl Pts',(-9.67137290472358,0.392053971459019,
7.88084212867133));
#25400=CARTESIAN_POINT('Ctrl Pts',(-9.74113641902229,-0.422096328884964,
7.9126568109746));
#25401=CARTESIAN_POINT('Ctrl Pts',(-9.04138768513413,-1.2974107456115,7.95242516385363));
#25402=CARTESIAN_POINT('Ctrl Pts',(-7.70002517381599,-1.15589881049344,
8.0001471873085));
#25403=CARTESIAN_POINT('Ctrl Pts',(-7.09607732311738,0.0472427024613963,
8.04786921076337));
#25404=CARTESIAN_POINT('Ctrl Pts',(-7.77953999755666,1.2070622053182,8.09559123421822));
#25405=CARTESIAN_POINT('Ctrl Pts',(-9.12738126735548,1.25808108395864,8.1433132576731));
#25406=CARTESIAN_POINT('Ctrl Pts',(-9.76670415651867,0.337706235269572,
8.18308161055213));
#25407=CARTESIAN_POINT('Ctrl Pts',(-9.64236730081661,-0.469912490238714,
8.21489629285539));
#25408=CARTESIAN_POINT('Ctrl Pts',(-9.16244480469929,-1.13126115561727,
8.24671097515861));
#25409=CARTESIAN_POINT('Ctrl Pts',(-8.06055772321674,-1.33538973854775,
8.28647932803768));
#25410=CARTESIAN_POINT('Ctrl Pts',(-7.13873614714364,-0.350745642218132,
8.33420135149253));
#25411=CARTESIAN_POINT('Ctrl Pts',(-7.46918871853192,0.954284474147625,
8.3819233749474));
#25412=CARTESIAN_POINT('Ctrl Pts',(-8.74490509614319,1.38422659868658,8.42964539840227));
#25413=CARTESIAN_POINT('Ctrl Pts',(-9.79759510919648,0.540945654416837,
8.47736742185711));
#25414=CARTESIAN_POINT('Ctrl Pts',(-9.67890329798344,-0.57338637539219,
8.51713577473619));
#25415=CARTESIAN_POINT('Ctrl Pts',(-9.05646522431439,-1.10279973367158,
8.54895045703941));
#25416=CARTESIAN_POINT('Ctrl Pts',(-8.26081574743447,-1.28894368178221,
8.58076513934267));
#25417=CARTESIAN_POINT('Ctrl Pts',(-7.29395295285977,-0.722375102372306,
8.6205334922217));
#25418=CARTESIAN_POINT('Ctrl Pts',(-7.24105420847638,0.625393697308591,
8.66825551567658));
#25419=CARTESIAN_POINT('Ctrl Pts',(-8.34481376796175,1.39611890216659,8.71597753913143));
#25420=CARTESIAN_POINT('Ctrl Pts',(-9.59088058679426,0.886589717955089,
8.7636995625863));
#25421=CARTESIAN_POINT('Ctrl Pts',(-9.83523995273739,-0.439897189189682,
8.81142158604116));
#25422=CARTESIAN_POINT('Ctrl Pts',(-9.0163949108726,-1.20495693595518,8.85118993892021));
#25423=CARTESIAN_POINT('Ctrl Pts',(-8.19929004648907,-1.19807943072103,
8.88300462122345));
#25424=CARTESIAN_POINT('Ctrl Pts',(-7.47578742485353,-0.818274723056666,
8.91481930352669));
#25425=CARTESIAN_POINT('Ctrl Pts',(-7.11528810852852,0.242792598858646,
8.95458765640575));
#25426=CARTESIAN_POINT('Ctrl Pts',(-7.9570999824169,1.29665776268705,9.0023096798606));
#25427=CARTESIAN_POINT('Ctrl Pts',(-9.29609107490602,1.15735463711695,9.05003170331547));
#25428=CARTESIAN_POINT('Ctrl Pts',(-9.90505903600862,-0.0432537623661014,
9.09775372677034));
#25429=CARTESIAN_POINT('Ctrl Pts',(-9.2219641867544,-1.20629307445875,9.14547575022517));
#25430=CARTESIAN_POINT('Ctrl Pts',(-8.10214743413141,-1.24911899245564,
9.18524410310427));
#25431=CARTESIAN_POINT('Ctrl Pts',(-7.48870897396143,-0.709303361835556,
9.21705878540747));
#25432=CARTESIAN_POINT('Ctrl Pts',(-7.19005593077866,0.0512977289309366,
9.24887346771074));
#25433=CARTESIAN_POINT('Ctrl Pts',(-7.61166111530691,1.08960052055114,9.28864182058977));
#25434=CARTESIAN_POINT('Ctrl Pts',(-8.93780590948666,1.33580977996377,9.33636384404464));
#25435=CARTESIAN_POINT('Ctrl Pts',(-9.85927926973828,0.354387672557732,
9.38408586749951));
#25436=CARTESIAN_POINT('Ctrl Pts',(-9.53428053627848,-0.952011320785507,
9.43180789095435));
#25437=CARTESIAN_POINT('Ctrl Pts',(-8.25673567435074,-1.38462909701822,
9.47952991440924));
#25438=CARTESIAN_POINT('Ctrl Pts',(-7.38185044108033,-0.684343835633376,
9.51929826728827));
#25439=CARTESIAN_POINT('Ctrl Pts',(-7.27112556056279,0.125253385404266,
9.55111294959153));
#25440=CARTESIAN_POINT('Ctrl Pts',(-7.54291347100558,0.89586287873705,9.58292763189476));
#25441=CARTESIAN_POINT('Ctrl Pts',(-8.54109342884341,1.40523542459937,9.62269598477382));
#25442=CARTESIAN_POINT('Ctrl Pts',(-9.70508436318578,0.723763400728029,
9.67041800822868));
#25443=CARTESIAN_POINT('Ctrl Pts',(-9.75982784765577,-0.621340928856411,
9.71814003168354));
#25444=CARTESIAN_POINT('Ctrl Pts',(-8.65929714385257,-1.39666968270552,
9.7658620551384));
#25445=CARTESIAN_POINT('Ctrl Pts',(-7.41009690516316,-0.887967630214163,
9.81358407859327));
#25446=CARTESIAN_POINT('Ctrl Pts',(-7.20664393228174,0.214044396277857,
9.85335243147231));
#25447=CARTESIAN_POINT('Ctrl Pts',(-7.65261027533608,0.898749939077259,
9.88516711377557));
#25448=CARTESIAN_POINT('Ctrl Pts',(-8.36234433802887,1.30370082465606,9.91698179607878));
#25449=CARTESIAN_POINT('Ctrl Pts',(-9.4504929687235,1.03582739143657,9.95675014895787));
#25450=CARTESIAN_POINT('Ctrl Pts',(-9.88489219289376,-0.24111282979186,
10.0044721724127));
#25451=CARTESIAN_POINT('Ctrl Pts',(-9.04621871645882,-1.294169953828,10.0521941958676));
#25452=CARTESIAN_POINT('Ctrl Pts',(-7.70665745170364,-1.16046084970194,
10.0999162193224));
#25453=CARTESIAN_POINT('Ctrl Pts',(-7.09477865657472,0.0415721592550427,
10.1476382427773));
#25454=CARTESIAN_POINT('Ctrl Pts',(-7.6619399172144,1.00808740648965,10.1874065956564));
#25455=CARTESIAN_POINT('Ctrl Pts',(-8.44719185329995,1.23411186612052,10.2192212779596));
#25456=CARTESIAN_POINT('Ctrl Pts',(-9.24888142608082,1.07599327653697,10.2510359602628));
#25457=CARTESIAN_POINT('Ctrl Pts',(-9.89653349865093,0.161460383961197,
10.2908043131419));
#25458=CARTESIAN_POINT('Ctrl Pts',(-9.38957427574612,-1.08844815703784,
10.3385263365968));
#25459=CARTESIAN_POINT('Ctrl Pts',(-8.06633158847052,-1.33609972099488,
10.3862483600516));
#25460=CARTESIAN_POINT('Ctrl Pts',(-7.1407669831977,-0.358535059182231,
10.4339703835065));
#25461=CARTESIAN_POINT('Ctrl Pts',(-7.46449648071845,0.950845797171473,
10.4816924069613));
#25462=CARTESIAN_POINT('Ctrl Pts',(-8.52578462688086,1.31069450082703,10.5214607598404));
#25463=CARTESIAN_POINT('Ctrl Pts',(-9.26751705207691,0.967852454265898,
10.5532754421436));
#25464=CARTESIAN_POINT('Ctrl Pts',(-9.77034379229997,0.32374615186375,10.5850901244469));
#25465=CARTESIAN_POINT('Ctrl Pts',(-9.66177322247695,-0.791617488423889,
10.6248584773259));
#25466=CARTESIAN_POINT('Ctrl Pts',(-8.46059480690637,-1.40517223619938,
10.6725805007808));
#25467=CARTESIAN_POINT('Ctrl Pts',(-7.29785493107611,-0.726689747322139,
10.7203025242356));
#25468=CARTESIAN_POINT('Ctrl Pts',(-7.23749358360742,0.61817419162873,10.7680245476905));
#25469=CARTESIAN_POINT('Ctrl Pts',(-8.33901539365003,1.39658842360999,10.8157465711454));
#25470=CARTESIAN_POINT('Ctrl Pts',(-9.37705950218062,0.974346730438539,
10.8555149240244));
#25471=CARTESIAN_POINT('Ctrl Pts',(-9.71368278510872,0.229771398542418,
10.8873296063277));
#25472=CARTESIAN_POINT('Ctrl Pts',(-9.67252199622786,-0.586325071818906,
10.9191442886309));
#25473=CARTESIAN_POINT('Ctrl Pts',(-8.86065621577464,-1.35878709239755,
10.95891264151));
#25474=CARTESIAN_POINT('Ctrl Pts',(-7.55082510800669,-1.03688418207522,
11.0066346649648));
#25475=CARTESIAN_POINT('Ctrl Pts',(-7.11541601124033,0.236976652165245,
11.0543566884197));
#25476=CARTESIAN_POINT('Ctrl Pts',(-7.94968367760215,1.29352762936508,11.1020787118745));
#25477=CARTESIAN_POINT('Ctrl Pts',(-9.29201323306557,1.16150346839435,11.1498007353294));
#25478=CARTESIAN_POINT('Ctrl Pts',(-9.80077369478986,0.163011399676013,
11.1895690882084));
#25479=CARTESIAN_POINT('Ctrl Pts',(-9.5681862205647,-0.620321688040218,
11.2213837705117));
#25480=CARTESIAN_POINT('Ctrl Pts',(-9.00310351380729,-1.21056671682165,
11.2531984528149));
#25481=CARTESIAN_POINT('Ctrl Pts',(-7.88372169902902,-1.26355701264146,
11.292966805694));
#25482=CARTESIAN_POINT('Ctrl Pts',(-7.10377186540718,-0.163121975220387,
11.3406888291489));
#25483=CARTESIAN_POINT('Ctrl Pts',(-7.60795259079157,1.08511850750303,11.3884108526037));
#25484=CARTESIAN_POINT('Ctrl Pts',(-8.93014932407102,1.33829493820665,11.4361328760586));
#25485=CARTESIAN_POINT('Ctrl Pts',(-9.85890988118501,0.360193285974161,
11.4838548995135));
#25486=CARTESIAN_POINT('Ctrl Pts',(-9.59036934973144,-0.727790905856776,
11.5236232523925));
#25487=CARTESIAN_POINT('Ctrl Pts',(-8.90195596740575,-1.16801207130932,
11.5554379346957));
#25488=CARTESIAN_POINT('Ctrl Pts',(-8.08842540955644,-1.24466512684449,
11.587252616999));
#25489=CARTESIAN_POINT('Ctrl Pts',(-7.20721876125312,-0.55235128060609,
11.627020969878));
#25490=CARTESIAN_POINT('Ctrl Pts',(-7.33737056595869,0.790161111248255,
11.6747429933329));
#25491=CARTESIAN_POINT('Ctrl Pts',(-8.53535635817352,1.40427229679212,11.7224650167878));
#25492=CARTESIAN_POINT('Ctrl Pts',(-9.70092003171144,0.730652352396493,
11.7701870402426));
#25493=CARTESIAN_POINT('Ctrl Pts',(-9.76334698685623,-0.616708731285964,
11.8179090636975));
#25494=CARTESIAN_POINT('Ctrl Pts',(-8.84841718790923,-1.26379997810216,
11.8576774165765));
#25495=CARTESIAN_POINT('Ctrl Pts',(-8.03977484955831,-1.14630432667695,
11.8894920988798));
#25496=CARTESIAN_POINT('Ctrl Pts',(-7.37438718484698,-0.671997553451563,
11.921306781183));
#25497=CARTESIAN_POINT('Ctrl Pts',(-7.16093809190246,0.428122032515589,
11.9610751340621));
#25498=CARTESIAN_POINT('Ctrl Pts',(-8.13774339449002,1.35824590350669,12.0087971575169));
#25499=CARTESIAN_POINT('Ctrl Pts',(-9.44552413575031,1.03885266727997,12.0565191809718));
#25500=CARTESIAN_POINT('Ctrl Pts',(-9.88625019929875,-0.233178402886088,
12.1042412044267));
#25501=CARTESIAN_POINT('Ctrl Pts',(-9.05191082642372,-1.29296933765629,
12.1519632278815));
#25502=CARTESIAN_POINT('Ctrl Pts',(-7.93661396084778,-1.18371495401975,
12.1917315807606));
#25503=CARTESIAN_POINT('Ctrl Pts',(-7.40195043615906,-0.565780835488536,
12.2235462630638));
#25504=CARTESIAN_POINT('Ctrl Pts',(-7.20907773223965,0.228264364459372,
12.2553609453671));
#25505=CARTESIAN_POINT('Ctrl Pts',(-7.76744120993183,1.19988869797868,12.2951292982461));
#25506=CARTESIAN_POINT('Ctrl Pts',(-9.11471391243231,1.26419483802557,12.3428513217009));
#25507=CARTESIAN_POINT('Ctrl Pts',(-9.89475517645041,0.166999261572729,
12.3905733451558));
#25508=CARTESIAN_POINT('Ctrl Pts',(-9.39579260092668,-1.08333623531818,
12.4382953686107));
#25509=CARTESIAN_POINT('Ctrl Pts',(-8.07142180339368,-1.33891597863226,
12.4860173920655));
#25510=CARTESIAN_POINT('Ctrl Pts',(-7.29945768638114,-0.526576750998625,
12.5257857449446));
#25511=CARTESIAN_POINT('Ctrl Pts',(-7.29941789289706,0.290557055604651,
12.5576004272478));
#25512=CARTESIAN_POINT('Ctrl Pts',(-7.67308431204718,1.0172489206183,12.5894151095511));
#25513=CARTESIAN_POINT('Ctrl Pts',(-8.73106187313777,1.38671759173422,12.6291834624301));
#25514=CARTESIAN_POINT('Ctrl Pts',(-9.79201548042824,0.553857184626279,
12.676905485885));
#25515=CARTESIAN_POINT('Ctrl Pts',(-9.66405233131191,-0.786265175095756,
12.7246275093399));
#25516=CARTESIAN_POINT('Ctrl Pts',(-8.46864205863334,-1.40537484755547,
12.7723495327947));
#25517=CARTESIAN_POINT('Ctrl Pts',(-7.29986180498706,-0.732149971873374,
12.8200715562496));
#25518=CARTESIAN_POINT('Ctrl Pts',(-7.24755781690594,0.387264121095883,
12.8598399091287));
#25519=CARTESIAN_POINT('Ctrl Pts',(-7.78216115368569,1.00525031170328,12.8916545914319));
#25520=CARTESIAN_POINT('Ctrl Pts',(-8.54020679811835,1.31033138360747,12.9234692737351));
#25521=CARTESIAN_POINT('Ctrl Pts',(-9.58204140768946,0.897530868822055,
12.9632376266142));
#25522=CARTESIAN_POINT('Ctrl Pts',(-9.8394680820938,-0.426482168068336,
13.010959650069));
#25523=CARTESIAN_POINT('Ctrl Pts',(-8.86588170522376,-1.35623056055511,
13.0586816735239));
#25524=CARTESIAN_POINT('Ctrl Pts',(-7.55677830450565,-1.04230255481654,
13.1064036969788));
#25525=CARTESIAN_POINT('Ctrl Pts',(-7.11336120643524,0.231534283907112,
13.1541257204336));
#25526=CARTESIAN_POINT('Ctrl Pts',(-7.80621519412012,1.11231630600824,13.1938940733127));
#25527=CARTESIAN_POINT('Ctrl Pts',(-8.61484608482721,1.22989071679448,13.2257087556159));
#25528=CARTESIAN_POINT('Ctrl Pts',(-9.38772873712336,0.964635999103795,
13.2575234379192));
#25529=CARTESIAN_POINT('Ctrl Pts',(-9.9055329419163,-0.0291961920663647,
13.2972917907982));
#25530=CARTESIAN_POINT('Ctrl Pts',(-9.23393888925362,-1.19891429613191,
13.345013814253));
#25531=CARTESIAN_POINT('Ctrl Pts',(-7.88934617768876,-1.26504255457979,
13.392735837708));
#25532=CARTESIAN_POINT('Ctrl Pts',(-7.10472886292055,-0.171114688619423,
13.4404578611628));
#25533=CARTESIAN_POINT('Ctrl Pts',(-7.6028378109668,1.08234711392059,13.4881798846177));
#25534=CARTESIAN_POINT('Ctrl Pts',(-8.70308805672016,1.29512167872337,13.5279482374967));
#25535=CARTESIAN_POINT('Ctrl Pts',(-9.39154431231752,0.85496756525127,13.5597629198));
#25536=CARTESIAN_POINT('Ctrl Pts',(-9.80248881225848,0.148686971262036,
13.5915776021032));
#25537=CARTESIAN_POINT('Ctrl Pts',(-9.54383650121592,-0.941690303216714,
13.6313459549822));
#25538=CARTESIAN_POINT('Ctrl Pts',(-8.27061936204929,-1.38688366691718,
13.6790679784371));
#25539=CARTESIAN_POINT('Ctrl Pts',(-7.21050033312947,-0.557154704495852,
13.726790001892));
#25540=CARTESIAN_POINT('Ctrl Pts',(-7.33286483455415,0.783490451893329,
13.7745120253468));
#25541=CARTESIAN_POINT('Ctrl Pts',(-8.52967502452601,1.4055229138518,13.8222340488017));
#25542=CARTESIAN_POINT('Ctrl Pts',(-9.50095684039326,0.846563834067789,
13.8620024016807));
#25543=CARTESIAN_POINT('Ctrl Pts',(-9.73362060837031,0.0632534035562258,
13.893817083984));
#25544=CARTESIAN_POINT('Ctrl Pts',(-9.58229424135026,-0.739745967627832,
13.9256317662872));
#25545=CARTESIAN_POINT('Ctrl Pts',(-8.67327669837474,-1.39511664538971,
13.9654001191663));
#25546=CARTESIAN_POINT('Ctrl Pts',(-7.41912137251077,-0.898756460486,14.0131221426211));
#25547=CARTESIAN_POINT('Ctrl Pts',(-7.16027701249887,0.422342363920669,
14.060844166076));
#25548=CARTESIAN_POINT('Ctrl Pts',(-8.12997144830433,1.35614920033099,14.1085661895309));
#25549=CARTESIAN_POINT('Ctrl Pts',(-9.44204586070303,1.04351562747063,14.1562882129857));
#25550=CARTESIAN_POINT('Ctrl Pts',(-9.81086581180923,-0.0146882575975216,
14.1960565658648));
#25551=CARTESIAN_POINT('Ctrl Pts',(-9.474315050416,-0.759296372301599,14.227871248168));
#25552=CARTESIAN_POINT('Ctrl Pts',(-8.83448841538654,-1.26755766001138,
14.2596859304713));
#25553=CARTESIAN_POINT('Ctrl Pts',(-7.71824565582048,-1.16843288801694,
14.2994542833503));
#25554=CARTESIAN_POINT('Ctrl Pts',(-7.09454453567121,0.0275085517186915,
14.3471763068052));
#25555=CARTESIAN_POINT('Ctrl Pts',(-7.76315975106791,1.19595033473491,14.3948983302601));
#25556=CARTESIAN_POINT('Ctrl Pts',(-9.10746452361569,1.26769421990389,14.4426203537149));
#25557=CARTESIAN_POINT('Ctrl Pts',(-9.89517559599181,0.172801402766538,
14.4903423771698));
#25558=CARTESIAN_POINT('Ctrl Pts',(-9.48173640552899,-0.868779921226412,
14.5301107300488));
#25559=CARTESIAN_POINT('Ctrl Pts',(-8.740037375894,-1.21169420921505,14.561925412352));
#25560=CARTESIAN_POINT('Ctrl Pts',(-7.92362170827253,-1.17744341108029,
14.5937400946553));
#25561=CARTESIAN_POINT('Ctrl Pts',(-7.14431466438971,-0.372145857416179,
14.6335084475344));
#25562=CARTESIAN_POINT('Ctrl Pts',(-7.4551179039004,0.940363327686876,14.6812304709892));
#25563=CARTESIAN_POINT('Ctrl Pts',(-8.72524721766598,1.38654045969507,14.7289524944441));
#25564=CARTESIAN_POINT('Ctrl Pts',(-9.78882267771499,0.561246726270562,
14.7766745178989));
#25565=CARTESIAN_POINT('Ctrl Pts',(-9.66816649404496,-0.782152358472022,
14.8243965413538));
#25566=CARTESIAN_POINT('Ctrl Pts',(-8.67401702075417,-1.29934714241638,
14.8641648942329));
#25567=CARTESIAN_POINT('Ctrl Pts',(-7.88874307551789,-1.07339916673311,
14.8959795765361));
#25568=CARTESIAN_POINT('Ctrl Pts',(-7.2937355886856,-0.513333317189202,
14.9277942588393));
#25569=CARTESIAN_POINT('Ctrl Pts',(-7.23127127492183,0.605559803923401,
14.9675626117184));
#25570=CARTESIAN_POINT('Ctrl Pts',(-8.32506434800626,1.39479723197527,15.0152846351733));
#25571=CARTESIAN_POINT('Ctrl Pts',(-9.577528174018,0.901201308551766,15.0630066586281));
#25572=CARTESIAN_POINT('Ctrl Pts',(-9.84188831197631,-0.418804799962236,
15.110728682083));
#25573=CARTESIAN_POINT('Ctrl Pts',(-8.87168403101893,-1.35581207733519,
15.1584507055378));
#25574=CARTESIAN_POINT('Ctrl Pts',(-7.78146541211255,-1.09649119427727,
15.1982190584169));
#25575=CARTESIAN_POINT('Ctrl Pts',(-7.33543257577158,-0.411829247736474,
15.2300337407201));
#25576=CARTESIAN_POINT('Ctrl Pts',(-7.25189509248559,0.401023575788254,
15.2618484230234));
#25577=CARTESIAN_POINT('Ctrl Pts',(-7.93672527856798,1.28805862362876,15.3016167759024));
#25578=CARTESIAN_POINT('Ctrl Pts',(-9.2802898119901,1.1692775185069,15.3493387993573));
#25579=CARTESIAN_POINT('Ctrl Pts',(-9.90452303617752,-0.023468903252238,
15.3970608228122));
#25580=CARTESIAN_POINT('Ctrl Pts',(-9.24078902202083,-1.19468910281144,
15.444782846267));
#25581=CARTESIAN_POINT('Ctrl Pts',(-7.89401458685209,-1.26852769992676,
15.4925048697219));
#25582=CARTESIAN_POINT('Ctrl Pts',(-7.23918325907841,-0.359093832643389,
15.5322732226009));
#25583=CARTESIAN_POINT('Ctrl Pts',(-7.34985615927118,0.450492361508205,
15.5640879049042));
#25584=CARTESIAN_POINT('Ctrl Pts',(-7.81846044934637,1.11991416460057,15.5959025872074));
#25585=CARTESIAN_POINT('Ctrl Pts',(-8.91685053280032,1.3425736633541,15.6356709400865));
#25586=CARTESIAN_POINT('Ctrl Pts',(-9.85499739493844,0.373849720226626,
15.6833929635413));
#25587=CARTESIAN_POINT('Ctrl Pts',(-9.54706276738189,-0.936893375628721,
15.7311149869962));
#25588=CARTESIAN_POINT('Ctrl Pts',(-8.27810821927371,-1.38780367521502,
15.7788370104511));
#25589=CARTESIAN_POINT('Ctrl Pts',(-7.21262708385088,-0.563549955867792,
15.8265590339059));
#25590=CARTESIAN_POINT('Ctrl Pts',(-7.32972690286773,0.778060702080066,
15.8742810573608));
#25591=CARTESIAN_POINT('Ctrl Pts',(-8.52189522723517,1.40525997677246,15.9220030808156));
#25592=CARTESIAN_POINT('Ctrl Pts',(-9.69354285869501,0.741326568114595,
15.9697251042705));
#25593=CARTESIAN_POINT('Ctrl Pts',(-9.76973983670298,-0.602944691238737,
16.0174471277254));
#25594=CARTESIAN_POINT('Ctrl Pts',(-8.67795139285792,-1.39448976690683,
16.0651691511802));
#25595=CARTESIAN_POINT('Ctrl Pts',(-7.63474546540348,-0.984905318057682,
16.1049375040593));
#25596=CARTESIAN_POINT('Ctrl Pts',(-7.28920191986363,-0.244422239744572,
16.1367521863625));
#25597=CARTESIAN_POINT('Ctrl Pts',(-7.32046026829885,0.572095495672729,
16.1685668686657));
#25598=CARTESIAN_POINT('Ctrl Pts',(-8.1229455399191,1.35433038087558,16.2083352215448));
#25599=CARTESIAN_POINT('Ctrl Pts',(-9.43656254042288,1.04828480643365,16.2560572449997));
#25600=CARTESIAN_POINT('Ctrl Pts',(-9.88735051158488,-0.220214228827959,
16.3037792684545));
#25601=CARTESIAN_POINT('Ctrl Pts',(-9.06591783859971,-1.2867785768872,16.3515012919094));
#25602=CARTESIAN_POINT('Ctrl Pts',(-7.72209157421216,-1.17099611903586,
16.3992233153643));
#25603=CARTESIAN_POINT('Ctrl Pts',(-7.20129244434704,-0.17873011326985,
16.4389916682433));
#25604=CARTESIAN_POINT('Ctrl Pts',(-7.42439036505487,0.607358648640506,
16.4708063505466));
#25605=CARTESIAN_POINT('Ctrl Pts',(-7.98229360457716,1.20439403072933,16.5026210328498));
#25606=CARTESIAN_POINT('Ctrl Pts',(-9.100952891,1.27091739730054,16.5423893857288));
#25607=CARTESIAN_POINT('Ctrl Pts',(-9.8941533483515,0.179994843177065,16.5901114091837));
#25608=CARTESIAN_POINT('Ctrl Pts',(-9.40510470497528,-1.07425147771346,
16.6378334326385));
#25609=CARTESIAN_POINT('Ctrl Pts',(-8.08606633854649,-1.34339894468471,
16.6855554560935));
#25610=CARTESIAN_POINT('Ctrl Pts',(-7.145545368936,-0.376600459845053,16.7332774795483));
#25611=CARTESIAN_POINT('Ctrl Pts',(-7.40090908890966,0.714551673218083,
16.7730458324274));
#25612=CARTESIAN_POINT('Ctrl Pts',(-8.08394846882832,1.16306574288832,16.8048605147306));
#25613=CARTESIAN_POINT('Ctrl Pts',(-8.89649255801945,1.24955134806578,16.8366751970338));
#25614=CARTESIAN_POINT('Ctrl Pts',(-9.786007031784,0.567944701423324,16.8764435499129));
#25615=CARTESIAN_POINT('Ctrl Pts',(-9.67209996192896,-0.776043466300687,
16.9241655733677));
#25616=CARTESIAN_POINT('Ctrl Pts',(-8.48162831789962,-1.40459717952674,
16.9718875968226));
#25617=CARTESIAN_POINT('Ctrl Pts',(-7.30800368174657,-0.745121842437952,
17.0196096202774));
#25618=CARTESIAN_POINT('Ctrl Pts',(-7.22928743756428,0.601385776393804,
17.0673316437324));
#25619=CARTESIAN_POINT('Ctrl Pts',(-8.13632495384472,1.25949409775313,17.1070999966114));
#25620=CARTESIAN_POINT('Ctrl Pts',(-8.94632905408739,1.15178607994229,17.1389146789146));
#25621=CARTESIAN_POINT('Ctrl Pts',(-9.61740393037904,0.685560630316964,
17.1707293612179));
#25622=CARTESIAN_POINT('Ctrl Pts',(-9.84414133781144,-0.411897235285352,
17.2104977140969));
#25623=CARTESIAN_POINT('Ctrl Pts',(-8.87865560148491,-1.35376575451348,
17.2582197375518));
#25624=CARTESIAN_POINT('Ctrl Pts',(-7.56710801788738,-1.05021107655027,
17.3059417610066));
#25625=CARTESIAN_POINT('Ctrl Pts',(-7.11103130626957,0.216397205310442,
17.3536637844615));
#25626=CARTESIAN_POINT('Ctrl Pts',(-7.93249344605425,1.28620044303824,17.4013858079163));
#25627=CARTESIAN_POINT('Ctrl Pts',(-9.04902998642944,1.19044151283572,17.4411541607954));
#25628=CARTESIAN_POINT('Ctrl Pts',(-9.59112719047142,0.579018352620608,
17.4729688430987));
#25629=CARTESIAN_POINT('Ctrl Pts',(-9.79358830678465,-0.212636342217181,
17.5047835254019));
#25630=CARTESIAN_POINT('Ctrl Pts',(-9.24701566858587,-1.19094200502388,
17.5445518782809));
#25631=CARTESIAN_POINT('Ctrl Pts',(-7.9006191498078,-1.27153622797434,17.5922739017358));
#25632=CARTESIAN_POINT('Ctrl Pts',(-7.10736636384562,-0.183854048235282,
17.6399959251907));
#25633=CARTESIAN_POINT('Ctrl Pts',(-7.59117194467839,1.07242405255042,17.6877179486456));
#25634=CARTESIAN_POINT('Ctrl Pts',(-8.91235513076913,1.34400093548014,17.7354399721004));
#25635=CARTESIAN_POINT('Ctrl Pts',(-9.69408654676645,0.541056596219814,
17.7752083249795));
#25636=CARTESIAN_POINT('Ctrl Pts',(-9.70400806777014,-0.276016976292779,
17.8070230072827));
#25637=CARTESIAN_POINT('Ctrl Pts',(-9.33915697445163,-1.0071745100581,17.8388376895859));
#25638=CARTESIAN_POINT('Ctrl Pts',(-8.28572482191837,-1.38941045645308,
17.878606042465));
#25639=CARTESIAN_POINT('Ctrl Pts',(-7.21477688206173,-0.569441234672508,
17.9263280659199));
#25640=CARTESIAN_POINT('Ctrl Pts',(-7.32652435883821,0.772130607605336,
17.9740500893747));
#25641=CARTESIAN_POINT('Ctrl Pts',(-8.51436022445611,1.40565129622602,18.0217721128296));
#25642=CARTESIAN_POINT('Ctrl Pts',(-9.69119642771782,0.746609897493594,
18.0694941362844));
#25643=CARTESIAN_POINT('Ctrl Pts',(-9.75703384557922,-0.372089817853069,
18.1092624891635));
#25644=CARTESIAN_POINT('Ctrl Pts',(-9.22994300794511,-0.996495862314252,
18.1410771714668));
#25645=CARTESIAN_POINT('Ctrl Pts',(-8.4756421899822,-1.31072179297238,18.1728918537699));
#25646=CARTESIAN_POINT('Ctrl Pts',(-7.42889170154707,-0.910550537547681,
18.212660206649));
#25647=CARTESIAN_POINT('Ctrl Pts',(-7.15547234904076,0.410252578827254,
18.2603822301039));
#25648=CARTESIAN_POINT('Ctrl Pts',(-8.11774393575135,1.35170672001962,18.3081042535588));
#25649=CARTESIAN_POINT('Ctrl Pts',(-9.43054799017888,1.05363286803438,18.3558262770136));
#25650=CARTESIAN_POINT('Ctrl Pts',(-9.88933737698507,-0.214748507224885,
18.4035483004685));
#25651=CARTESIAN_POINT('Ctrl Pts',(-9.20718549273468,-1.10384491680092,
18.4433166533475));
#25652=CARTESIAN_POINT('Ctrl Pts',(-8.40003557935687,-1.23118963326648,
18.4751313356508));
#25653=CARTESIAN_POINT('Ctrl Pts',(-7.62400167613423,-0.975300906421168,
18.506946017954));
#25654=CARTESIAN_POINT('Ctrl Pts',(-7.09421676335546,0.0121967213730914,
18.5467143708331));
#25655=CARTESIAN_POINT('Ctrl Pts',(-7.75161611674647,1.18995098466898,18.5944363942879));
#25656=CARTESIAN_POINT('Ctrl Pts',(-9.09531080539251,1.27233478321708,18.6421584177428));
#25657=CARTESIAN_POINT('Ctrl Pts',(-9.89309979053325,0.187975413936358,
18.6898804411977));
#25658=CARTESIAN_POINT('Ctrl Pts',(-9.41018558167302,-1.07141844083329,
18.7376024646525));
#25659=CARTESIAN_POINT('Ctrl Pts',(-8.31258890865753,-1.29748294953091,
18.7773708175316));
#25660=CARTESIAN_POINT('Ctrl Pts',(-7.61886014196042,-0.865686634430366,
18.8091854998348));
#25661=CARTESIAN_POINT('Ctrl Pts',(-7.19940452759574,-0.164427305041153,
18.841000182138));
#25662=CARTESIAN_POINT('Ctrl Pts',(-7.44485181710885,0.928998159623897,
18.8807685350171));
#25663=CARTESIAN_POINT('Ctrl Pts',(-8.71259205746091,1.38955618804453,18.9284905584719));
#25664=CARTESIAN_POINT('Ctrl Pts',(-9.78266761091162,0.572708089273526,
18.9762125819268));
#25665=CARTESIAN_POINT('Ctrl Pts',(-9.6765246946901,-0.769318806095816,
19.0239346053817));
#25666=CARTESIAN_POINT('Ctrl Pts',(-8.48732435991086,-1.40577899991123,
19.0716566288365));
#25667=CARTESIAN_POINT('Ctrl Pts',(-7.5093539869978,-0.858606661052929,
19.1114249817156));
#25668=CARTESIAN_POINT('Ctrl Pts',(-7.26723453363784,-0.0781671504038373,
19.1432396640188));
#25669=CARTESIAN_POINT('Ctrl Pts',(-7.40883903449548,0.726603515571496,
19.1750543463221));
#25670=CARTESIAN_POINT('Ctrl Pts',(-8.30986460269802,1.39291916460931,19.2148226992011));
#25671=CARTESIAN_POINT('Ctrl Pts',(-9.56993078200403,0.911761977902418,
19.262544722656));
#25672=CARTESIAN_POINT('Ctrl Pts',(-9.84473247440981,-0.406109994790532,
19.3102667461109));
#25673=CARTESIAN_POINT('Ctrl Pts',(-8.88640162358035,-1.3515752172642,19.3579887695657));
#25674=CARTESIAN_POINT('Ctrl Pts',(-7.57064242851217,-1.05483163242354,
19.4057107930206));
#25675=CARTESIAN_POINT('Ctrl Pts',(-7.18905241771698,-0.00116532738733117,
19.4454791458996));
#25676=CARTESIAN_POINT('Ctrl Pts',(-7.51657390327246,0.747458300330247,
19.4772938282029));
#25677=CARTESIAN_POINT('Ctrl Pts',(-8.15020726559116,1.26341994777524,19.5091085105061));
#25678=CARTESIAN_POINT('Ctrl Pts',(-9.26756713176743,1.17780132733557,19.5488768633852));
#25679=CARTESIAN_POINT('Ctrl Pts',(-9.90568535581634,-0.0105101413827072,
19.59659888684));
#25680=CARTESIAN_POINT('Ctrl Pts',(-9.25124918710935,-1.18695215340324,
19.6443209102949));
#25681=CARTESIAN_POINT('Ctrl Pts',(-7.90791032709937,-1.27494768593567,
19.6920429337497));
#25682=CARTESIAN_POINT('Ctrl Pts',(-7.10701614127563,-0.189660849350813,
19.7397649572047));
#25683=CARTESIAN_POINT('Ctrl Pts',(-7.50782908869113,0.856844095640571,
19.7795333100836));
#25684=CARTESIAN_POINT('Ctrl Pts',(-8.24532696405019,1.20870279358388,19.8113479923869));
#25685=CARTESIAN_POINT('Ctrl Pts',(-9.0620971317096,1.18432754591179,19.8431626746901));
#25686=CARTESIAN_POINT('Ctrl Pts',(-9.85108578157514,0.388513164858798,
19.8829310275692));
#25687=CARTESIAN_POINT('Ctrl Pts',(-9.55617765393731,-0.927658636542429,
19.9306530510241));
#25688=CARTESIAN_POINT('Ctrl Pts',(-8.29153691019929,-1.38916301987629,
19.9783750744789));
#25689=CARTESIAN_POINT('Ctrl Pts',(-7.21805881404244,-0.57679162474335,
20.0260970979338));
#25690=CARTESIAN_POINT('Ctrl Pts',(-7.32246023424974,0.767968338227514,
20.0738191213886));
#25691=CARTESIAN_POINT('Ctrl Pts',(-8.31028248984177,1.29714771241403,20.1135874742677));
#25692=CARTESIAN_POINT('Ctrl Pts',(-9.09823143854941,1.08071270205753,20.1454021565709));
#25693=CARTESIAN_POINT('Ctrl Pts',(-9.69996837905173,0.527883330630518,
20.1772168388742));
#25694=CARTESIAN_POINT('Ctrl Pts',(-9.77595908553397,-0.590172585339566,
20.2169851917532));
#25695=CARTESIAN_POINT('Ctrl Pts',(-8.69179035992437,-1.39257970704315,
20.2647072152081));
#25696=CARTESIAN_POINT('Ctrl Pts',(-7.43344900514689,-0.914166139702682,
20.312429238663));
#25697=CARTESIAN_POINT('Ctrl Pts',(-7.1531451156656,0.40254652299194,20.3601512621178));
#25698=CARTESIAN_POINT('Ctrl Pts',(-8.11194714289106,1.35121806105923,20.4078732855727));
#25699=CARTESIAN_POINT('Ctrl Pts',(-9.20522191726533,1.10510043384764,20.4476416384518));
#25700=CARTESIAN_POINT('Ctrl Pts',(-9.65950205965873,0.425882345377853,
20.479456320755));
#25701=CARTESIAN_POINT('Ctrl Pts',(-9.75286301069235,-0.385900502617611,
20.5112710030582));
#25702=CARTESIAN_POINT('Ctrl Pts',(-9.07881080904158,-1.28115311956834,
20.5510393559372));
#25703=CARTESIAN_POINT('Ctrl Pts',(-7.73390653914345,-1.17862741859382,
20.5987613793922));
#25704=CARTESIAN_POINT('Ctrl Pts',(-7.09529762703471,0.00648066252536313,
20.646483402847));
#25705=CARTESIAN_POINT('Ctrl Pts',(-7.7448142288305,1.1856459141124,20.6942054263018));
#25706=CARTESIAN_POINT('Ctrl Pts',(-9.09060724228286,1.2757579526721,20.7419274497568));
#25707=CARTESIAN_POINT('Ctrl Pts',(-9.75637034345738,0.374324032841098,
20.7816958026357));
#25708=CARTESIAN_POINT('Ctrl Pts',(-9.65552312703059,-0.43656282635472,
20.8135104849391));
#25709=CARTESIAN_POINT('Ctrl Pts',(-9.19499524498417,-1.11156040363579,
20.8453251672422));
#25710=CARTESIAN_POINT('Ctrl Pts',(-8.09949610707047,-1.34758001624817,
20.8850935201213));
#25711=CARTESIAN_POINT('Ctrl Pts',(-7.14948819284198,-0.390102090939205,
20.9328155435762));
#25712=CARTESIAN_POINT('Ctrl Pts',(-7.44192932700205,0.923968184810892,
20.980537567031));
#25713=CARTESIAN_POINT('Ctrl Pts',(-8.70463139019127,1.39075079607264,21.0282595904859));
#25714=CARTESIAN_POINT('Ctrl Pts',(-9.78135023333184,0.578374314768165,
21.0759816139408));
#25715=CARTESIAN_POINT('Ctrl Pts',(-9.69504657087012,-0.538932848259564,
21.1157499668198));
#25716=CARTESIAN_POINT('Ctrl Pts',(-9.08823434389678,-1.08618651948812,
21.147564649123));
#25717=CARTESIAN_POINT('Ctrl Pts',(-8.29832191286535,-1.29534198984334,
21.1793793314263));
#25718=CARTESIAN_POINT('Ctrl Pts',(-7.315424393124,-0.757070604393955,21.2191476843053));
#25719=CARTESIAN_POINT('Ctrl Pts',(-7.22343538367285,0.588595415348976,
21.2668697077602));
#25720=CARTESIAN_POINT('Ctrl Pts',(-8.30436345332364,1.39102735314789,21.314591731215));
#25721=CARTESIAN_POINT('Ctrl Pts',(-9.56469210780724,0.917873901035059,
21.36231375467));
#25722=CARTESIAN_POINT('Ctrl Pts',(-9.84744349518117,-0.400962960555038,
21.4100357781248));
#25723=CARTESIAN_POINT('Ctrl Pts',(-9.05114553138379,-1.18946354492994,
21.4498041310038));
#25724=CARTESIAN_POINT('Ctrl Pts',(-8.23418522462471,-1.20630149782281,
21.4816188133071));
#25725=CARTESIAN_POINT('Ctrl Pts',(-7.49996530886433,-0.847652958472259,
21.5134334956103));
#25726=CARTESIAN_POINT('Ctrl Pts',(-7.10882542066799,0.202505699335723,
21.5532018484894));
#25727=CARTESIAN_POINT('Ctrl Pts',(-7.9196993471952,1.28035656556392,21.6009238719442));
#25728=CARTESIAN_POINT('Ctrl Pts',(-9.26216909691203,1.17996992474953,21.6486458953991));
#25729=CARTESIAN_POINT('Ctrl Pts',(-9.90572249357285,-0.00246042508295246,
21.696367918854));
#25730=CARTESIAN_POINT('Ctrl Pts',(-9.25666700161002,-1.18483345543481,
21.7440899423088));
#25731=CARTESIAN_POINT('Ctrl Pts',(-8.13856470554957,-1.26013866276976,
21.7838582951879));
#25732=CARTESIAN_POINT('Ctrl Pts',(-7.50971904305091,-0.738352507113889,
21.8156729774912));
#25733=CARTESIAN_POINT('Ctrl Pts',(-7.18911897548137,0.0132612608227678,
21.8474876597943));
#25734=CARTESIAN_POINT('Ctrl Pts',(-7.58041481673441,1.06336181949582,21.8872560126734));
#25735=CARTESIAN_POINT('Ctrl Pts',(-8.89885602513675,1.34795239301706,21.9349780361283));
#25736=CARTESIAN_POINT('Ctrl Pts',(-9.84842236738186,0.393684994310642,
21.9827000595832));
#25737=CARTESIAN_POINT('Ctrl Pts',(-9.56147249923753,-0.921595310312913,
22.030422083038));
#25738=CARTESIAN_POINT('Ctrl Pts',(-8.29702036984018,-1.39110550936414,
22.0781441064929));
#25739=CARTESIAN_POINT('Ctrl Pts',(-7.40218118543914,-0.71650455119125,
22.1179124593719));
#25740=CARTESIAN_POINT('Ctrl Pts',(-7.2680082514545,0.0895384273548286,
22.1497271416752));
#25741=CARTESIAN_POINT('Ctrl Pts',(-7.51731843588521,0.867710703535758,
22.1815418239784));
#25742=CARTESIAN_POINT('Ctrl Pts',(-8.50029588260379,1.4058361145228,22.2213101768575));
#25743=CARTESIAN_POINT('Ctrl Pts',(-9.68357303965896,0.758430380734344,
22.2690322003123));
#25744=CARTESIAN_POINT('Ctrl Pts',(-9.77732868873411,-0.584518756361056,
22.3167542237672));
#25745=CARTESIAN_POINT('Ctrl Pts',(-8.69976171084787,-1.39145860215367,
22.3644762472221));
#25746=CARTESIAN_POINT('Ctrl Pts',(-7.43632495976926,-0.919222865921664,
22.4121982706769));
#25747=CARTESIAN_POINT('Ctrl Pts',(-7.20097704672433,0.176420770728819,
22.4519666235559));
#25748=CARTESIAN_POINT('Ctrl Pts',(-7.62688525551803,0.873779973119977,
22.4837813058592));
#25749=CARTESIAN_POINT('Ctrl Pts',(-8.32456863272794,1.29915694081149,22.5155959881624));
#25750=CARTESIAN_POINT('Ctrl Pts',(-9.42003270766891,1.06297463999032,22.5553643410415));
#25751=CARTESIAN_POINT('Ctrl Pts',(-9.89130605755087,-0.200821405359406,
22.6030863644963));
#25752=CARTESIAN_POINT('Ctrl Pts',(-9.08354575717079,-1.27777349514265,
22.6508083879512));
#25753=CARTESIAN_POINT('Ctrl Pts',(-7.74066841505343,-1.18299506623269,
22.6985304114061));
#25754=CARTESIAN_POINT('Ctrl Pts',(-7.09416406785961,0.000774820024847972,
22.7462524348609));
#25755=CARTESIAN_POINT('Ctrl Pts',(-7.63303797081583,0.983342138543073,
22.78602078774));
#25756=CARTESIAN_POINT('Ctrl Pts',(-8.4113998990915,1.23205958483199,22.8178354700432));
#25757=CARTESIAN_POINT('Ctrl Pts',(-9.21734045606203,1.09727279724702,22.8496501523464));
#25758=CARTESIAN_POINT('Ctrl Pts',(-9.89125969775638,0.201920087762355,
22.8894185052255));
#25759=CARTESIAN_POINT('Ctrl Pts',(-9.42078661216186,-1.06217409001151,
22.9371405286804));
#25760=CARTESIAN_POINT('Ctrl Pts',(-8.1052881443608,-1.34812214083849,22.9848625521353));
#25761=CARTESIAN_POINT('Ctrl Pts',(-7.1517442241385,-0.397829291888364,
23.0325845755901));
#25762=CARTESIAN_POINT('Ctrl Pts',(-7.43733885659921,0.920394786354866,
23.080306599045));
#25763=CARTESIAN_POINT('Ctrl Pts',(-8.48773712657024,1.31089074427156,23.120074951924));
#25764=CARTESIAN_POINT('Ctrl Pts',(-9.23910650345744,0.989718331144916,
23.1518896342273));
#25765=CARTESIAN_POINT('Ctrl Pts',(-9.76041357098137,0.360475452101273,
23.1837043165305));
#25766=CARTESIAN_POINT('Ctrl Pts',(-9.68425682465483,-0.757569166282248,
23.2234726694096));
#25767=CARTESIAN_POINT('Ctrl Pts',(-8.50138980836165,-1.40572395976629,
23.2711946928644));
#25768=CARTESIAN_POINT('Ctrl Pts',(-7.31944993986188,-0.761270195862776,
23.3189167163193));
#25769=CARTESIAN_POINT('Ctrl Pts',(-7.22008577008131,0.581275620235319,
23.3666387397741));
#25770=CARTESIAN_POINT('Ctrl Pts',(-8.29855389552885,1.39132840675251,23.414360763229));
#25771=CARTESIAN_POINT('Ctrl Pts',(-9.34841435168295,0.999388817898224,
23.4541291161081));
#25772=CARTESIAN_POINT('Ctrl Pts',(-9.70650359585349,0.264895963823484,
23.4859437984113));
#25773=CARTESIAN_POINT('Ctrl Pts',(-9.68904344055486,-0.552051281997461,
23.5177584807146));
#25774=CARTESIAN_POINT('Ctrl Pts',(-8.89993661427864,-1.34774848284182,
23.5575268335936));
#25775=CARTESIAN_POINT('Ctrl Pts',(-7.58131548221499,-1.06399273466057,
23.6052488570485));
#25776=CARTESIAN_POINT('Ctrl Pts',(-7.10912204955266,0.196695913939611,
23.6529708805033));
#25777=CARTESIAN_POINT('Ctrl Pts',(-7.91237700309648,1.27701252779228,23.7006929039582));
#25778=CARTESIAN_POINT('Ctrl Pts',(-9.25797257256842,1.1839986687818,23.7484149274131));
#25779=CARTESIAN_POINT('Ctrl Pts',(-9.79549521473797,0.200691479820764,
23.7881832802921));
#25780=CARTESIAN_POINT('Ctrl Pts',(-9.58573819775806,-0.589061426666565,
23.8199979625954));
#25781=CARTESIAN_POINT('Ctrl Pts',(-9.03802252939069,-1.19545668233927,
23.8518126448985));
#25782=CARTESIAN_POINT('Ctrl Pts',(-7.9206499604527,-1.28090936452179,23.8915809977777));
#25783=CARTESIAN_POINT('Ctrl Pts',(-7.10909375743094,-0.203572117468884,
23.9393030212324));
#25784=CARTESIAN_POINT('Ctrl Pts',(-7.57683792315452,1.05877407196975,23.9870250446874));
#25785=CARTESIAN_POINT('Ctrl Pts',(-8.89113054465059,1.3502143087931,24.0347470681422));
#25786=CARTESIAN_POINT('Ctrl Pts',(-9.84788465423753,0.399477442810103,
24.0824690915971));
#25787=CARTESIAN_POINT('Ctrl Pts',(-9.61103076409583,-0.6958416218611,24.1222374444761));
#25788=CARTESIAN_POINT('Ctrl Pts',(-8.93568263873,-1.15585528366082,24.1540521267794));
#25789=CARTESIAN_POINT('Ctrl Pts',(-8.12471920819932,-1.25608488916436,
24.1858668090826));
#25790=CARTESIAN_POINT('Ctrl Pts',(-7.22379260339601,-0.589635437619165,
24.2256351619617));
#25791=CARTESIAN_POINT('Ctrl Pts',(-7.31492958877942,0.756088555050138,
24.2733571854165));
#25792=CARTESIAN_POINT('Ctrl Pts',(-8.49458917842518,1.40470690131819,24.3210792088714));
#25793=CARTESIAN_POINT('Ctrl Pts',(-9.67921054321693,0.765195581138799,
24.3688012323263));
#25794=CARTESIAN_POINT('Ctrl Pts',(-9.78071191837591,-0.579786383569809,
24.4165232557811));
#25795=CARTESIAN_POINT('Ctrl Pts',(-8.88494619440142,-1.25315655402566,
24.4562916086602));
#25796=CARTESIAN_POINT('Ctrl Pts',(-8.07323468672448,-1.15917736599807,
24.4881062909634));
#25797=CARTESIAN_POINT('Ctrl Pts',(-7.39436278074097,-0.704380054282347,
24.5199209732667));
#25798=CARTESIAN_POINT('Ctrl Pts',(-7.14907787678811,0.389081849306566,
24.5596893261457));
#25799=CARTESIAN_POINT('Ctrl Pts',(-8.09847937545032,1.34716107822693,24.6074113496006));
#25800=CARTESIAN_POINT('Ctrl Pts',(-9.41497817327985,1.06585444504516,24.6551333730554));
#25801=CARTESIAN_POINT('Ctrl Pts',(-9.89243323319677,-0.19285091059547,
24.7028553965103));
#25802=CARTESIAN_POINT('Ctrl Pts',(-9.0892006276166,-1.27640819836731,24.7505774199652));
#25803=CARTESIAN_POINT('Ctrl Pts',(-7.97120291139482,-1.19956598841592,
24.7903457728442));
#25804=CARTESIAN_POINT('Ctrl Pts',(-7.41883199075804,-0.597408180601113,
24.8221604551474));
#25805=CARTESIAN_POINT('Ctrl Pts',(-7.20299715504592,0.190705379217913,
24.8539751374507));
#25806=CARTESIAN_POINT('Ctrl Pts',(-7.73292871366386,1.17812431861909,24.8937434903297));
#25807=CARTESIAN_POINT('Ctrl Pts',(-9.07776780005844,1.28150152237285,24.9414655137846));
#25808=CARTESIAN_POINT('Ctrl Pts',(-9.88932138510403,0.207405025237497,
24.9891875372394));
#25809=CARTESIAN_POINT('Ctrl Pts',(-9.42685396925393,-1.0568838641528,25.0369095606943));
#25810=CARTESIAN_POINT('Ctrl Pts',(-8.11045794382281,-1.35078949318993,
25.0846315841492));
#25811=CARTESIAN_POINT('Ctrl Pts',(-7.31524469729938,-0.561194969867331,
25.1243999370282));
#25812=CARTESIAN_POINT('Ctrl Pts',(-7.29149151917362,0.255593525403265,
25.1562146193315));
#25813=CARTESIAN_POINT('Ctrl Pts',(-7.64391180276608,0.992823206839166,
25.1880293016347));
#25814=CARTESIAN_POINT('Ctrl Pts',(-8.69072170844657,1.39283900662292,25.2277976545138));
#25815=CARTESIAN_POINT('Ctrl Pts',(-9.77539825914043,0.59111848491638,25.2755196779686));
#25816=CARTESIAN_POINT('Ctrl Pts',(-9.68637964828473,-0.752152966980069,
25.3232417014235));
#25817=CARTESIAN_POINT('Ctrl Pts',(-8.50943955061137,-1.40569295278612,
25.3709637248783));
#25818=CARTESIAN_POINT('Ctrl Pts',(-7.32161442543538,-0.76666988078383,
25.4186857483332));
#25819=CARTESIAN_POINT('Ctrl Pts',(-7.23684682521555,0.350754869550781,
25.4584541012123));
#25820=CARTESIAN_POINT('Ctrl Pts',(-7.75329090619035,0.983995085190644,
25.4902687835155));
#25821=CARTESIAN_POINT('Ctrl Pts',(-8.50216376128743,1.31094631454484,25.5220834658187));
#25822=CARTESIAN_POINT('Ctrl Pts',(-9.55553913695975,0.928553928853571,
25.5618518186978));
#25823=CARTESIAN_POINT('Ctrl Pts',(-9.85128053691354,-0.387430888271607,
25.6095738421527));
#25824=CARTESIAN_POINT('Ctrl Pts',(-8.90508571176895,-1.34504138290304,
25.6572958656075));
#25825=CARTESIAN_POINT('Ctrl Pts',(-7.58742341373451,-1.06923606225583,
25.7050178890624));
#25826=CARTESIAN_POINT('Ctrl Pts',(-7.10722604889511,0.191196206988292,
25.7527399125173));
#25827=CARTESIAN_POINT('Ctrl Pts',(-7.77422773713762,1.09171403945412,25.7925082653963));
#25828=CARTESIAN_POINT('Ctrl Pts',(-8.57910601748431,1.23270557573783,25.8243229476995));
#25829=CARTESIAN_POINT('Ctrl Pts',(-9.35936090055085,0.989991800009503,
25.8561376300028));
#25830=CARTESIAN_POINT('Ctrl Pts',(-9.90578824612508,0.0116049773692086,
25.8959059828818));
#25831=CARTESIAN_POINT('Ctrl Pts',(-9.26842252690367,-1.17711027638675,
25.9436280063367));
#25832=CARTESIAN_POINT('Ctrl Pts',(-7.92631518097252,-1.2822310571884,25.9913500297916));
#25833=CARTESIAN_POINT('Ctrl Pts',(-7.11028230216784,-0.211533692258238,
26.0390720532464));
#25834=CARTESIAN_POINT('Ctrl Pts',(-7.57180572399499,1.05585541360293,26.0867940767013));
#25835=CARTESIAN_POINT('Ctrl Pts',(-8.66541780729333,1.30046986528404,26.1265624295803));
#25836=CARTESIAN_POINT('Ctrl Pts',(-9.36635747060411,0.880480284609375,
26.1583771118836));
#25837=CARTESIAN_POINT('Ctrl Pts',(-9.79762530788041,0.186422857584386,
26.1901917941868));
#25838=CARTESIAN_POINT('Ctrl Pts',(-9.57072492125683,-0.9110013235131,26.2299601470659));
#25839=CARTESIAN_POINT('Ctrl Pts',(-8.31096363818387,-1.39295622204707,
26.2776821705207));
#25840=CARTESIAN_POINT('Ctrl Pts',(-7.22721218956511,-0.594341606493663,
26.3254041939756));
#25841=CARTESIAN_POINT('Ctrl Pts',(-7.31061933906771,0.749289947903038,
26.3731262174305));
#25842=CARTESIAN_POINT('Ctrl Pts',(-8.48887394443472,1.4057921181066,26.4208482408854));
#25843=CARTESIAN_POINT('Ctrl Pts',(-9.47596779494645,0.875255268312624,
26.4606165937644));
#25844=CARTESIAN_POINT('Ctrl Pts',(-9.73126541035378,0.0990267020740463,
26.4924312760676));
#25845=CARTESIAN_POINT('Ctrl Pts',(-9.60330599525195,-0.70802598986389,
26.5242459583709));
#25846=CARTESIAN_POINT('Ctrl Pts',(-8.71369030804601,-1.38950052921557,
26.5640143112499));
#25847=CARTESIAN_POINT('Ctrl Pts',(-7.44565872044378,-0.929745260193386,
26.6117363347048));
#25848=CARTESIAN_POINT('Ctrl Pts',(-7.14858480305884,0.383285430296478,
26.6594583581596));
#25849=CARTESIAN_POINT('Ctrl Pts',(-8.09077154939971,1.3448397145562,26.7071803816145));
#25850=CARTESIAN_POINT('Ctrl Pts',(-9.41136604307352,1.07041450101146,26.7549024050693));
#25851=CARTESIAN_POINT('Ctrl Pts',(-9.81073996404354,0.0233595406792121,
26.7946707579485));
#25852=CARTESIAN_POINT('Ctrl Pts',(-9.49593963948833,-0.730701740078134,
26.8264854402517));
#25853=CARTESIAN_POINT('Ctrl Pts',(-8.87113233708174,-1.25731686931094,
26.8583001225549));
#25854=CARTESIAN_POINT('Ctrl Pts',(-7.75248308879724,-1.19062745470989,
26.898068475434));
#25855=CARTESIAN_POINT('Ctrl Pts',(-7.09433817452238,-0.0132896585083106,
26.9457904988888));
#25856=CARTESIAN_POINT('Ctrl Pts',(-7.72876335020465,1.17406336524635,26.9935125223437));
#25857=CARTESIAN_POINT('Ctrl Pts',(-9.07041991168043,1.28478905155158,27.0412345457985));
#25858=CARTESIAN_POINT('Ctrl Pts',(-9.88957324816892,0.213216923381752,
27.0889565692534));
#25859=CARTESIAN_POINT('Ctrl Pts',(-9.50653510539861,-0.839923807902734,
27.1287249221325));
#25860=CARTESIAN_POINT('Ctrl Pts',(-8.7750999084873,-1.20421793659106,27.1605396044357));
#25861=CARTESIAN_POINT('Ctrl Pts',(-7.9580341293038,-1.19367412491104,27.192354286739));
#25862=CARTESIAN_POINT('Ctrl Pts',(-7.15568539944002,-0.411331403085548,
27.232122639618));
#25863=CARTESIAN_POINT('Ctrl Pts',(-7.42826843340841,0.909644563441927,
27.2798446630729));
#25864=CARTESIAN_POINT('Ctrl Pts',(-8.68491464228127,1.39249320668759,27.3275666865277));
#25865=CARTESIAN_POINT('Ctrl Pts',(-9.77199235522125,0.598412258302711,
27.3752887099826));
#25866=CARTESIAN_POINT('Ctrl Pts',(-9.69037272304938,-0.747922488405797,
27.4230107334374));
#25867=CARTESIAN_POINT('Ctrl Pts',(-8.71165106735223,-1.29374987813343,
27.4627790863165));
#25868=CARTESIAN_POINT('Ctrl Pts',(-7.92015079905928,-1.09068588632374,
27.4945937686197));
#25869=CARTESIAN_POINT('Ctrl Pts',(-7.30914068425147,-0.548123171902564,
27.526408450923));
#25870=CARTESIAN_POINT('Ctrl Pts',(-7.21423215015474,0.56848597585817,27.5661768038021));
#25871=CARTESIAN_POINT('Ctrl Pts',(-8.2846607135526,1.3891331017367,27.6138988272568));
#25872=CARTESIAN_POINT('Ctrl Pts',(-9.55092127427873,0.932091857527698,
27.6616208507118));
#25873=CARTESIAN_POINT('Ctrl Pts',(-9.85347697299502,-0.379686536764967,
27.7093428741665));
#25874=CARTESIAN_POINT('Ctrl Pts',(-8.91087340080395,-1.34445465410882,
27.7570648976215));
#25875=CARTESIAN_POINT('Ctrl Pts',(-7.81358853956333,-1.11688147467079,
27.7968332505005));
#25876=CARTESIAN_POINT('Ctrl Pts',(-7.34787432426479,-0.445451709806008,
27.8286479328038));
#25877=CARTESIAN_POINT('Ctrl Pts',(-7.24078324703436,0.364634187278428,
27.860462615107));
#25878=CARTESIAN_POINT('Ctrl Pts',(-7.89958218878159,1.27117021693195,27.9002309679861));
#25879=CARTESIAN_POINT('Ctrl Pts',(-9.2460294657544,1.19142847827918,27.9479529914409));
#25880=CARTESIAN_POINT('Ctrl Pts',(-9.90461076431774,0.0173019179198019,
27.9956750148958));
#25881=CARTESIAN_POINT('Ctrl Pts',(-9.27515055498282,-1.17269066668845,
28.0433970383506));
#25882=CARTESIAN_POINT('Ctrl Pts',(-7.93107602430974,-1.28557410456496,
28.0911190618055));
#25883=CARTESIAN_POINT('Ctrl Pts',(-7.25014704022386,-0.395540769605531,
28.1308874146846));
#25884=CARTESIAN_POINT('Ctrl Pts',(-7.3372514650321,0.416937216961606,28.1627020969878));
#25885=CARTESIAN_POINT('Ctrl Pts',(-7.78628561432887,1.09963480172617,28.1945167792911));
#25886=CARTESIAN_POINT('Ctrl Pts',(-8.87763192295398,1.35416741919462,28.2342851321701));
#25887=CARTESIAN_POINT('Ctrl Pts',(-9.84371380784354,0.412910384032882,
28.2820071556249));
#25888=CARTESIAN_POINT('Ctrl Pts',(-9.57356183488256,-0.905922591770999,
28.3297291790799));
#25889=CARTESIAN_POINT('Ctrl Pts',(-8.3189433892574,-1.39401588453317,28.3774512025346));
#25890=CARTESIAN_POINT('Ctrl Pts',(-7.22862530768708,-0.599984716648168,
28.4251732259896));
#25891=CARTESIAN_POINT('Ctrl Pts',(-7.29600055841505,0.518623433827608,
28.4649415788686));
#25892=CARTESIAN_POINT('Ctrl Pts',(-7.89346079467198,1.07607201936972,28.4967562611719));
#25893=CARTESIAN_POINT('Ctrl Pts',(-8.67971900484753,1.29857075310551,28.5285709434751));
#25894=CARTESIAN_POINT('Ctrl Pts',(-9.67158860247685,0.777016997712584,
28.5683392963541));
#25895=CARTESIAN_POINT('Ctrl Pts',(-9.78634659247671,-0.56689878022201,
28.616061319809));
#25896=CARTESIAN_POINT('Ctrl Pts',(-8.71915864026611,-1.38751585434476,
28.6637833432638));
#25897=CARTESIAN_POINT('Ctrl Pts',(-7.45100011939933,-0.935767616313009,
28.7115053667187));
#25898=CARTESIAN_POINT('Ctrl Pts',(-7.14596130919067,0.378093235837449,
28.7592273901736));
#25899=CARTESIAN_POINT('Ctrl Pts',(-7.92879581040033,1.17996215792724,28.7989957430527));
#25900=CARTESIAN_POINT('Ctrl Pts',(-8.74535395632626,1.21062885803138,28.8308104253558));
#25901=CARTESIAN_POINT('Ctrl Pts',(-9.48554058013625,0.864462087680875,
28.8626251076592));
#25902=CARTESIAN_POINT('Ctrl Pts',(-9.89440360594169,-0.17892405294294,
28.9023934605382));
#25903=CARTESIAN_POINT('Ctrl Pts',(-9.10189397776309,-1.27034854886995,
28.950115483993));
#25904=CARTESIAN_POINT('Ctrl Pts',(-7.75791702419191,-1.19270436179798,
28.9978375074479));
#25905=CARTESIAN_POINT('Ctrl Pts',(-7.09443740014052,-0.0213388321030302,
29.0455595309027));
#25906=CARTESIAN_POINT('Ctrl Pts',(-7.72338203077529,1.1718532119868,29.0932815543577));
#25907=CARTESIAN_POINT('Ctrl Pts',(-8.84004957245219,1.26607722708656,29.1330499072366));
#25908=CARTESIAN_POINT('Ctrl Pts',(-9.47763834518235,0.755012087082805,
29.1648645895399));
#25909=CARTESIAN_POINT('Ctrl Pts',(-9.81091851614448,0.00893409317460413,
29.1966792718431));
#25910=CARTESIAN_POINT('Ctrl Pts',(-9.43745431001592,-1.04764123587576,
29.2364476247222));
#25911=CARTESIAN_POINT('Ctrl Pts',(-8.12402506966911,-1.35451113192694,
29.2841696481771));
#25912=CARTESIAN_POINT('Ctrl Pts',(-7.15843040209203,-0.416458701888962,
29.3318916716319));
#25913=CARTESIAN_POINT('Ctrl Pts',(-7.42308757914243,0.903494929509393,
29.3796136950868));
#25914=CARTESIAN_POINT('Ctrl Pts',(-8.67937808940375,1.39433769122377,29.4273357185416));
#25915=CARTESIAN_POINT('Ctrl Pts',(-9.58556770780354,0.734996509965079,
29.4671040714208));
#25916=CARTESIAN_POINT('Ctrl Pts',(-9.73328209692014,-0.0686793482256725,
29.4989187537239));
#25917=CARTESIAN_POINT('Ctrl Pts',(-9.49735030797155,-0.850921733780152,
29.5307334360272));
#25918=CARTESIAN_POINT('Ctrl Pts',(-8.52325181788503,-1.40569864308938,
29.5705017889063));
#25919=CARTESIAN_POINT('Ctrl Pts',(-7.32986179028487,-0.778260502859741,
29.6182238123611));
#25920=CARTESIAN_POINT('Ctrl Pts',(-7.21218073812471,0.56262788812223,29.665945835816));
#25921=CARTESIAN_POINT('Ctrl Pts',(-8.27818752900583,1.38822684395199,29.7136678592708));
#25922=CARTESIAN_POINT('Ctrl Pts',(-9.33384484159048,1.01168221201436,29.7534362121499));
#25923=CARTESIAN_POINT('Ctrl Pts',(-9.70261207523359,0.282249903129775,
29.7852508944531));
#25924=CARTESIAN_POINT('Ctrl Pts',(-9.69665295292861,-0.534421386281917,
29.8170655767564));
#25925=CARTESIAN_POINT('Ctrl Pts',(-8.92010172213024,-1.34249070178533,
29.8568339296354));
#25926=CARTESIAN_POINT('Ctrl Pts',(-7.5957088359255,-1.076002984984,29.9045559530903));
#25927=CARTESIAN_POINT('Ctrl Pts',(-7.18991001744901,-0.0344549071388059,
29.9443243059693));
#25928=CARTESIAN_POINT('Ctrl Pts',(-7.49844573549237,0.725568290707585,
29.9761389882726));
#25929=CARTESIAN_POINT('Ctrl Pts',(-7.80953045183888,0.987070987050173,
29.9920463294242));
#25930=CARTESIAN_POINT('Ctrl Pts',(-7.9881611888325,1.07233375495115,30.));
#25931=CARTESIAN_POINT('Ctrl Pts',(-7.84336223800221,-0.920831852263776,
1.73389339417779));
#25932=CARTESIAN_POINT('Ctrl Pts',(-7.68996888294128,-0.811448288777214,
1.7418470647536));
#25933=CARTESIAN_POINT('Ctrl Pts',(-7.44147150789439,-0.515011305712358,
1.75775440590522));
#25934=CARTESIAN_POINT('Ctrl Pts',(-7.27756915484984,0.248331434474109,
1.78956908820846));
#25935=CARTESIAN_POINT('Ctrl Pts',(-7.82972574274999,1.15778987946338,1.82933744108751));
#25936=CARTESIAN_POINT('Ctrl Pts',(-9.11518963502401,1.1892113537284,1.87705946454237));
#25937=CARTESIAN_POINT('Ctrl Pts',(-9.70989914651746,0.303653650183944,
1.91682781742143));
#25938=CARTESIAN_POINT('Ctrl Pts',(-9.58081711606472,-0.462897910902464,
1.94864249972467));
#25939=CARTESIAN_POINT('Ctrl Pts',(-9.1148424724598,-1.08587738685965,1.98045718202791));
#25940=CARTESIAN_POINT('Ctrl Pts',(-8.06315002296502,-1.26478329921431,
2.02022553490696));
#25941=CARTESIAN_POINT('Ctrl Pts',(-7.19998796076663,-0.315061926834089,
2.06794755836182));
#25942=CARTESIAN_POINT('Ctrl Pts',(-7.53141637453974,0.922516240590291,
2.11566958181669));
#25943=CARTESIAN_POINT('Ctrl Pts',(-8.7535951383005,1.31390426831436,2.16339160527155));
#25944=CARTESIAN_POINT('Ctrl Pts',(-9.57525824943383,0.633214111788618,
2.2031599581506));
#25945=CARTESIAN_POINT('Ctrl Pts',(-9.66743586945616,-0.138985158650247,
2.23497464045384));
#25946=CARTESIAN_POINT('Ctrl Pts',(-9.39643922585092,-0.868013858452754,
2.26678932275708));
#25947=CARTESIAN_POINT('Ctrl Pts',(-8.43822881651588,-1.33666768258406,
2.30655767563613));
#25948=CARTESIAN_POINT('Ctrl Pts',(-7.3414888899664,-0.669377881206568,
2.354279699091));
#25949=CARTESIAN_POINT('Ctrl Pts',(-7.31105138266357,0.611622684002372,
2.40200172254586));
#25950=CARTESIAN_POINT('Ctrl Pts',(-8.37090883221922,1.33175184955348,2.44972374600072));
#25951=CARTESIAN_POINT('Ctrl Pts',(-9.55154902931157,0.827500878887315,
2.49744576945558));
#25952=CARTESIAN_POINT('Ctrl Pts',(-9.72741589040921,-0.224544184030281,
2.53721412233464));
#25953=CARTESIAN_POINT('Ctrl Pts',(-9.29196288579558,-0.868979538690168,
2.56902880463787));
#25954=CARTESIAN_POINT('Ctrl Pts',(-8.60999646405335,-1.24292755198912,
2.60084348694112));
#25955=CARTESIAN_POINT('Ctrl Pts',(-7.57874071102671,-0.97046216532521,
2.64061183982017));
#25956=CARTESIAN_POINT('Ctrl Pts',(-7.18590781273401,0.251779422282229,
2.68833386327503));
#25957=CARTESIAN_POINT('Ctrl Pts',(-8.00102785596058,1.24044081982532,2.7360558867299));
#25958=CARTESIAN_POINT('Ctrl Pts',(-9.27371025598029,1.09160606477469,2.78377791018476));
#25959=CARTESIAN_POINT('Ctrl Pts',(-9.83665460260352,-0.0622076783418028,
2.83149993363962));
#25960=CARTESIAN_POINT('Ctrl Pts',(-9.28132245236828,-0.972883886508404,
2.87126828651867));
#25961=CARTESIAN_POINT('Ctrl Pts',(-8.53036971029236,-1.1753335976729,2.90308296882191));
#25962=CARTESIAN_POINT('Ctrl Pts',(-7.76996377379206,-1.01193622592224,
2.93489765112516));
#25963=CARTESIAN_POINT('Ctrl Pts',(-7.16834172261016,-0.131154827519332,
2.97466600400421));
#25964=CARTESIAN_POINT('Ctrl Pts',(-7.67094735813036,1.05019191790059,3.02238802745907));
#25965=CARTESIAN_POINT('Ctrl Pts',(-8.93424496562127,1.26455441305742,3.07011005091393));
#25966=CARTESIAN_POINT('Ctrl Pts',(-9.79933578640807,0.319308413861016,
3.11783207436879));
#25967=CARTESIAN_POINT('Ctrl Pts',(-9.4701483140956,-0.921589714816724,
3.16555409782365));
#25968=CARTESIAN_POINT('Ctrl Pts',(-8.45434027041126,-1.24694948055712,
3.20532245070271));
#25969=CARTESIAN_POINT('Ctrl Pts',(-7.75397118940257,-0.908720199684656,
3.23713713300595));
#25970=CARTESIAN_POINT('Ctrl Pts',(-7.28581913026257,-0.287632810134478,
3.26895181530919));
#25971=CARTESIAN_POINT('Ctrl Pts',(-7.40711716645252,0.772089674964555,
3.30872016818824));
#25972=CARTESIAN_POINT('Ctrl Pts',(-8.56014462832698,1.33664279908732,3.35644219164311));
#25973=CARTESIAN_POINT('Ctrl Pts',(-9.65577050263654,0.672206143179195,
3.40416421509796));
#25974=CARTESIAN_POINT('Ctrl Pts',(-9.6915437695127,-0.608649976596257,
3.45188623855283));
#25975=CARTESIAN_POINT('Ctrl Pts',(-8.63070115364378,-1.33170288070012,
3.49960826200769));
#25976=CARTESIAN_POINT('Ctrl Pts',(-7.64961690888714,-0.913135486265902,
3.53937661488675));
#25977=CARTESIAN_POINT('Ctrl Pts',(-7.34125675698761,-0.199111738272663,
3.57119129718998));
#25978=CARTESIAN_POINT('Ctrl Pts',(-7.39357959894616,0.576889689681292,
3.60300597949323));
#25979=CARTESIAN_POINT('Ctrl Pts',(-8.17866573276028,1.29894558882475,3.64277433237228));
#25980=CARTESIAN_POINT('Ctrl Pts',(-9.42002179212659,0.971489192263309,
3.69049635582714));
#25981=CARTESIAN_POINT('Ctrl Pts',(-9.81386559492375,-0.247838157214267,
3.738218379282));
#25982=CARTESIAN_POINT('Ctrl Pts',(-9.00288207825834,-1.23989554561616,
3.78594040273686));
#25983=CARTESIAN_POINT('Ctrl Pts',(-7.72753804870358,-1.09261973615206,
3.83366242619173));
#25984=CARTESIAN_POINT('Ctrl Pts',(-7.25944965685775,-0.13417400664288,
3.87343077907078));
#25985=CARTESIAN_POINT('Ctrl Pts',(-7.49342196021817,0.607562373237147,
3.90524546137402));
#25986=CARTESIAN_POINT('Ctrl Pts',(-8.04071266532901,1.16018229694294,3.93706014367726));
#25987=CARTESIAN_POINT('Ctrl Pts',(-9.10686262033383,1.19257415453766,3.97682849655631));
#25988=CARTESIAN_POINT('Ctrl Pts',(-9.83139444220645,0.13274105594708,4.02455052001118));
#25989=CARTESIAN_POINT('Ctrl Pts',(-9.33145993517061,-1.04706300187806,
4.07227254346604));
#25990=CARTESIAN_POINT('Ctrl Pts',(-8.06906871353424,-1.26670027039436,
4.1199945669209));
#25991=CARTESIAN_POINT('Ctrl Pts',(-7.20094501503803,-0.32089172640491,
4.16771659037576));
#25992=CARTESIAN_POINT('Ctrl Pts',(-7.47404245851617,0.710196410158088,
4.20748494325482));
#25993=CARTESIAN_POINT('Ctrl Pts',(-8.13628727307677,1.11805386266434,4.23929962555805));
#25994=CARTESIAN_POINT('Ctrl Pts',(-8.91174525720005,1.17789373930854,4.2711143078613));
#25995=CARTESIAN_POINT('Ctrl Pts',(-9.73921801071789,0.504830739894083,
4.31088266074035));
#25996=CARTESIAN_POINT('Ctrl Pts',(-9.59372114360799,-0.770717463599363,
4.35860468419521));
#25997=CARTESIAN_POINT('Ctrl Pts',(-8.44372307881386,-1.33585158675566,
4.40632670765008));
#25998=CARTESIAN_POINT('Ctrl Pts',(-7.34533148911299,-0.675997025613394,
4.45404873110494));
#25999=CARTESIAN_POINT('Ctrl Pts',(-7.3076326594131,0.607268868896949,4.5017707545598));
#26000=CARTESIAN_POINT('Ctrl Pts',(-8.18878274818164,1.20835079347829,4.54153910743885));
#26001=CARTESIAN_POINT('Ctrl Pts',(-8.95646012486506,1.08350151912803,4.57335378974209));
#26002=CARTESIAN_POINT('Ctrl Pts',(-9.58205477061933,0.621389806248012,
4.60516847204534));
#26003=CARTESIAN_POINT('Ctrl Pts',(-9.76746285062318,-0.429014307826431,
4.64493682492438));
#26004=CARTESIAN_POINT('Ctrl Pts',(-8.82286605099045,-1.2984563380376,4.69265884837925));
#26005=CARTESIAN_POINT('Ctrl Pts',(-7.5834208477958,-0.973421394587389,
4.7403808718341));
#26006=CARTESIAN_POINT('Ctrl Pts',(-7.18448749550299,0.244250279803643,
4.78810289528898));
#26007=CARTESIAN_POINT('Ctrl Pts',(-7.99559146371714,1.2393899235328,4.83582491874383));
#26008=CARTESIAN_POINT('Ctrl Pts',(-9.05523938128985,1.11744218973236,4.87559327162289));
#26009=CARTESIAN_POINT('Ctrl Pts',(-9.55411169716992,0.520749380637289,
4.90740795392613));
#26010=CARTESIAN_POINT('Ctrl Pts',(-9.72486976937421,-0.238037530658888,
4.93922263622937));
#26011=CARTESIAN_POINT('Ctrl Pts',(-9.17782796817209,-1.15371772959998,
4.97899098910842));
#26012=CARTESIAN_POINT('Ctrl Pts',(-7.8946159026944,-1.19320637083518,5.02671301256328));
#26013=CARTESIAN_POINT('Ctrl Pts',(-7.16994486640164,-0.136454737127305,
5.07443503601815));
#26014=CARTESIAN_POINT('Ctrl Pts',(-7.66494711141124,1.0454271959021,5.12215705947301));
#26015=CARTESIAN_POINT('Ctrl Pts',(-8.92944607964153,1.26731662133429,5.16987908292787));
#26016=CARTESIAN_POINT('Ctrl Pts',(-9.65102050340854,0.481787939515094,
5.20964743580693));
#26017=CARTESIAN_POINT('Ctrl Pts',(-9.63789081754475,-0.295864622575736,
5.24146211811016));
#26018=CARTESIAN_POINT('Ctrl Pts',(-9.27056889001754,-0.981423152195916,
5.27327680041342));
#26019=CARTESIAN_POINT('Ctrl Pts',(-8.25775645274699,-1.3159914201255,5.31304515329245));
#26020=CARTESIAN_POINT('Ctrl Pts',(-7.26148648143051,-0.506276222029801,
5.36076717674732));
#26021=CARTESIAN_POINT('Ctrl Pts',(-7.40486192963386,0.767032698475483,
5.40848920020218));
#26022=CARTESIAN_POINT('Ctrl Pts',(-8.55248946485333,1.33696529676413,5.45621122365705));
#26023=CARTESIAN_POINT('Ctrl Pts',(-9.65394858372652,0.677434882586624,
5.5039332471119));
#26024=CARTESIAN_POINT('Ctrl Pts',(-9.68568677413502,-0.388734731623442,
5.54370159999096));
#26025=CARTESIAN_POINT('Ctrl Pts',(-9.16695572119068,-0.968246587143773,
5.5755162822942));
#26026=CARTESIAN_POINT('Ctrl Pts',(-8.44062079418711,-1.24637150474729,
5.60733096459744));
#26027=CARTESIAN_POINT('Ctrl Pts',(-7.4557770578489,-0.836728032944395,
5.6470993174765));
#26028=CARTESIAN_POINT('Ctrl Pts',(-7.23212417540165,0.427460222794115,
5.69482134093136));
#26029=CARTESIAN_POINT('Ctrl Pts',(-8.17365152926984,1.29659678749714,5.74254336438622));
#26030=CARTESIAN_POINT('Ctrl Pts',(-9.41444355276615,0.976741694347395,
5.79026538784108));
#26031=CARTESIAN_POINT('Ctrl Pts',(-9.81590881670993,-0.242691862522644,
5.83798741129594));
#26032=CARTESIAN_POINT('Ctrl Pts',(-9.14233861671162,-1.06975180271407,
5.877755764175));
#26033=CARTESIAN_POINT('Ctrl Pts',(-8.37088414006259,-1.16861477068245,
5.90957044647823));
#26034=CARTESIAN_POINT('Ctrl Pts',(-7.63961966684838,-0.903722025987471,
5.94138512878148));
#26035=CARTESIAN_POINT('Ctrl Pts',(-7.16284941248119,0.0504347135191421,
5.98115348166053));
#26036=CARTESIAN_POINT('Ctrl Pts',(-7.82084291379945,1.15281264780352,6.02887550511539));
#26037=CARTESIAN_POINT('Ctrl Pts',(-9.10153384108041,1.19407855341718,6.07659752857025));
#26038=CARTESIAN_POINT('Ctrl Pts',(-9.83061248159845,0.140363002556222,
6.12431955202512));
#26039=CARTESIAN_POINT('Ctrl Pts',(-9.3363722406032,-1.04450793638824,6.17204157547998));
#26040=CARTESIAN_POINT('Ctrl Pts',(-8.28585464946359,-1.2292719742891,6.21180992835902));
#26041=CARTESIAN_POINT('Ctrl Pts',(-7.6377556831852,-0.799291014377838,
6.24362461066228));
#26042=CARTESIAN_POINT('Ctrl Pts',(-7.25804823806631,-0.120514061249209,
6.2754392929655));
#26043=CARTESIAN_POINT('Ctrl Pts',(-7.5217737984046,0.913010872083068,6.31520764584457));
#26044=CARTESIAN_POINT('Ctrl Pts',(-8.74064622138336,1.31617656292995,6.36292966929942));
#26045=CARTESIAN_POINT('Ctrl Pts',(-9.73617240019874,0.509454954517775,
6.4106516927543));
#26046=CARTESIAN_POINT('Ctrl Pts',(-9.59811666235571,-0.764441720819152,
6.45837371620915));
#26047=CARTESIAN_POINT('Ctrl Pts',(-8.44910975161753,-1.33713332792554,
6.50609573966402));
#26048=CARTESIAN_POINT('Ctrl Pts',(-7.53376511844561,-0.78953022209195,
6.54586409254306));
#26049=CARTESIAN_POINT('Ctrl Pts',(-7.32496560452136,-0.0403181967197514,
6.57767877484631));
#26050=CARTESIAN_POINT('Ctrl Pts',(-7.48192004532567,0.721443708004499,
6.60949345714955));
#26051=CARTESIAN_POINT('Ctrl Pts',(-8.3575769611271,1.33050029388492,6.6492618100286));
#26052=CARTESIAN_POINT('Ctrl Pts',(-9.54313609419374,0.83791314446213,6.69698383348346));
#26053=CARTESIAN_POINT('Ctrl Pts',(-9.76818512374022,-0.423524551377841,
6.74470585693832));
#26054=CARTESIAN_POINT('Ctrl Pts',(-8.83029626289538,-1.29658618201396,
6.79242788039319));
#26055=CARTESIAN_POINT('Ctrl Pts',(-7.58665592075209,-0.977915102108791,
6.84014990384804));
#26056=CARTESIAN_POINT('Ctrl Pts',(-7.25270867534208,0.0351022700415088,
6.8799182567271));
#26057=CARTESIAN_POINT('Ctrl Pts',(-7.58499699015572,0.738309474082838,
6.91173293903034));
#26058=CARTESIAN_POINT('Ctrl Pts',(-8.20209906933813,1.21170246077153,6.94354762133359));
#26059=CARTESIAN_POINT('Ctrl Pts',(-9.26281040945734,1.09937965837702,6.98331597421263));
#26060=CARTESIAN_POINT('Ctrl Pts',(-9.83710404863512,-0.0488273672825927,
7.0310379976675));
#26061=CARTESIAN_POINT('Ctrl Pts',(-9.18196602157746,-1.15003865113727,
7.07876002112236));
#26062=CARTESIAN_POINT('Ctrl Pts',(-7.90145862879751,-1.19665349020977,
7.12648204457722));
#26063=CARTESIAN_POINT('Ctrl Pts',(-7.16945126292874,-0.141969758426622,
7.17420406803208));
#26064=CARTESIAN_POINT('Ctrl Pts',(-7.57969846964756,0.842622638646724,
7.21397242091114));
#26065=CARTESIAN_POINT('Ctrl Pts',(-8.2910862664808,1.15701617944247,7.24578710321438));
#26066=CARTESIAN_POINT('Ctrl Pts',(-9.06750281866429,1.11126431092565,7.27760178551762));
#26067=CARTESIAN_POINT('Ctrl Pts',(-9.79617884906223,0.332318740478792,
7.31737013839667));
#26068=CARTESIAN_POINT('Ctrl Pts',(-9.47924265918208,-0.911764861743525,
7.36509216185153));
#26069=CARTESIAN_POINT('Ctrl Pts',(-8.2632930128867,-1.31591654596617,7.4128141853064));
#26070=CARTESIAN_POINT('Ctrl Pts',(-7.26440593819962,-0.513360169000101,
7.46053620876126));
#26071=CARTESIAN_POINT('Ctrl Pts',(-7.40088027814676,0.763184899655971,
7.50825823221612));
#26072=CARTESIAN_POINT('Ctrl Pts',(-8.35532914820361,1.23937006683617,7.54802658509517));
#26073=CARTESIAN_POINT('Ctrl Pts',(-9.09901960048363,1.01168518116112,7.57984126739841));
#26074=CARTESIAN_POINT('Ctrl Pts',(-9.65625271272335,0.469092189498902,
7.61165594970165));
#26075=CARTESIAN_POINT('Ctrl Pts',(-9.69766870777694,-0.59674535644745,
7.65142430258072));
#26076=CARTESIAN_POINT('Ctrl Pts',(-8.64400697660681,-1.33022304120803,
7.69914632603556));
#26077=CARTESIAN_POINT('Ctrl Pts',(-7.46001308842361,-0.840293863743886,
7.74686834949043));
#26078=CARTESIAN_POINT('Ctrl Pts',(-7.22969714705018,0.420192825331074,
7.7945903729453));
#26079=CARTESIAN_POINT('Ctrl Pts',(-8.16812285842602,1.2962919875284,7.84231239640014));
#26080=CARTESIAN_POINT('Ctrl Pts',(-9.20148590623969,1.03193281819899,7.88208074927922));
#26081=CARTESIAN_POINT('Ctrl Pts',(-9.61493485738788,0.373164375746146,
7.91389543158245));
#26082=CARTESIAN_POINT('Ctrl Pts',(-9.68133708809676,-0.4017592590297,7.94571011388569));
#26083=CARTESIAN_POINT('Ctrl Pts',(-9.0153030252643,-1.23490005513933,7.98547846676475));
#26084=CARTESIAN_POINT('Ctrl Pts',(-7.73856884929759,-1.10020632220151,
8.0332004902196));
#26085=CARTESIAN_POINT('Ctrl Pts',(-7.16371987671753,0.0449664965946314,
8.08092251367447));
#26086=CARTESIAN_POINT('Ctrl Pts',(-7.81425256053065,1.14890460784758,8.12864453712933));
#26087=CARTESIAN_POINT('Ctrl Pts',(-9.0971533411999,1.19746534025978,8.1763665605842));
#26088=CARTESIAN_POINT('Ctrl Pts',(-9.70567294360804,0.321435173838384,
8.21613491346324));
#26089=CARTESIAN_POINT('Ctrl Pts',(-9.58732677568735,-0.447271584630546,
8.2479495957665));
#26090=CARTESIAN_POINT('Ctrl Pts',(-9.1305274783773,-1.07675573689679,8.27976427806972));
#26091=CARTESIAN_POINT('Ctrl Pts',(-8.08173054010407,-1.27104917802106,
8.3195326309488));
#26092=CARTESIAN_POINT('Ctrl Pts',(-7.20432335123046,-0.333846327680171,
8.36725465440363));
#26093=CARTESIAN_POINT('Ctrl Pts',(-7.5188543507682,0.908305988469376,8.41497667785851));
#26094=CARTESIAN_POINT('Ctrl Pts',(-8.73310529664872,1.31753302400603,8.46269870131337));
#26095=CARTESIAN_POINT('Ctrl Pts',(-9.73507553588205,0.514882292077843,
8.51042072476822));
#26096=CARTESIAN_POINT('Ctrl Pts',(-9.62210242793819,-0.545759983091655,
8.55018907764729));
#26097=CARTESIAN_POINT('Ctrl Pts',(-9.02965411186355,-1.04966561786629,
8.58200375995052));
#26098=CARTESIAN_POINT('Ctrl Pts',(-8.27233991033248,-1.22684094384789,
8.61381844225377));
#26099=CARTESIAN_POINT('Ctrl Pts',(-7.35206163888205,-0.687570267757052,
8.65358679513281));
#26100=CARTESIAN_POINT('Ctrl Pts',(-7.30171161474597,0.595261534485032,
8.70130881858769));
#26101=CARTESIAN_POINT('Ctrl Pts',(-8.35229081295244,1.32885234309819,8.74903084204254));
#26102=CARTESIAN_POINT('Ctrl Pts',(-9.53832074872148,0.843872840804017,
8.79675286549741));
#26103=CARTESIAN_POINT('Ctrl Pts',(-9.77090660905737,-0.418702454117434,
8.84447488895226));
#26104=CARTESIAN_POINT('Ctrl Pts',(-8.99151443062067,-1.14690077270034,
8.88424324183132));
#26105=CARTESIAN_POINT('Ctrl Pts',(-8.21377858598168,-1.14035463330576,
8.91605792413455));
#26106=CARTESIAN_POINT('Ctrl Pts',(-7.52513512409165,-0.778849338222222,
8.94787260643781));
#26107=CARTESIAN_POINT('Ctrl Pts',(-7.18200506515434,0.23109458182923,8.98764095931685));
#26108=CARTESIAN_POINT('Ctrl Pts',(-7.98325750814354,1.23418335176835,9.03536298277172));
#26109=CARTESIAN_POINT('Ctrl Pts',(-9.2577345228738,1.10159200548163,9.08308500622657));
#26110=CARTESIAN_POINT('Ctrl Pts',(-9.8373617313639,-0.0411697480627666,
9.13080702968145));
#26111=CARTESIAN_POINT('Ctrl Pts',(-9.18717915050991,-1.14817253456704,
9.1785290531363));
#26112=CARTESIAN_POINT('Ctrl Pts',(-8.12131641256235,-1.1889350522776,9.21829740601535));
#26113=CARTESIAN_POINT('Ctrl Pts',(-7.53743409861438,-0.675128338195253,
9.25011208831859));
#26114=CARTESIAN_POINT('Ctrl Pts',(-7.25317049070035,0.0488261473858512,
9.28192677062183));
#26115=CARTESIAN_POINT('Ctrl Pts',(-7.6544622692538,1.03710235749143,9.3216951235009));
#26116=CARTESIAN_POINT('Ctrl Pts',(-8.91671193459285,1.27144898137521,9.36941714695573));
#26117=CARTESIAN_POINT('Ctrl Pts',(-9.7937876850699,0.337312880953606,9.41713917041064));
#26118=CARTESIAN_POINT('Ctrl Pts',(-9.48444775149291,-0.906142358160533,
9.46486119386546));
#26119=CARTESIAN_POINT('Ctrl Pts',(-8.26845641970075,-1.3179161295211,9.51258321732035));
#26120=CARTESIAN_POINT('Ctrl Pts',(-7.43572412851178,-0.651371389682554,
9.55235157019938));
#26121=CARTESIAN_POINT('Ctrl Pts',(-7.33033409569525,0.11921853820403,9.58416625250264));
#26122=CARTESIAN_POINT('Ctrl Pts',(-7.58902696279783,0.852699210401694,
9.61598093480587));
#26123=CARTESIAN_POINT('Ctrl Pts',(-8.53911350180821,1.33752962135646,9.65574928768493));
#26124=CARTESIAN_POINT('Ctrl Pts',(-9.64702206034544,0.688891676356318,
9.70347131113978));
#26125=CARTESIAN_POINT('Ctrl Pts',(-9.69912794294225,-0.591404032917394,
9.75119333459465));
#26126=CARTESIAN_POINT('Ctrl Pts',(-8.65162203056557,-1.32937658641912,
9.7989153580495));
#26127=CARTESIAN_POINT('Ctrl Pts',(-7.46260964658798,-0.845184363720304,
9.84663738150439));
#26128=CARTESIAN_POINT('Ctrl Pts',(-7.26895926387031,0.203731499573094,
9.8864057343834));
#26129=CARTESIAN_POINT('Ctrl Pts',(-7.69343845327961,0.855447168968696,
9.91822041668668));
#26130=CARTESIAN_POINT('Ctrl Pts',(-8.36897674068639,1.24088707119054,9.95003509898991));
#26131=CARTESIAN_POINT('Ctrl Pts',(-9.40469716198697,0.985920077451709,
9.98980345186895));
#26132=CARTESIAN_POINT('Ctrl Pts',(-9.81816654914519,-0.229495745901432,
10.0375254753238));
#26133=CARTESIAN_POINT('Ctrl Pts',(-9.01990129213503,-1.23181540830278,
10.0852474987787));
#26134=CARTESIAN_POINT('Ctrl Pts',(-7.7448815766716,-1.10454855729489,10.1329695222335));
#26135=CARTESIAN_POINT('Ctrl Pts',(-7.16248378137103,0.0395691664569845,
10.1806915456884));
#26136=CARTESIAN_POINT('Ctrl Pts',(-7.70231858265184,0.959516635784098,
10.2204598985675));
#26137=CARTESIAN_POINT('Ctrl Pts',(-8.44973620845025,1.17465098595439,10.2522745808707));
#26138=CARTESIAN_POINT('Ctrl Pts',(-9.21279948735437,1.02415072560454,10.2840892631739));
#26139=CARTESIAN_POINT('Ctrl Pts',(-9.82924696386352,0.153681043363534,
10.323857616053));
#26140=CARTESIAN_POINT('Ctrl Pts',(-9.34671359928637,-1.03600551613187,
10.3715796395079));
#26141=CARTESIAN_POINT('Ctrl Pts',(-8.08722621411818,-1.27172495272547,
10.4193016629627));
#26142=CARTESIAN_POINT('Ctrl Pts',(-7.20625633934821,-0.341260441884946,
10.4670236864176));
#26143=CARTESIAN_POINT('Ctrl Pts',(-7.51438819018325,0.905032990768513,
10.5147457098724));
#26144=CARTESIAN_POINT('Ctrl Pts',(-8.52454229492433,1.24754378427726,10.5545140627515));
#26145=CARTESIAN_POINT('Ctrl Pts',(-9.23053722819551,0.921220248238709,
10.5863287450547));
#26146=CARTESIAN_POINT('Ctrl Pts',(-9.70913721769566,0.308147702753446,
10.618143427358));
#26147=CARTESIAN_POINT('Ctrl Pts',(-9.60579769849225,-0.753476478756218,
10.657911780237));
#26148=CARTESIAN_POINT('Ctrl Pts',(-8.46249339286839,-1.33746947744375,
10.7056338036919));
#26149=CARTESIAN_POINT('Ctrl Pts',(-7.35577561545489,-0.691677028321873,
10.7533558271468));
#26150=CARTESIAN_POINT('Ctrl Pts',(-7.29832254473717,0.588389872605941,
10.8010778506016));
#26151=CARTESIAN_POINT('Ctrl Pts',(-8.34677181075405,1.32929924247705,10.8487998740565));
#26152=CARTESIAN_POINT('Ctrl Pts',(-9.33480180140853,0.927401622973597,
10.8885682269355));
#26153=CARTESIAN_POINT('Ctrl Pts',(-9.6552062007518,0.218700757404208,10.9203829092388));
#26154=CARTESIAN_POINT('Ctrl Pts',(-9.61602858438752,-0.558075278756368,
10.952197591542));
#26155=CARTESIAN_POINT('Ctrl Pts',(-8.84327939879723,-1.29331922138004,
10.9919659444211));
#26156=CARTESIAN_POINT('Ctrl Pts',(-7.59655740834266,-0.986925950743844,
11.0396879678759));
#26157=CARTESIAN_POINT('Ctrl Pts',(-7.18212680537146,0.22555885390601,11.0874099913308));
#26158=CARTESIAN_POINT('Ctrl Pts',(-7.97619852913042,1.23120403174577,11.1351320147857));
#26159=CARTESIAN_POINT('Ctrl Pts',(-9.25385315598159,1.10554094146089,11.1828540382405));
#26160=CARTESIAN_POINT('Ctrl Pts',(-9.73810097369181,0.155157329418831,
11.2226223911196));
#26161=CARTESIAN_POINT('Ctrl Pts',(-9.5167198222586,-0.590433900255586,
11.2544370734228));
#26162=CARTESIAN_POINT('Ctrl Pts',(-8.9788634278258,-1.15224026809512,11.286251755726));
#26163=CARTESIAN_POINT('Ctrl Pts',(-7.91341467193457,-1.20267743261775,
11.3260201086051));
#26164=CARTESIAN_POINT('Ctrl Pts',(-7.17104368741518,-0.155262577310692,
11.3737421320599));
#26165=CARTESIAN_POINT('Ctrl Pts',(-7.65093242556789,1.03283629280916,11.4214641555148));
#26166=CARTESIAN_POINT('Ctrl Pts',(-8.90942425196499,1.27381440193424,11.4691861789697));
#26167=CARTESIAN_POINT('Ctrl Pts',(-9.79343609406736,0.342838773468614,
11.5169082024246));
#26168=CARTESIAN_POINT('Ctrl Pts',(-9.53783414362817,-0.692725131815334,
11.5566765553036));
#26169=CARTESIAN_POINT('Ctrl Pts',(-8.88258928253219,-1.11173595265966,
11.5884912376068));
#26170=CARTESIAN_POINT('Ctrl Pts',(-8.10825553036941,-1.18469577885752,
11.6203059199101));
#26171=CARTESIAN_POINT('Ctrl Pts',(-7.2695063969436,-0.525738382531577,
11.6600742727892));
#26172=CARTESIAN_POINT('Ctrl Pts',(-7.39338734316738,0.752090271450184,
11.707796296244));
#26173=CARTESIAN_POINT('Ctrl Pts',(-8.53365284957409,1.33661289811649,11.7555183196989));
#26174=CARTESIAN_POINT('Ctrl Pts',(-9.64305837098596,0.695448710683353,
11.8032403431537));
#26175=CARTESIAN_POINT('Ctrl Pts',(-9.70247752610808,-0.586995019769853,
11.8509623666086));
#26176=CARTESIAN_POINT('Ctrl Pts',(-8.83163006088557,-1.20290869173268,
11.8907307194876));
#26177=CARTESIAN_POINT('Ctrl Pts',(-8.06194900837746,-1.09107411126975,
11.9225454017909));
#26178=CARTESIAN_POINT('Ctrl Pts',(-7.42862046025152,-0.639619965086561,
11.9543600840941));
#26179=CARTESIAN_POINT('Ctrl Pts',(-7.22545558163593,0.407494637567971,
11.9941284369732));
#26180=CARTESIAN_POINT('Ctrl Pts',(-8.15519732002207,1.29280410757092,12.0418504604281));
#26181=CARTESIAN_POINT('Ctrl Pts',(-9.39996773290423,0.988799592145459,
12.0895724838829));
#26182=CARTESIAN_POINT('Ctrl Pts',(-9.81945912529353,-0.221943608495,12.1372945073378));
#26183=CARTESIAN_POINT('Ctrl Pts',(-9.02531914992084,-1.23067263915149,
12.1850165307926));
#26184=CARTESIAN_POINT('Ctrl Pts',(-7.9637585258431,-1.12668225304343,12.2247848836717));
#26185=CARTESIAN_POINT('Ctrl Pts',(-7.45485568350695,-0.538520886546523,
12.2565995659749));
#26186=CARTESIAN_POINT('Ctrl Pts',(-7.27127580064357,0.217266333896634,
12.2884142482782));
#26187=CARTESIAN_POINT('Ctrl Pts',(-7.80273670592906,1.14207672805771,12.3281826011572));
#26188=CARTESIAN_POINT('Ctrl Pts',(-9.08509631350376,1.20328452686656,12.3759046246121));
#26189=CARTESIAN_POINT('Ctrl Pts',(-9.82755432320141,0.158953051700929,
12.4236266480669));
#26190=CARTESIAN_POINT('Ctrl Pts',(-9.35263231865442,-1.03113989247735,
12.4713486715218));
#26191=CARTESIAN_POINT('Ctrl Pts',(-8.09207117683376,-1.27440551994248,
12.5190706949767));
#26192=CARTESIAN_POINT('Ctrl Pts',(-7.35730114822946,-0.501205698382691,
12.5588390478557));
#26193=CARTESIAN_POINT('Ctrl Pts',(-7.35726327203958,0.276557694007757,
12.590653730159));
#26194=CARTESIAN_POINT('Ctrl Pts',(-7.71292602816593,0.968236737988355,
12.6224684124622));
#26195=CARTESIAN_POINT('Ctrl Pts',(-8.71992905550032,1.31990399824245,12.6622367653413));
#26196=CARTESIAN_POINT('Ctrl Pts',(-9.72976473982391,0.527171730423799,
12.7099587887961));
#26197=CARTESIAN_POINT('Ctrl Pts',(-9.60796699733264,-0.748382045827872,
12.757680812251));
#26198=CARTESIAN_POINT('Ctrl Pts',(-8.47015291907083,-1.3376623267597,12.8054028357058));
#26199=CARTESIAN_POINT('Ctrl Pts',(-7.35768579595222,-0.696874173190761,
12.8531248591607));
#26200=CARTESIAN_POINT('Ctrl Pts',(-7.30790187209926,0.368605305692363,
12.8928932120397));
#26201=CARTESIAN_POINT('Ctrl Pts',(-7.81674742644668,0.956816235375078,
12.924707894343));
#26202=CARTESIAN_POINT('Ctrl Pts',(-8.53826958993604,1.24719816244858,12.9565225766462));
#26203=CARTESIAN_POINT('Ctrl Pts',(-9.5299074510817,0.854286834872281,12.9962909295253));
#26204=CARTESIAN_POINT('Ctrl Pts',(-9.77493102244612,-0.405933783610824,
13.0440129529801));
#26205=CARTESIAN_POINT('Ctrl Pts',(-8.84825311836191,-1.29088586608074,
13.091734976435));
#26206=CARTESIAN_POINT('Ctrl Pts',(-7.60222377322338,-0.992083260269492,
13.1394569998899));
#26207=CARTESIAN_POINT('Ctrl Pts',(-7.18017100334371,0.220378704994195,
13.1871790233447));
#26208=CARTESIAN_POINT('Ctrl Pts',(-7.83964251650143,1.05872367117979,13.2269473762238));
#26209=CARTESIAN_POINT('Ctrl Pts',(-8.60931267292587,1.17063321629039,13.258762058527));
#26210=CARTESIAN_POINT('Ctrl Pts',(-9.34495698076375,0.918158765458134,
13.2905767408303));
#26211=CARTESIAN_POINT('Ctrl Pts',(-9.83781280395867,-0.0277894871107221,
13.3303450937093));
#26212=CARTESIAN_POINT('Ctrl Pts',(-9.19857689854507,-1.14114927397397,
13.3780671171642));
#26213=CARTESIAN_POINT('Ctrl Pts',(-7.91876815696661,-1.20409139949583,
13.425789140619));
#26214=CARTESIAN_POINT('Ctrl Pts',(-7.17195457572563,-0.162870192902413,
13.4735111640739));
#26215=CARTESIAN_POINT('Ctrl Pts',(-7.64606408151493,1.0301984280471,13.5212331875288));
#26216=CARTESIAN_POINT('Ctrl Pts',(-8.69330304862208,1.23272127803588,13.5610015404078));
#26217=CARTESIAN_POINT('Ctrl Pts',(-9.34858871730795,0.813774278533218,
13.5928162227111));
#26218=CARTESIAN_POINT('Ctrl Pts',(-9.73973345489619,0.14152306787283,13.6246309050143));
#26219=CARTESIAN_POINT('Ctrl Pts',(-9.49354329942793,-0.896318618679486,
13.6643992578933));
#26220=CARTESIAN_POINT('Ctrl Pts',(-8.28167117590845,-1.32006207173866,
13.7121212813482));
#26221=CARTESIAN_POINT('Ctrl Pts',(-7.27262985904281,-0.530310372124225,
13.7598433048031));
#26222=CARTESIAN_POINT('Ctrl Pts',(-7.38909870290544,0.745741011870611,
13.8075653282579));
#26223=CARTESIAN_POINT('Ctrl Pts',(-8.52824524889072,1.33780325905745,13.8552873517128));
#26224=CARTESIAN_POINT('Ctrl Pts',(-9.45272962828058,0.805775448450338,
13.8950557045918));
#26225=CARTESIAN_POINT('Ctrl Pts',(-9.67418339754811,0.0602057843313418,
13.9268703868951));
#26226=CARTESIAN_POINT('Ctrl Pts',(-9.53014810293605,-0.704104185434403,
13.9586850691983));
#26227=CARTESIAN_POINT('Ctrl Pts',(-8.66492803462685,-1.3278983761658,13.9984534220774));
#26228=CARTESIAN_POINT('Ctrl Pts',(-7.47119930507729,-0.855453376168864,
14.0461754455322));
#26229=CARTESIAN_POINT('Ctrl Pts',(-7.22482635377211,0.401993439824162,
14.0938974689871));
#26230=CARTESIAN_POINT('Ctrl Pts',(-8.14779983483422,1.29080842588256,14.141619492442));
#26231=CARTESIAN_POINT('Ctrl Pts',(-9.39665704501126,0.993237885736016,
14.1893415158968));
#26232=CARTESIAN_POINT('Ctrl Pts',(-9.74770684130611,-0.0139805610353641,
14.2291098687759));
#26233=CARTESIAN_POINT('Ctrl Pts',(-9.42737146932972,-0.722712629900664,
14.2609245510791));
#26234=CARTESIAN_POINT('Ctrl Pts',(-8.81837239209062,-1.20648532435468,
14.2927392333824));
#26235=CARTESIAN_POINT('Ctrl Pts',(-7.75591144824565,-1.11213649395108,
14.3325075862614));
#26236=CARTESIAN_POINT('Ctrl Pts',(-7.16226094067262,0.0261831591490891,
14.3802296097163));
#26237=CARTESIAN_POINT('Ctrl Pts',(-7.79866153250768,1.1383281195285,14.4279516331712));
#26238=CARTESIAN_POINT('Ctrl Pts',(-9.07819620829063,1.20661530463999,14.475673656626));
#26239=CARTESIAN_POINT('Ctrl Pts',(-9.82795448646243,0.164475639288861,
14.5233956800809));
#26240=CARTESIAN_POINT('Ctrl Pts',(-9.4344352553121,-0.826921139859,14.5631640329599));
#26241=CARTESIAN_POINT('Ctrl Pts',(-8.72847210856683,-1.15331343665297,
14.5949787152632));
#26242=CARTESIAN_POINT('Ctrl Pts',(-7.95139225442456,-1.12071288000722,
14.6267933975664));
#26243=CARTESIAN_POINT('Ctrl Pts',(-7.20963308932079,-0.354215456745463,
14.6665617504455));
#26244=CARTESIAN_POINT('Ctrl Pts',(-7.505461483611,0.895055578304256,14.7142837739003));
#26245=CARTESIAN_POINT('Ctrl Pts',(-8.71439455658622,1.31973540062164,14.7620057973552));
#26246=CARTESIAN_POINT('Ctrl Pts',(-9.72672576989096,0.534205235745722,
14.80972782081));
#26247=CARTESIAN_POINT('Ctrl Pts',(-9.61188293513649,-0.744467389276269,
14.8574498442649));
#26248=CARTESIAN_POINT('Ctrl Pts',(-8.66563268745192,-1.23674315419584,
14.897218197144));
#26249=CARTESIAN_POINT('Ctrl Pts',(-7.91819411292805,-1.02168160289173,
14.9290328794472));
#26250=CARTESIAN_POINT('Ctrl Pts',(-7.35185474755516,-0.488600347920775,
14.9608475617504));
#26251=CARTESIAN_POINT('Ctrl Pts',(-7.29240003379382,0.57638326010828,15.0006159146295));
#26252=CARTESIAN_POINT('Ctrl Pts',(-8.33349294198175,1.32759435244437,15.0483379380844));
#26253=CARTESIAN_POINT('Ctrl Pts',(-9.52561167002035,0.857780428739866,
15.0960599615392));
#26254=CARTESIAN_POINT('Ctrl Pts',(-9.7772346429653,-0.398626319625639,
15.1437819849941));
#26255=CARTESIAN_POINT('Ctrl Pts',(-8.85377588165687,-1.29048754584707,
15.1915040084489));
#26256=CARTESIAN_POINT('Ctrl Pts',(-7.81608520647529,-1.04366103090559,
15.231272361328));
#26257=CARTESIAN_POINT('Ctrl Pts',(-7.39154272749966,-0.391986857252505,
15.2630870436313));
#26258=CARTESIAN_POINT('Ctrl Pts',(-7.31203017292505,0.381701814578057,
15.2949017259345));
#26259=CARTESIAN_POINT('Ctrl Pts',(-7.96386448015173,1.22599852877905,15.3346700788135));
#26260=CARTESIAN_POINT('Ctrl Pts',(-9.24269458235218,1.11294042920609,15.3823921022684));
#26261=CARTESIAN_POINT('Ctrl Pts',(-9.83685155659984,-0.0223381454316971,
15.4301141257232));
#26262=CARTESIAN_POINT('Ctrl Pts',(-9.20509698430864,-1.13712765515967,
15.4778361491781));
#26263=CARTESIAN_POINT('Ctrl Pts',(-7.92321163699227,-1.2074086266698,15.525558172633));
#26264=CARTESIAN_POINT('Ctrl Pts',(-7.29993080976771,-0.341792293020232,
15.565326525512));
#26265=CARTESIAN_POINT('Ctrl Pts',(-7.4052713667291,0.428787139267935,15.5971412078153));
#26266=CARTESIAN_POINT('Ctrl Pts',(-7.85129778173277,1.06595545650788,15.6289558901185));
#26267=CARTESIAN_POINT('Ctrl Pts',(-8.89676621122576,1.27788697335264,15.6687242429976));
#26268=CARTESIAN_POINT('Ctrl Pts',(-9.78971211575288,0.355837225553599,
15.7164462664524));
#26269=CARTESIAN_POINT('Ctrl Pts',(-9.49661412050732,-0.891752812389575,
15.7641682899073));
#26270=CARTESIAN_POINT('Ctrl Pts',(-8.28879921167558,-1.32093775301506,
15.8118903133622));
#26271=CARTESIAN_POINT('Ctrl Pts',(-7.27465414055275,-0.536397493183267,
15.859612336817));
#26272=CARTESIAN_POINT('Ctrl Pts',(-7.38611196025228,0.74057287343298,15.9073343602719));
#26273=CARTESIAN_POINT('Ctrl Pts',(-8.52084029087267,1.33755299057858,15.9550563837267));
#26274=CARTESIAN_POINT('Ctrl Pts',(-9.63603663835765,0.705608630834653,
16.0027784071816));
#26275=CARTESIAN_POINT('Ctrl Pts',(-9.7085623613501,-0.57389414645679,16.0505004306365));
#26276=CARTESIAN_POINT('Ctrl Pts',(-8.66937749713867,-1.32730170138437,
16.0982224540913));
#26277=CARTESIAN_POINT('Ctrl Pts',(-7.67643438972821,-0.937451486116148,
16.1379908069704));
#26278=CARTESIAN_POINT('Ctrl Pts',(-7.34753951593156,-0.232645704807778,
16.1698054892736));
#26279=CARTESIAN_POINT('Ctrl Pts',(-7.37729180242736,0.544531299390573,
16.2016201715769));
#26280=CARTESIAN_POINT('Ctrl Pts',(-8.14111244251711,1.28907723916828,16.2413885244559));
#26281=CARTESIAN_POINT('Ctrl Pts',(-9.39143791719134,0.997777280360524,
16.2891105479108));
#26282=CARTESIAN_POINT('Ctrl Pts',(-9.82050642331186,-0.20960406273945,
16.3368325713656));
#26283=CARTESIAN_POINT('Ctrl Pts',(-9.03865128869567,-1.22478015611096,
16.3845545948205));
#26284=CARTESIAN_POINT('Ctrl Pts',(-7.75957206601839,-1.1145762256531,16.4322766182754));
#26285=CARTESIAN_POINT('Ctrl Pts',(-7.26386561656706,-0.170118697936401,
16.4720449711544));
#26286=CARTESIAN_POINT('Ctrl Pts',(-7.47621443170938,0.578095434489346,
16.5038596534576));
#26287=CARTESIAN_POINT('Ctrl Pts',(-8.0072372736111,1.14636498887337,16.5356743357609));
#26288=CARTESIAN_POINT('Ctrl Pts',(-9.07199831336541,1.2096831857704,16.5754426886399));
#26289=CARTESIAN_POINT('Ctrl Pts',(-9.82698149184862,0.171322491752237,
16.6231647120948));
#26290=CARTESIAN_POINT('Ctrl Pts',(-9.36149575518903,-1.02249284858247,
16.6708867355496));
#26291=CARTESIAN_POINT('Ctrl Pts',(-8.10601012202046,-1.27867249171228,
16.7186087590046));
#26292=CARTESIAN_POINT('Ctrl Pts',(-7.21080449715534,-0.358455431482571,
16.7663307824594));
#26293=CARTESIAN_POINT('Ctrl Pts',(-7.45386450952434,0.680123780107074,
16.8060991353384));
#26294=CARTESIAN_POINT('Ctrl Pts',(-8.10399429361696,1.10702794383478,16.8379138176417));
#26295=CARTESIAN_POINT('Ctrl Pts',(-8.87738910627695,1.18934657651432,16.8697284999449));
#26296=CARTESIAN_POINT('Ctrl Pts',(-9.72404578490763,0.540580495017656,
16.909496852824));
#26297=CARTESIAN_POINT('Ctrl Pts',(-9.6156268841698,-0.738652830313552,
16.9572188762788));
#26298=CARTESIAN_POINT('Ctrl Pts',(-8.48251348594472,-1.33692212764018,
17.0049408997337));
#26299=CARTESIAN_POINT('Ctrl Pts',(-7.36543538804804,-0.709221044626535,
17.0526629231886));
#26300=CARTESIAN_POINT('Ctrl Pts',(-7.29051177992318,0.572410341860231,
17.1003849466434));
#26301=CARTESIAN_POINT('Ctrl Pts',(-8.15384722142223,1.19881027348046,17.1401532995225));
#26302=CARTESIAN_POINT('Ctrl Pts',(-8.92482442462193,1.09629174757539,17.1719679818257));
#26303=CARTESIAN_POINT('Ctrl Pts',(-9.5635661681587,0.652529557847061,17.203782664129));
#26304=CARTESIAN_POINT('Ctrl Pts',(-9.77937911551377,-0.392051569085598,
17.243551017008));
#26305=CARTESIAN_POINT('Ctrl Pts',(-8.86041155411601,-1.28853981713131,
17.2912730404629));
#26306=CARTESIAN_POINT('Ctrl Pts',(-7.61205578954346,-0.99961074064383,
17.3389950639177));
#26307=CARTESIAN_POINT('Ctrl Pts',(-7.17795336035532,0.205970947653733,
17.3867170873726));
#26308=CARTESIAN_POINT('Ctrl Pts',(-7.95983654202789,1.22422987739285,17.4344391108275));
#26309=CARTESIAN_POINT('Ctrl Pts',(-9.02257711199641,1.13308471878594,17.4742074637065));
#26310=CARTESIAN_POINT('Ctrl Pts',(-9.53855547075963,0.551120605403174,
17.5060221460098));
#26311=CARTESIAN_POINT('Ctrl Pts',(-9.73126178565995,-0.202391287120677,
17.537836828313));
#26312=CARTESIAN_POINT('Ctrl Pts',(-9.21102362412759,-1.13356109670459,
17.5776051811921));
#26313=CARTESIAN_POINT('Ctrl Pts',(-7.92949798477055,-1.21027220049513,
17.6253272046469));
#26314=CARTESIAN_POINT('Ctrl Pts',(-7.17446499892724,-0.174995756025178,
17.6730492281018));
#26315=CARTESIAN_POINT('Ctrl Pts',(-7.63496028961901,1.0207534707931,17.7207712515566));
#26316=CARTESIAN_POINT('Ctrl Pts',(-8.89248740265649,1.27924547792269,17.7684932750115));
#26317=CARTESIAN_POINT('Ctrl Pts',(-9.63655413093407,0.514987888581546,
17.8082616278906));
#26318=CARTESIAN_POINT('Ctrl Pts',(-9.64599762203821,-0.262718171863597,
17.8400763101938));
#26319=CARTESIAN_POINT('Ctrl Pts',(-9.29872545955566,-0.958647723716373,
17.871890992497));
#26320=CARTESIAN_POINT('Ctrl Pts',(-8.29604883794672,-1.32246711774878,
17.9116593453761));
#26321=CARTESIAN_POINT('Ctrl Pts',(-7.2767003590985,-0.542004923633025,
17.959381368831));
#26322=CARTESIAN_POINT('Ctrl Pts',(-7.38306371835046,0.734928497495294,
18.0071033922858));
#26323=CARTESIAN_POINT('Ctrl Pts',(-8.51366833289497,1.33792545582631,18.0548254157407));
#26324=CARTESIAN_POINT('Ctrl Pts',(-9.63380326103061,0.710637403537144,
18.1025474391955));
#26325=CARTESIAN_POINT('Ctrl Pts',(-9.69646855898839,-0.354162117230549,
18.1423157920746));
#26326=CARTESIAN_POINT('Ctrl Pts',(-9.19477354323534,-0.948483585079254,
18.1741304743779));
#26327=CARTESIAN_POINT('Ctrl Pts',(-8.47681577631781,-1.24756976145674,
18.2059451566811));
#26328=CARTESIAN_POINT('Ctrl Pts',(-7.48049888881085,-0.866679201500626,
18.2457135095602));
#26329=CARTESIAN_POINT('Ctrl Pts',(-7.22025318433492,0.39048615400201,18.293435533015));
#26330=CARTESIAN_POINT('Ctrl Pts',(-8.13616145741442,1.28657998920588,18.3411575564699));
#26331=CARTESIAN_POINT('Ctrl Pts',(-9.38571315465714,1.00286766641441,18.3888795799247));
#26332=CARTESIAN_POINT('Ctrl Pts',(-9.82239755933068,-0.204401685672783,
18.4366016033796));
#26333=CARTESIAN_POINT('Ctrl Pts',(-9.17311251037952,-1.05066044291179,
18.4763699562587));
#26334=CARTESIAN_POINT('Ctrl Pts',(-8.40485197615202,-1.17186954952435,
18.5081846385619));
#26335=CARTESIAN_POINT('Ctrl Pts',(-7.66620824815671,-0.928309825697792,
18.5399993208651));
#26336=CARTESIAN_POINT('Ctrl Pts',(-7.16194896079103,0.0116090697930224,
18.5797676737441));
#26337=CARTESIAN_POINT('Ctrl Pts',(-7.78767408330682,1.1326178248109,18.627489697199));
#26338=CARTESIAN_POINT('Ctrl Pts',(-9.06662806970791,1.2110322804595,18.6752117206539));
#26339=CARTESIAN_POINT('Ctrl Pts',(-9.82597869561601,0.178918549750082,
18.7229337441087));
#26340=CARTESIAN_POINT('Ctrl Pts',(-9.36633182960527,-1.01979631056521,
18.7706557675636));
#26341=CARTESIAN_POINT('Ctrl Pts',(-8.32161858315476,-1.23496878019377,
18.8104241204427));
#26342=CARTESIAN_POINT('Ctrl Pts',(-7.66131443880895,-0.823976891055952,
18.8422388027459));
#26343=CARTESIAN_POINT('Ctrl Pts',(-7.26206866174134,-0.156505014891145,
18.8740534850491));
#26344=CARTESIAN_POINT('Ctrl Pts',(-7.49569002828134,0.884237996659342,
18.9138218379282));
#26345=CARTESIAN_POINT('Ctrl Pts',(-8.70234913605313,1.32260582783032,18.961543861383));
#26346=CARTESIAN_POINT('Ctrl Pts',(-9.72086726104124,0.545114377551589,
19.009265884838));
#26347=CARTESIAN_POINT('Ctrl Pts',(-9.61983842839294,-0.732252171704951,
19.0569879082928));
#26348=CARTESIAN_POINT('Ctrl Pts',(-8.48793508632651,-1.33804700660616,
19.1047099317477));
#26349=CARTESIAN_POINT('Ctrl Pts',(-7.55708441199681,-0.817238038658018,
19.1444782846267));
#26350=CARTESIAN_POINT('Ctrl Pts',(-7.32663054276847,-0.0744009702944177,
19.1762929669299));
#26351=CARTESIAN_POINT('Ctrl Pts',(-7.46141238152576,0.691594951312568,
19.2081076492332));
#26352=CARTESIAN_POINT('Ctrl Pts',(-8.31902553728147,1.32580677244966,19.2478760021122));
#26353=CARTESIAN_POINT('Ctrl Pts',(-9.51838032879036,0.86783227331379,19.2955980255671));
#26354=CARTESIAN_POINT('Ctrl Pts',(-9.77994177049436,-0.386543164264433,
19.343320049022));
#26355=CARTESIAN_POINT('Ctrl Pts',(-8.86778436426511,-1.28645482239925,
19.3910420724768));
#26356=CARTESIAN_POINT('Ctrl Pts',(-7.61541990833944,-1.00400867300409,
19.4387640959317));
#26357=CARTESIAN_POINT('Ctrl Pts',(-7.25221532801234,-0.00110918061983182,
19.4785324488107));
#26358=CARTESIAN_POINT('Ctrl Pts',(-7.56395646468766,0.711444929382833,
19.510347131114));
#26359=CARTESIAN_POINT('Ctrl Pts',(-8.16706066797269,1.20254697168893,19.5421618134172));
#26360=CARTESIAN_POINT('Ctrl Pts',(-9.23058489499091,1.12105355145988,19.5819301662963));
#26361=CARTESIAN_POINT('Ctrl Pts',(-9.83795787438773,-0.0100037510994853,
19.6296521897511));
#26362=CARTESIAN_POINT('Ctrl Pts',(-9.2150531670274,-1.12976348056569,19.677374213206));
#26363=CARTESIAN_POINT('Ctrl Pts',(-7.93643786504349,-1.21351929062353,
19.7250962366609));
#26364=CARTESIAN_POINT('Ctrl Pts',(-7.1741316504696,-0.180522779014628,
19.7728182601157));
#26365=CARTESIAN_POINT('Ctrl Pts',(-7.55563298498379,0.815560395604377,
19.8125866129948));
#26366=CARTESIAN_POINT('Ctrl Pts',(-8.25759739373146,1.15046615074881,19.844401295298));
#26367=CARTESIAN_POINT('Ctrl Pts',(-9.03501466770616,1.12726532957784,19.8762159776013));
#26368=CARTESIAN_POINT('Ctrl Pts',(-9.7859889682652,0.369794169139932,19.9159843304803));
#26369=CARTESIAN_POINT('Ctrl Pts',(-9.50528984170661,-0.882963013287452,
19.9637063539352));
#26370=CARTESIAN_POINT('Ctrl Pts',(-8.30158089336006,-1.32223160294103,
20.0114283773901));
#26371=CARTESIAN_POINT('Ctrl Pts',(-7.27982416395186,-0.549001163747792,
20.0591504008449));
#26372=CARTESIAN_POINT('Ctrl Pts',(-7.37919540779779,0.730966770878209,
20.1068724242998));
#26373=CARTESIAN_POINT('Ctrl Pts',(-8.31942329015859,1.23464969517342,20.1466407771788));
#26374=CARTESIAN_POINT('Ctrl Pts',(-9.06940798351601,1.02864276396269,20.1784554594821));
#26375=CARTESIAN_POINT('Ctrl Pts',(-9.6421525700082,0.502449325556989,20.2102701417853));
#26376=CARTESIAN_POINT('Ctrl Pts',(-9.71448195986604,-0.561737414803009,
20.2500384946644));
#26377=CARTESIAN_POINT('Ctrl Pts',(-8.68254968740398,-1.325483670326,20.2977605181192));
#26378=CARTESIAN_POINT('Ctrl Pts',(-7.48483661646242,-0.870120599928743,
20.3454825415741));
#26379=CARTESIAN_POINT('Ctrl Pts',(-7.21803807964812,0.38315138449426,20.3932045650289));
#26380=CARTESIAN_POINT('Ctrl Pts',(-8.13064396047136,1.28611487437685,20.4409265884838));
#26381=CARTESIAN_POINT('Ctrl Pts',(-9.17124354215662,1.05185546775307,20.4806949413628));
#26382=CARTESIAN_POINT('Ctrl Pts',(-9.6036359628206,0.405362861043841,20.5125096236661));
#26383=CARTESIAN_POINT('Ctrl Pts',(-9.692498679558,-0.367307387866645,20.5443243059693));
#26384=CARTESIAN_POINT('Ctrl Pts',(-9.05092306150429,-1.21942573957269,
20.5840926588484));
#26385=CARTESIAN_POINT('Ctrl Pts',(-7.77081777281899,-1.12183984072394,
20.6318146823033));
#26386=CARTESIAN_POINT('Ctrl Pts',(-7.16297774725796,0.00616841700814254,
20.6795367057581));
#26387=CARTESIAN_POINT('Ctrl Pts',(-7.78119991790399,1.12852017733444,20.727258729213));
#26388=CARTESIAN_POINT('Ctrl Pts',(-9.06215112949211,1.21429051780881,20.7749807526679));
#26389=CARTESIAN_POINT('Ctrl Pts',(-9.69583702513552,0.356288685259583,
20.8147491055469));
#26390=CARTESIAN_POINT('Ctrl Pts',(-9.59984873958507,-0.415528744586615,
20.8465637878501));
#26391=CARTESIAN_POINT('Ctrl Pts',(-9.16150960230265,-1.05800418902307,
20.8783784701533));
#26392=CARTESIAN_POINT('Ctrl Pts',(-8.11879282938344,-1.28265211460481,
20.9181468230325));
#26393=CARTESIAN_POINT('Ctrl Pts',(-7.21455735142713,-0.371306538997314,
20.9658688464872));
#26394=CARTESIAN_POINT('Ctrl Pts',(-7.49290834699324,0.879450371618512,
21.0135908699422));
#26395=CARTESIAN_POINT('Ctrl Pts',(-8.69477202257272,1.32374287831705,21.061312893397));
#26396=CARTESIAN_POINT('Ctrl Pts',(-9.71961335617614,0.550507598009665,
21.1090349168519));
#26397=CARTESIAN_POINT('Ctrl Pts',(-9.63746790001045,-0.512966465156227,
21.1488032697309));
#26398=CARTESIAN_POINT('Ctrl Pts',(-9.05989255998547,-1.03385284679082,
21.1806179520342));
#26399=CARTESIAN_POINT('Ctrl Pts',(-8.30803898706308,-1.23293097432144,
21.2124326343374));
#26400=CARTESIAN_POINT('Ctrl Pts',(-7.37249856131074,-0.720594101962636,
21.2522009872164));
#26401=CARTESIAN_POINT('Ctrl Pts',(-7.28494168448683,0.56023623461398,21.2999230106713));
#26402=CARTESIAN_POINT('Ctrl Pts',(-8.31378943939285,1.32400611056527,21.3476450341262));
#26403=CARTESIAN_POINT('Ctrl Pts',(-9.51339405973382,0.873649717202732,
21.395367057581));
#26404=CARTESIAN_POINT('Ctrl Pts',(-9.78252217127443,-0.381644119854083,
21.4430890810359));
#26405=CARTESIAN_POINT('Ctrl Pts',(-9.02459072764576,-1.1321538704598,21.482857433915));
#26406=CARTESIAN_POINT('Ctrl Pts',(-8.24699247568435,-1.14818055208414,
21.5146721162182));
#26407=CARTESIAN_POINT('Ctrl Pts',(-7.54814809080176,-0.806812097631549,
21.5464867985215));
#26408=CARTESIAN_POINT('Ctrl Pts',(-7.17585375677161,0.192748749863114,
21.5862551514005));
#26409=CARTESIAN_POINT('Ctrl Pts',(-7.94765887705949,1.21866756442476,21.6339771748554));
#26410=CARTESIAN_POINT('Ctrl Pts',(-9.22544694344921,1.12311766344225,21.6816991983102));
#26411=CARTESIAN_POINT('Ctrl Pts',(-9.83799322280595,-0.00234187907010109,
21.7294212217651));
#26412=CARTESIAN_POINT('Ctrl Pts',(-9.22020994520899,-1.12774686381815,
21.7771432452199));
#26413=CARTESIAN_POINT('Ctrl Pts',(-8.15597905940294,-1.19942378263886,
21.816911598099));
#26414=CARTESIAN_POINT('Ctrl Pts',(-7.55743187924388,-0.702777863395583,
21.8487262804022));
#26415=CARTESIAN_POINT('Ctrl Pts',(-7.25227867894974,0.0126223185498688,
21.8805409627055));
#26416=CARTESIAN_POINT('Ctrl Pts',(-7.62472145204494,1.0121278661905,21.9203093155845));
#26417=CARTESIAN_POINT('Ctrl Pts',(-8.87963869892395,1.28300654984747,21.9680313390394));
#26418=CARTESIAN_POINT('Ctrl Pts',(-9.78345388032542,0.374716814105572,
22.0157533624942));
#26419=CARTESIAN_POINT('Ctrl Pts',(-9.51032957548044,-0.877191824848875,
22.0634753859492));
#26420=CARTESIAN_POINT('Ctrl Pts',(-8.30680015382619,-1.32408050112826,
22.1111974094039));
#26421=CARTESIAN_POINT('Ctrl Pts',(-7.45507531503048,-0.681982566251019,
22.150965762283));
#26422=CARTESIAN_POINT('Ctrl Pts',(-7.32736698200152,0.0852243664941577,
22.1827804445863));
#26423=CARTESIAN_POINT('Ctrl Pts',(-7.56466512489233,0.825903438264024,
22.2145951268895));
#26424=CARTESIAN_POINT('Ctrl Pts',(-8.50028162665128,1.33810136937232,22.2543634797686));
#26425=CARTESIAN_POINT('Ctrl Pts',(-9.62654717627403,0.721888362768944,
22.3020855032234));
#26426=CARTESIAN_POINT('Ctrl Pts',(-9.7157855740631,-0.55635599358315,22.3498075266783));
#26427=CARTESIAN_POINT('Ctrl Pts',(-8.69013696978794,-1.32441658151506,
22.3975295501331));
#26428=CARTESIAN_POINT('Ctrl Pts',(-7.48757400439743,-0.874933687463104,
22.4452515735881));
#26429=CARTESIAN_POINT('Ctrl Pts',(-7.26356541515204,0.167920622083289,
22.485019926467));
#26430=CARTESIAN_POINT('Ctrl Pts',(-7.6689528934835,0.83168028369988,22.5168346087703));
#26431=CARTESIAN_POINT('Ctrl Pts',(-8.33302111081603,1.23656211671549,22.5486492910735));
#26432=CARTESIAN_POINT('Ctrl Pts',(-9.37570451013549,1.01175934142366,22.5884176439526));
#26433=CARTESIAN_POINT('Ctrl Pts',(-9.82427138668064,-0.19114560704095,
22.6361396674074));
#26434=CARTESIAN_POINT('Ctrl Pts',(-9.05542987457454,-1.21620894920483,
22.6838616908623));
#26435=CARTESIAN_POINT('Ctrl Pts',(-7.77725385403873,-1.12599705024939,
22.7315837143172));
#26436=CARTESIAN_POINT('Ctrl Pts',(-7.1618988042227,0.000737488335527086,
22.7793057377721));
#26437=CARTESIAN_POINT('Ctrl Pts',(-7.67480916412578,0.935963622326308,
22.8190740906511));
#26438=CARTESIAN_POINT('Ctrl Pts',(-8.41566875034181,1.17269758585735,22.8508887729544));
#26439=CARTESIAN_POINT('Ctrl Pts',(-9.18277819629672,1.04440497537631,22.8827034552576));
#26440=CARTESIAN_POINT('Ctrl Pts',(-9.8242272605525,0.192191353705862,22.9224718081366));
#26441=CARTESIAN_POINT('Ctrl Pts',(-9.37642209067293,-1.01099736283169,
22.9701938315915));
#26442=CARTESIAN_POINT('Ctrl Pts',(-8.1243057998852,-1.28316811903035,23.0179158550463));
#26443=CARTESIAN_POINT('Ctrl Pts',(-7.21670468463048,-0.378661434823841,
23.0656378785012));
#26444=CARTESIAN_POINT('Ctrl Pts',(-7.48853905055207,0.876049143468286,
23.1133599019561));
#26445=CARTESIAN_POINT('Ctrl Pts',(-8.48832796542965,1.24773057249471,23.1531282548351));
#26446=CARTESIAN_POINT('Ctrl Pts',(-9.20349553135788,0.942032602888077,
23.1849429371384));
#26447=CARTESIAN_POINT('Ctrl Pts',(-9.69968544546749,0.343107344518375,
23.2167576194416));
#26448=CARTESIAN_POINT('Ctrl Pts',(-9.6271980157496,-0.72106864258534,23.2565259723207));
#26449=CARTESIAN_POINT('Ctrl Pts',(-8.50132284585153,-1.33799461835653,
23.3042479957755));
#26450=CARTESIAN_POINT('Ctrl Pts',(-7.37633015273652,-0.724591352450931,
23.3519700192304));
#26451=CARTESIAN_POINT('Ctrl Pts',(-7.2817534589978,0.553269115357387,23.3996920426852));
#26452=CARTESIAN_POINT('Ctrl Pts',(-8.30825979254401,1.3242926590729,23.4474140661402));
#26453=CARTESIAN_POINT('Ctrl Pts',(-9.3075368060717,0.951237154850738,23.4871824190191));
#26454=CARTESIAN_POINT('Ctrl Pts',(-9.64837291280723,0.252132982124907,
23.5189971013224));
#26455=CARTESIAN_POINT('Ctrl Pts',(-9.63175400718011,-0.525452838188874,
23.5508117836256));
#26456=CARTESIAN_POINT('Ctrl Pts',(-8.8806672240812,-1.28281246429085,23.5905801365047));
#26457=CARTESIAN_POINT('Ctrl Pts',(-7.62557872246267,-1.01272838316213,
23.6383021599596));
#26458=CARTESIAN_POINT('Ctrl Pts',(-7.17613609374723,0.187218886379039,
23.6860241834144));
#26459=CARTESIAN_POINT('Ctrl Pts',(-7.94068933163074,1.21548464610644,23.7337462068693));
#26460=CARTESIAN_POINT('Ctrl Pts',(-9.22145261230867,1.1269522981132,23.7814682303241));
#26461=CARTESIAN_POINT('Ctrl Pts',(-9.73307681667046,0.191021941459234,
23.8212365832032));
#26462=CARTESIAN_POINT('Ctrl Pts',(-9.53342612569965,-0.560679792988806,
23.8530512655064));
#26463=CARTESIAN_POINT('Ctrl Pts',(-9.01210000646154,-1.13785825185349,
23.8848659478097));
#26464=CARTESIAN_POINT('Ctrl Pts',(-7.94856368871474,-1.21919372891504,
23.9246343006887));
#26465=CARTESIAN_POINT('Ctrl Pts',(-7.1761091647714,-0.193763786786585,
23.9723563241436));
#26466=CARTESIAN_POINT('Ctrl Pts',(-7.62131689716979,1.00776116143484,24.0200783475984));
#26467=CARTESIAN_POINT('Ctrl Pts',(-8.87228544066663,1.28515948400961,24.0678003710534));
#26468=CARTESIAN_POINT('Ctrl Pts',(-9.78294207479748,0.380230176003933,
24.1155223945081));
#26469=CARTESIAN_POINT('Ctrl Pts',(-9.55750006810439,-0.662315199801606,
24.1552907473873));
#26470=CARTESIAN_POINT('Ctrl Pts',(-8.91469096537924,-1.10016489253993,
24.1871054296905));
#26471=CARTESIAN_POINT('Ctrl Pts',(-8.14280065349016,-1.19556532434741,
24.2189201119937));
#26472=CARTESIAN_POINT('Ctrl Pts',(-7.28528169296711,-0.561226147456453,
24.2586884648727));
#26473=CARTESIAN_POINT('Ctrl Pts',(-7.37202759718887,0.719659368846581,
24.3064104883277));
#26474=CARTESIAN_POINT('Ctrl Pts',(-8.49484987781715,1.33702656291388,24.3541325117825));
#26475=CARTESIAN_POINT('Ctrl Pts',(-9.62239486975506,0.728327608305291,
24.4018545352374));
#26476=CARTESIAN_POINT('Ctrl Pts',(-9.71900579594374,-0.551851631768187,
24.4495765586922));
#26477=CARTESIAN_POINT('Ctrl Pts',(-8.86639905928022,-1.19277807964749,
24.4893449115712));
#26478=CARTESIAN_POINT('Ctrl Pts',(-8.09379671343249,-1.10332691326113,
24.5211595938745));
#26479=CARTESIAN_POINT('Ctrl Pts',(-7.44763360975285,-0.6704422410672,24.5529742761777));
#26480=CARTESIAN_POINT('Ctrl Pts',(-7.21416680485634,0.3703354537393,24.5927426290568));
#26481=CARTESIAN_POINT('Ctrl Pts',(-8.11782508502159,1.2822533614826,24.6404646525117));
#26482=CARTESIAN_POINT('Ctrl Pts',(-9.37089350882629,1.014500394273,24.6881866759665));
#26483=CARTESIAN_POINT('Ctrl Pts',(-9.82534425375221,-0.183559139565816,
24.7359086994214));
#26484=CARTESIAN_POINT('Ctrl Pts',(-9.06081228708266,-1.21490943394426,
24.7836307228763));
#26485=CARTESIAN_POINT('Ctrl Pts',(-7.99668094234245,-1.14176956700014,
24.8233990757553));
#26486=CARTESIAN_POINT('Ctrl Pts',(-7.47092386605872,-0.568624391050042,
24.8552137580586));
#26487=CARTESIAN_POINT('Ctrl Pts',(-7.26548819241141,0.181516982272607,
24.8870284403618));
#26488=CARTESIAN_POINT('Ctrl Pts',(-7.76988706005669,1.12136098066457,24.9267967932408));
#26489=CARTESIAN_POINT('Ctrl Pts',(-9.04993030585202,1.21975735594326,24.9745188166957));
#26490=CARTESIAN_POINT('Ctrl Pts',(-9.82238233795618,0.19741202080254,25.0222408401506));
#26491=CARTESIAN_POINT('Ctrl Pts',(-9.38219711576266,-1.00596202592954,
25.0699628636054));
#26492=CARTESIAN_POINT('Ctrl Pts',(-8.12922651266813,-1.28570695538346,
25.1176848870603));
#26493=CARTESIAN_POINT('Ctrl Pts',(-7.37232752343053,-0.534155973023465,
25.1574532399393));
#26494=CARTESIAN_POINT('Ctrl Pts',(-7.34971879980421,0.243278745517771,
25.1892679222426));
#26495=CARTESIAN_POINT('Ctrl Pts',(-7.68515908277749,0.94498788222336,25.2210826045458));
#26496=CARTESIAN_POINT('Ctrl Pts',(-8.68153252474089,1.32573047656409,25.2608509574249));
#26497=CARTESIAN_POINT('Ctrl Pts',(-9.71394815471084,0.562637739887994,
25.3085729808797));
#26498=CARTESIAN_POINT('Ctrl Pts',(-9.62921855937965,-0.715913401780119,
25.3562950043346));
#26499=CARTESIAN_POINT('Ctrl Pts',(-8.50898474258058,-1.33796510532709,
25.4040170277894));
#26500=CARTESIAN_POINT('Ctrl Pts',(-7.37839035099148,-0.729730874556245,
25.4517390512443));
#26501=CARTESIAN_POINT('Ctrl Pts',(-7.29770694788286,0.333855110429494,
25.4915074041234));
#26502=CARTESIAN_POINT('Ctrl Pts',(-7.78926817953549,0.936585109279324,
25.5233220864266));
#26503=CARTESIAN_POINT('Ctrl Pts',(-8.50205950886568,1.24778346533051,25.5551367687299));
#26504=CARTESIAN_POINT('Ctrl Pts',(-9.50468208918595,0.883815169420991,
25.5949051216089));
#26505=CARTESIAN_POINT('Ctrl Pts',(-9.7861743400752,-0.368764037840361,
25.6426271450638));
#26506=CARTESIAN_POINT('Ctrl Pts',(-8.88556823233645,-1.2802357954333,25.6903491685186));
#26507=CARTESIAN_POINT('Ctrl Pts',(-7.63139236705886,-1.01771908141124,
25.7380711919735));
#26508=CARTESIAN_POINT('Ctrl Pts',(-7.17433144450681,0.181984161415946,
25.7857932154284));
#26509=CARTESIAN_POINT('Ctrl Pts',(-7.80919625071778,1.03911404470665,25.8255615683074));
#26510=CARTESIAN_POINT('Ctrl Pts',(-8.57529460171618,1.173312452204,25.8573762506107));
#26511=CARTESIAN_POINT('Ctrl Pts',(-9.31795593805921,0.942292895719095,
25.8891909329139));
#26512=CARTESIAN_POINT('Ctrl Pts',(-9.83805580732715,0.0110458366725677,
25.928959285793));
#26513=CARTESIAN_POINT('Ctrl Pts',(-9.23139907623976,-1.12039579611305,
25.9766813092478));
#26514=CARTESIAN_POINT('Ctrl Pts',(-7.95395595261882,-1.22045174096127,
26.0244033327027));
#26515=CARTESIAN_POINT('Ctrl Pts',(-7.17724044410301,-0.20134176406142,
26.0721253561575));
#26516=CARTESIAN_POINT('Ctrl Pts',(-7.61652715495395,1.00498312726924,26.1198473796124));
#26517=CARTESIAN_POINT('Ctrl Pts',(-8.65744779364467,1.237811783029,26.1596157324915));
#26518=CARTESIAN_POINT('Ctrl Pts',(-9.32461540559779,0.838057766741282,
26.1914304147947));
#26519=CARTESIAN_POINT('Ctrl Pts',(-9.73510427955986,0.177440797287226,
26.223245097098));
#26520=CARTESIAN_POINT('Ctrl Pts',(-9.51913620553223,-0.867108268097489,
26.263013449977));
#26521=CARTESIAN_POINT('Ctrl Pts',(-8.32007162001735,-1.32584204441894,
26.3107354734319));
#26522=CARTESIAN_POINT('Ctrl Pts',(-7.28853651967721,-0.565705567888474,
26.3584574968867));
#26523=CARTESIAN_POINT('Ctrl Pts',(-7.3679250200947,0.713188326141545,26.4061795203416));
#26524=CARTESIAN_POINT('Ctrl Pts',(-8.48941001014702,1.33805949275231,26.4539015437964));
#26525=CARTESIAN_POINT('Ctrl Pts',(-9.42894458279322,0.833084497531996,
26.4936698966755));
#26526=CARTESIAN_POINT('Ctrl Pts',(-9.67194167558743,0.0942554856010431,
26.5254845789787));
#26527=CARTESIAN_POINT('Ctrl Pts',(-9.55014748720162,-0.673912511423524,
26.557299261282));
#26528=CARTESIAN_POINT('Ctrl Pts',(-8.70339447170565,-1.32255285070552,
26.597067614161));
#26529=CARTESIAN_POINT('Ctrl Pts',(-7.49645805411769,-0.884949101093904,
26.6447896376159));
#26530=CARTESIAN_POINT('Ctrl Pts',(-7.21369748796687,0.364818312633921,
26.6925116610707));
#26531=CARTESIAN_POINT('Ctrl Pts',(-8.11048863058951,1.28004384369136,26.7402336845256));
#26532=CARTESIAN_POINT('Ctrl Pts',(-9.36745541506446,1.01884074167898,26.7879557079805));
#26533=CARTESIAN_POINT('Ctrl Pts',(-9.74758705702552,0.0222340520690824,
26.8277240608595));
#26534=CARTESIAN_POINT('Ctrl Pts',(-9.44795416168687,-0.69549571881149,
26.8595387431628));
#26535=CARTESIAN_POINT('Ctrl Pts',(-8.85325076894622,-1.19673794632238,
26.891353425466));
#26536=CARTESIAN_POINT('Ctrl Pts',(-7.78849928368159,-1.13326170177414,
26.9311217783451));
#26537=CARTESIAN_POINT('Ctrl Pts',(-7.16206452223313,-0.0126493480035826,
26.9788438017999));
#26538=CARTESIAN_POINT('Ctrl Pts',(-7.76592238843451,1.11749568853494,27.0265658252548));
#26539=CARTESIAN_POINT('Ctrl Pts',(-9.04293644689573,1.22288648831542,27.0742878487096));
#26540=CARTESIAN_POINT('Ctrl Pts',(-9.82262206597892,0.202943895240207,
27.1220098721645));
#26541=CARTESIAN_POINT('Ctrl Pts',(-9.45803912628356,-0.799455346119385,
27.1617782250435));
#26542=CARTESIAN_POINT('Ctrl Pts',(-8.76184528940354,-1.14619737914625,
27.1935929073468));
#26543=CARTESIAN_POINT('Ctrl Pts',(-7.98414664679625,-1.13616158002172,
27.22540758965));
#26544=CARTESIAN_POINT('Ctrl Pts',(-7.22045596972938,-0.391512999309722,
27.2651759425291));
#26545=CARTESIAN_POINT('Ctrl Pts',(-7.47990565042312,0.8658168782332,27.312897965984));
#26546=CARTESIAN_POINT('Ctrl Pts',(-8.67600524947205,1.32540133765365,27.3606199894388));
#26547=CARTESIAN_POINT('Ctrl Pts',(-9.71070635102469,0.569580091172984,
27.4083420128937));
#26548=CARTESIAN_POINT('Ctrl Pts',(-9.63301924336791,-0.711886752361416,
27.4560640363486));
#26549=CARTESIAN_POINT('Ctrl Pts',(-8.70145348389303,-1.23141557232169,
27.4958323892276));
#26550=CARTESIAN_POINT('Ctrl Pts',(-7.94808857747159,-1.03813542913593,
27.5276470715309));
#26551=CARTESIAN_POINT('Ctrl Pts',(-7.36651760850961,-0.521713988800611,
27.5594617538341));
#26552=CARTESIAN_POINT('Ctrl Pts',(-7.27618187297965,0.541095690248971,
27.5992301067131));
#26553=CARTESIAN_POINT('Ctrl Pts',(-8.29503599950346,1.3222031262906,27.646952130168));
#26554=CARTESIAN_POINT('Ctrl Pts',(-9.50028672025696,0.8871826367628,27.6946741536229));
#26555=CARTESIAN_POINT('Ctrl Pts',(-9.78826494942713,-0.361392817789259,
27.7423961770777));
#26556=CARTESIAN_POINT('Ctrl Pts',(-8.89107706408667,-1.27967733588393,
27.7901182005326));
#26557=CARTESIAN_POINT('Ctrl Pts',(-7.84666060597338,-1.06306888494675,
27.8298865534116));
#26558=CARTESIAN_POINT('Ctrl Pts',(-7.40338501873419,-0.42398935176246,
27.8617012357149));
#26559=CARTESIAN_POINT('Ctrl Pts',(-7.30145370852712,0.34706570721632,27.8935159180181));
#26560=CARTESIAN_POINT('Ctrl Pts',(-7.92851098567795,1.20992382427112,27.9332842708972));
#26561=CARTESIAN_POINT('Ctrl Pts',(-9.2100849376435,1.13402413113834,27.981006294352));
#26562=CARTESIAN_POINT('Ctrl Pts',(-9.8369350579009,0.0164682923010958,
28.0287283178069));
#26563=CARTESIAN_POINT('Ctrl Pts',(-9.23780294045469,-1.11618912811791,
28.0764503412618));
#26564=CARTESIAN_POINT('Ctrl Pts',(-7.95848741323725,-1.22363371660283,
28.1241723647166));
#26565=CARTESIAN_POINT('Ctrl Pts',(-7.31036634376251,-0.376483176085945,
28.1639407175957));
#26566=CARTESIAN_POINT('Ctrl Pts',(-7.39327398065573,0.396848718847905,
28.1957553998989));
#26567=CARTESIAN_POINT('Ctrl Pts',(-7.82067316599591,1.04665317585658,28.2275700822022));
#26568=CARTESIAN_POINT('Ctrl Pts',(-8.85943719755328,1.28892212916213,28.2673384350812));
#26569=CARTESIAN_POINT('Ctrl Pts',(-9.77897218441442,0.393015903201587,
28.3150604585361));
#26570=CARTESIAN_POINT('Ctrl Pts',(-9.52183643350912,-0.862274235290551,
28.3627824819909));
#26571=CARTESIAN_POINT('Ctrl Pts',(-8.32766689782281,-1.32685065118973,
28.4105045054458));
#26572=CARTESIAN_POINT('Ctrl Pts',(-7.28988155219882,-0.571076786729173,
28.4582265289006));
#26573=CARTESIAN_POINT('Ctrl Pts',(-7.35401058852779,0.4936355808648,28.4979948817797));
#26574=CARTESIAN_POINT('Ctrl Pts',(-7.92268452713421,1.02422567452007,28.529809564083));
#26575=CARTESIAN_POINT('Ctrl Pts',(-8.67105994361954,1.23600417218416,28.5616242463862));
#26576=CARTESIAN_POINT('Ctrl Pts',(-9.61514016258385,0.739579455901104,
28.6013925992652));
#26577=CARTESIAN_POINT('Ctrl Pts',(-9.72436898518915,-0.539584967461109,
28.6491146227201));
#26578=CARTESIAN_POINT('Ctrl Pts',(-8.70859933360693,-1.32066379967392,
28.696836646175));
#26579=CARTESIAN_POINT('Ctrl Pts',(-7.50154209854002,-0.890681293407978,
28.7445586696298));
#26580=CARTESIAN_POINT('Ctrl Pts',(-7.21120039694662,0.359876283869756,
28.7922806930847));
#26581=CARTESIAN_POINT('Ctrl Pts',(-7.95631706256593,1.12311027083399,28.8320490459638));
#26582=CARTESIAN_POINT('Ctrl Pts',(-8.73353253024973,1.15229941527241,28.863863728267));
#26583=CARTESIAN_POINT('Ctrl Pts',(-9.43805614056221,0.822811344328694,
28.8956784105702));
#26584=CARTESIAN_POINT('Ctrl Pts',(-9.82721969175024,-0.170303293380481,
28.9354467634493));
#26585=CARTESIAN_POINT('Ctrl Pts',(-9.07289405752337,-1.2091417450888,28.9831687869042));
#26586=CARTESIAN_POINT('Ctrl Pts',(-7.79367140603468,-1.13523854117236,
29.030890810359));
#26587=CARTESIAN_POINT('Ctrl Pts',(-7.16215896705078,-0.0203107034760627,
29.0786128338139));
#26588=CARTESIAN_POINT('Ctrl Pts',(-7.76080034695112,1.11539202291376,29.1263348572687));
#26589=CARTESIAN_POINT('Ctrl Pts',(-8.82366560643313,1.20507622033222,29.1661032101478));
#26590=CARTESIAN_POINT('Ctrl Pts',(-9.43053464406366,0.718634766301466,
29.197917892451));
#26591=CARTESIAN_POINT('Ctrl Pts',(-9.74775700628796,0.00850363864441496,
29.2297325747543));
#26592=CARTESIAN_POINT('Ctrl Pts',(-9.39228672033525,-0.997164717746648,
29.2695009276333));
#26593=CARTESIAN_POINT('Ctrl Pts',(-8.14213995932516,-1.28924928143331,
29.3172229510882));
#26594=CARTESIAN_POINT('Ctrl Pts',(-7.22306871510535,-0.396393259163025,
29.364944974543));
#26595=CARTESIAN_POINT('Ctrl Pts',(-7.47497441546891,0.859963540492578,
29.4126669979979));
#26596=CARTESIAN_POINT('Ctrl Pts',(-8.67073545386039,1.32715695287662,29.4603890214527));
#26597=CARTESIAN_POINT('Ctrl Pts',(-9.53326385014039,0.699583561916176,
29.5001573743319));
#26598=CARTESIAN_POINT('Ctrl Pts',(-9.67386119595553,-0.0653703009610333,
29.531972056635));
#26599=CARTESIAN_POINT('Ctrl Pts',(-9.44929686259604,-0.809923379715055,
29.5637867389383));
#26600=CARTESIAN_POINT('Ctrl Pts',(-8.52213151947877,-1.33797052146522,
29.6035550918174));
#26601=CARTESIAN_POINT('Ctrl Pts',(-7.38624034864398,-0.740763047589384,
29.6512771152722));
#26602=CARTESIAN_POINT('Ctrl Pts',(-7.27422930025927,0.535519851685437,
29.6989991387271));
#26603=CARTESIAN_POINT('Ctrl Pts',(-8.2888747001765,1.32134053301234,29.7467211621819));
#26604=CARTESIAN_POINT('Ctrl Pts',(-9.29366927115465,0.962938239586792,
29.786489515061));
#26605=CARTESIAN_POINT('Ctrl Pts',(-9.64466888997224,0.268650789364219,
29.8183041973642));
#26606=CARTESIAN_POINT('Ctrl Pts',(-9.63899688479749,-0.508672370426549,
29.8501188796675));
#26607=CARTESIAN_POINT('Ctrl Pts',(-8.89986075464358,-1.27780800896432,
29.8898872325465));
#26608=CARTESIAN_POINT('Ctrl Pts',(-7.63927858840787,-1.02415996628783,
29.9376092560014));
#26609=CARTESIAN_POINT('Ctrl Pts',(-7.25303160763693,-0.0327948314514716,
29.9773776088804));
#26610=CARTESIAN_POINT('Ctrl Pts',(-7.54670173216219,0.690609604732206,
30.0091922911837));
#26611=CARTESIAN_POINT('Ctrl Pts',(-7.84279804142178,0.939512810771537,
30.0250996323353));
#26612=CARTESIAN_POINT('Ctrl Pts',(-8.01282215114119,1.02066752383247,30.0330533029111));
#26613=CARTESIAN_POINT('Ctrl Pts',(-7.87660126793166,-0.874219306856458,
1.76694669708889));
#26614=CARTESIAN_POINT('Ctrl Pts',(-7.73097269067503,-0.770372743754183,
1.7749003676647));
#26615=CARTESIAN_POINT('Ctrl Pts',(-7.49505426275024,-0.488941412697979,
1.79080770881633));
#26616=CARTESIAN_POINT('Ctrl Pts',(-7.33944865341066,0.235760887270365,
1.82262239111956));
#26617=CARTESIAN_POINT('Ctrl Pts',(-7.86365505261755,1.09918250918611,1.86239074399862));
#26618=CARTESIAN_POINT('Ctrl Pts',(-9.08404871094944,1.12901342715983,1.91011276745348));
#26619=CARTESIAN_POINT('Ctrl Pts',(-9.64865400304555,0.288282690195508,
1.94988112033254));
#26620=CARTESIAN_POINT('Ctrl Pts',(-9.52610611016745,-0.439466000029754,
1.98169580263577));
#26621=CARTESIAN_POINT('Ctrl Pts',(-9.08371912176839,-1.03091022985107,
2.01351048493902));
#26622=CARTESIAN_POINT('Ctrl Pts',(-8.08526338637744,-1.20075991772491,
2.05327883781807));
#26623=CARTESIAN_POINT('Ctrl Pts',(-7.26579462249314,-0.299113479422665,
2.10100086127293));
#26624=CARTESIAN_POINT('Ctrl Pts',(-7.58044611662734,0.875818431377988,
2.14872288472779));
#26625=CARTESIAN_POINT('Ctrl Pts',(-8.74075814219729,1.24739438139292,2.19644490818265));
#26626=CARTESIAN_POINT('Ctrl Pts',(-9.52082863358897,0.601160787975269,
2.23621326106171));
#26627=CARTESIAN_POINT('Ctrl Pts',(-9.60834021877745,-0.131949724327797,
2.26802794336495));
#26628=CARTESIAN_POINT('Ctrl Pts',(-9.35106143617397,-0.824074962016934,
2.29984262566819));
#26629=CARTESIAN_POINT('Ctrl Pts',(-8.44135567630907,-1.26900551071649,
2.33961097854724));
#26630=CARTESIAN_POINT('Ctrl Pts',(-7.40013276896415,-0.635493945930393,
2.38733300200211));
#26631=CARTESIAN_POINT('Ctrl Pts',(-7.37123600950541,0.580662319132022,
2.43505502545696));
#26632=CARTESIAN_POINT('Ctrl Pts',(-8.37744343232561,1.26433851735166,2.48277704891183));
#26633=CARTESIAN_POINT('Ctrl Pts',(-9.49831957514312,0.785612751107122,
2.53049907236669));
#26634=CARTESIAN_POINT('Ctrl Pts',(-9.66528404865682,-0.213177748400982,
2.57026742524574));
#26635=CARTESIAN_POINT('Ctrl Pts',(-9.2518736926554,-0.82499175948189,2.60208210754898));
#26636=CARTESIAN_POINT('Ctrl Pts',(-8.6044284386178,-1.18001050930349,2.63389678985223));
#26637=CARTESIAN_POINT('Ctrl Pts',(-7.6253748932976,-0.921337331474078,
2.67366514273128));
#26638=CARTESIAN_POINT('Ctrl Pts',(-7.25242721212033,0.239034337796918,
2.72138716618614));
#26639=CARTESIAN_POINT('Ctrl Pts',(-8.0262858459658,1.17764965562183,2.769109189641));
#26640=CARTESIAN_POINT('Ctrl Pts',(-9.23454501169552,1.0363489218597,2.81683121309586));
#26641=CARTESIAN_POINT('Ctrl Pts',(-9.76899309284508,-0.059058723161371,
2.86455323655073));
#26642=CARTESIAN_POINT('Ctrl Pts',(-9.24177187839627,-0.923636465033414,
2.90432158942978));
#26643=CARTESIAN_POINT('Ctrl Pts',(-8.52883239433566,-1.11583816367411,
2.93613627173302));
#26644=CARTESIAN_POINT('Ctrl Pts',(-7.8069182369327,-0.960711973455134,
2.96795095403626));
#26645=CARTESIAN_POINT('Ctrl Pts',(-7.23575031818529,-0.124515764873949,
3.00771930691532));
#26646=CARTESIAN_POINT('Ctrl Pts',(-7.71291403621515,0.997031160766364,
3.05544133037017));
#26647=CARTESIAN_POINT('Ctrl Pts',(-8.9122634679914,1.20054261779448,3.10316335382504));
#26648=CARTESIAN_POINT('Ctrl Pts',(-9.73356335662679,0.30314500910545,3.1508853772799));
#26649=CARTESIAN_POINT('Ctrl Pts',(-9.42103936740634,-0.874938806376356,
3.19860740073476));
#26650=CARTESIAN_POINT('Ctrl Pts',(-8.45665156776007,-1.18382884768558,
3.23837575361381));
#26651=CARTESIAN_POINT('Ctrl Pts',(-7.7917351978084,-0.86272074661816,3.27019043591706));
#26652=CARTESIAN_POINT('Ctrl Pts',(-7.34728101473615,-0.273072825713877,
3.3020051182203));
#26653=CARTESIAN_POINT('Ctrl Pts',(-7.46243893945415,0.733006464555997,
3.34177347109935));
#26654=CARTESIAN_POINT('Ctrl Pts',(-8.55710010482131,1.26898188682335,3.38949549455421));
#26655=CARTESIAN_POINT('Ctrl Pts',(-9.59726535329547,0.638179041168183,
3.43721751800907));
#26656=CARTESIAN_POINT('Ctrl Pts',(-9.63122777596328,-0.5778400902944,3.48493954146394));
#26657=CARTESIAN_POINT('Ctrl Pts',(-8.62408505598824,-1.26429202730363,
3.53266156491879));
#26658=CARTESIAN_POINT('Ctrl Pts',(-7.69266333517091,-0.866912531215043,
3.57242991779785));
#26659=CARTESIAN_POINT('Ctrl Pts',(-7.39991238656605,-0.189032694070974,
3.60424460010109));
#26660=CARTESIAN_POINT('Ctrl Pts',(-7.4495866441596,0.547687510380818,3.63605928240433));
#26661=CARTESIAN_POINT('Ctrl Pts',(-8.19493168629539,1.23319291086082,3.67582763528338));
#26662=CARTESIAN_POINT('Ctrl Pts',(-9.37345025199584,0.922312370267252,
3.72354965873824));
#26663=CARTESIAN_POINT('Ctrl Pts',(-9.74735766565093,-0.235292579725254,
3.77127168219311));
#26664=CARTESIAN_POINT('Ctrl Pts',(-8.97742616722564,-1.17713198321507,
3.81899370564797));
#26665=CARTESIAN_POINT('Ctrl Pts',(-7.76664010375505,-1.03731128115117,
3.86671572910283));
#26666=CARTESIAN_POINT('Ctrl Pts',(-7.32224636513591,-0.127382113028792,
3.90648408198189));
#26667=CARTESIAN_POINT('Ctrl Pts',(-7.5443749810873,0.576807541461097,3.93829876428512));
#26668=CARTESIAN_POINT('Ctrl Pts',(-8.06396180868744,1.10145382239662,3.97011344658837));
#26669=CARTESIAN_POINT('Ctrl Pts',(-9.07614321007789,1.13220600285683,4.00988179946742));
#26670=CARTESIAN_POINT('Ctrl Pts',(-9.76399920197892,0.126021698354871,
4.05760382292229));
#26671=CARTESIAN_POINT('Ctrl Pts',(-9.28937139980207,-0.994060630598775,
4.10532584637714));
#26672=CARTESIAN_POINT('Ctrl Pts',(-8.09088247259194,-1.2025798517467,4.15304786983201));
#26673=CARTESIAN_POINT('Ctrl Pts',(-7.26670323063882,-0.304648174304674,
4.20076989328686));
#26674=CARTESIAN_POINT('Ctrl Pts',(-7.52597647054109,0.674246239304052,
4.24053824616593));
#26675=CARTESIAN_POINT('Ctrl Pts',(-8.15469842594599,1.06145793115607,4.27235292846916));
#26676=CARTESIAN_POINT('Ctrl Pts',(-8.89090269571564,1.1182687108372,4.30416761077241));
#26677=CARTESIAN_POINT('Ctrl Pts',(-9.67648874516065,0.479276187531012,
4.34393596365146));
#26678=CARTESIAN_POINT('Ctrl Pts',(-9.53835693531735,-0.731703714585315,
4.39165798710632));
#26679=CARTESIAN_POINT('Ctrl Pts',(-8.44657181882848,-1.26823072569175,
4.43938001056118));
#26680=CARTESIAN_POINT('Ctrl Pts',(-7.40378085558735,-0.641778028981052,
4.48710203401604));
#26681=CARTESIAN_POINT('Ctrl Pts',(-7.36799034216343,0.576528894322393,
4.53482405747091));
#26682=CARTESIAN_POINT('Ctrl Pts',(-8.2045365779891,1.14718402769951,4.57459241034995));
#26683=CARTESIAN_POINT('Ctrl Pts',(-8.93335409498056,1.0286546286397,4.6064070926532));
#26684=CARTESIAN_POINT('Ctrl Pts',(-9.52728111459864,0.589935029256832,
4.63822177495644));
#26685=CARTESIAN_POINT('Ctrl Pts',(-9.70330383013366,-0.407297586304579,
4.67799012783549));
#26686=CARTESIAN_POINT('Ctrl Pts',(-8.80652255850025,-1.23272842596821,
4.72571215129035));
#26687=CARTESIAN_POINT('Ctrl Pts',(-7.62981812135516,-0.924146764431953,
4.77343417474522));
#26688=CARTESIAN_POINT('Ctrl Pts',(-7.25107879140469,0.2318863208135,4.82115619820008));
#26689=CARTESIAN_POINT('Ctrl Pts',(-8.02112464411643,1.17665195574191,4.86887822165494));
#26690=CARTESIAN_POINT('Ctrl Pts',(-9.02713314147116,1.06087722113259,4.90864657453399));
#26691=CARTESIAN_POINT('Ctrl Pts',(-9.50075252065141,0.494389026039362,
4.94046125683723));
#26692=CARTESIAN_POINT('Ctrl Pts',(-9.66286681237104,-0.225988061280402,
4.97227593914048));
#26693=CARTESIAN_POINT('Ctrl Pts',(-9.14351628915378,-1.09531649171262,
5.01204429201953));
#26694=CARTESIAN_POINT('Ctrl Pts',(-7.92526047005516,-1.13280621633993,
5.05976631547439));
#26695=CARTESIAN_POINT('Ctrl Pts',(-7.23727231077356,-0.129547392844347,
5.10748833892925));
#26696=CARTESIAN_POINT('Ctrl Pts',(-7.70721752222633,0.992507629187124,
5.15521036238412));
#26697=CARTESIAN_POINT('Ctrl Pts',(-8.90770750181304,1.20316500297725,5.20293238583897));
#26698=CARTESIAN_POINT('Ctrl Pts',(-9.59275579921949,0.45739981463423,5.24270073871803));
#26699=CARTESIAN_POINT('Ctrl Pts',(-9.58029073858244,-0.280887943477999,
5.27451542102127));
#26700=CARTESIAN_POINT('Ctrl Pts',(-9.23156266180433,-0.931743472748283,
5.30633010332451));
#26701=CARTESIAN_POINT('Ctrl Pts',(-8.2700188308547,-1.24937588149542,5.34609845620357));
#26702=CARTESIAN_POINT('Ctrl Pts',(-7.32418008556689,-0.480648499302866,
5.39382047965842));
#26703=CARTESIAN_POINT('Ctrl Pts',(-7.460297862814,0.728205472420246,5.44154250311328));
#26704=CARTESIAN_POINT('Ctrl Pts',(-8.54983244603065,1.26928805965479,5.48926452656816));
#26705=CARTESIAN_POINT('Ctrl Pts',(-9.59553565999399,0.64314310157645,5.53698655002299));
#26706=CARTESIAN_POINT('Ctrl Pts',(-9.62566726192722,-0.369056963869468,
5.57675490290208));
#26707=CARTESIAN_POINT('Ctrl Pts',(-9.13319439575196,-0.919233905949193,
5.6085695852053));
#26708=CARTESIAN_POINT('Ctrl Pts',(-8.4436265719743,-1.18328012903449,5.64038426750855));
#26709=CARTESIAN_POINT('Ctrl Pts',(-7.50863566519058,-0.794372826254617,
5.6801526203876));
#26710=CARTESIAN_POINT('Ctrl Pts',(-7.2963041006504,0.40582216911912,5.72787464384246));
#26711=CARTESIAN_POINT('Ctrl Pts',(-8.19017130198736,1.23096300595092,5.77559666729732));
#26712=CARTESIAN_POINT('Ctrl Pts',(-9.36815438333627,0.927298990484527,
5.82331869075219));
#26713=CARTESIAN_POINT('Ctrl Pts',(-9.74929745946807,-0.23040679067796,
5.87104071420704));
#26714=CARTESIAN_POINT('Ctrl Pts',(-9.10982341009197,-1.01560092342369,
5.91080906708611));
#26715=CARTESIAN_POINT('Ctrl Pts',(-8.37741999008716,-1.10945944397624,
5.94262374938933));
#26716=CARTESIAN_POINT('Ctrl Pts',(-7.68317215392635,-0.857975580674617,
5.97443843169259));
#26717=CARTESIAN_POINT('Ctrl Pts',(-7.23053602901599,0.0478817062916687,
6.01420678457163));
#26718=CARTESIAN_POINT('Ctrl Pts',(-7.85522187282586,1.0944572251931,6.0619288080265));
#26719=CARTESIAN_POINT('Ctrl Pts',(-9.07108417384462,1.13363424900455,6.10965083148136));
#26720=CARTESIAN_POINT('Ctrl Pts',(-9.76325682424838,0.13325782172002,6.15737285493622));
#26721=CARTESIAN_POINT('Ctrl Pts',(-9.29403504413602,-0.991634902626839,
6.20509487839108));
#26722=CARTESIAN_POINT('Ctrl Pts',(-8.29669469572309,-1.16704617749604,
6.24486323127014));
#26723=CARTESIAN_POINT('Ctrl Pts',(-7.68140252519118,-0.758830871074005,
6.27667791357338));
#26724=CARTESIAN_POINT('Ctrl Pts',(-7.32091588622009,-0.114413634620499,
6.30849259587662));
#26725=CARTESIAN_POINT('Ctrl Pts',(-7.57129164808408,0.86679422500701,6.34826094875567));
#26726=CARTESIAN_POINT('Ctrl Pts',(-8.72846469997545,1.24955165236365,6.39598297221053));
#26727=CARTESIAN_POINT('Ctrl Pts',(-9.67359730356846,0.483666324224417,
6.4437049956654));
#26728=CARTESIAN_POINT('Ctrl Pts',(-9.54252995272924,-0.725745650157118,
6.49142701912026));
#26729=CARTESIAN_POINT('Ctrl Pts',(-8.45168581803811,-1.26944758507204,
6.53914904257512));
#26730=CARTESIAN_POINT('Ctrl Pts',(-7.58267596702233,-0.749564170486322,
6.57891739545417));
#26731=CARTESIAN_POINT('Ctrl Pts',(-7.38444589289304,-0.0382772879798582,
6.61073207775742));
#26732=CARTESIAN_POINT('Ctrl Pts',(-7.53345529358936,0.684924198480989,
6.64254676006065));
#26733=CARTESIAN_POINT('Ctrl Pts',(-8.36478642108454,1.2631503154814,6.68231511293971));
#26734=CARTESIAN_POINT('Ctrl Pts',(-9.49033250313942,0.795497947379644,
6.73003713639457));
#26735=CARTESIAN_POINT('Ctrl Pts',(-9.70398954175645,-0.402085721548271,
6.77775915984943));
#26736=CARTESIAN_POINT('Ctrl Pts',(-8.81357665277965,-1.23095293731772,
6.8254811833043));
#26737=CARTESIAN_POINT('Ctrl Pts',(-7.63288943478823,-0.928413000297835,
6.87320320675915));
#26738=CARTESIAN_POINT('Ctrl Pts',(-7.31584661237576,0.0333253917197164,
6.91297155963821));
#26739=CARTESIAN_POINT('Ctrl Pts',(-7.63131447932525,0.700936218801929,
6.94478624194145));
#26740=CARTESIAN_POINT('Ctrl Pts',(-8.21717882643293,1.15036603345952,6.97660092424469));
#26741=CARTESIAN_POINT('Ctrl Pts',(-9.22419691584206,1.04372901584115,7.01636927712374));
#26742=CARTESIAN_POINT('Ctrl Pts',(-9.76941978790048,-0.0463557239862788,
7.06409130057861));
#26743=CARTESIAN_POINT('Ctrl Pts',(-9.14744487412929,-1.0918236483497,7.11181332403347));
#26744=CARTESIAN_POINT('Ctrl Pts',(-7.93175681708765,-1.1360788423931,7.15953534748832));
#26745=CARTESIAN_POINT('Ctrl Pts',(-7.2368036935283,-0.134783243543619,
7.2072573709432));
#26746=CARTESIAN_POINT('Ctrl Pts',(-7.62628417013839,0.799969046778991,
7.24702572382224));
#26747=CARTESIAN_POINT('Ctrl Pts',(-8.3016614880762,1.09844797389141,7.2788404061255));
#26748=CARTESIAN_POINT('Ctrl Pts',(-9.03877580315234,1.05501206679962,7.31065508842871));
#26749=CARTESIAN_POINT('Ctrl Pts',(-9.73056622357639,0.315496752466419,
7.35042344130779));
#26750=CARTESIAN_POINT('Ctrl Pts',(-9.42967335637867,-0.865611287760983,
7.39814546476263));
#26751=CARTESIAN_POINT('Ctrl Pts',(-8.27527513009739,-1.24930479746904,
7.44586748821751));
#26752=CARTESIAN_POINT('Ctrl Pts',(-7.3269517593169,-0.487373856592538,
7.49358951167236));
#26753=CARTESIAN_POINT('Ctrl Pts',(-7.45651776268534,0.724552449331778,
7.54131153512723));
#26754=CARTESIAN_POINT('Ctrl Pts',(-8.36265239254167,1.1766331041921,7.58107988800629));
#26755=CARTESIAN_POINT('Ctrl Pts',(-9.06869720420805,0.960473636589914,
7.61289457030951));
#26756=CARTESIAN_POINT('Ctrl Pts',(-9.59772315388831,0.445346723994618,
7.64470925261277));
#26757=CARTESIAN_POINT('Ctrl Pts',(-9.63704266960617,-0.566538082496456,
7.68447760549181));
#26758=CARTESIAN_POINT('Ctrl Pts',(-8.63671733765756,-1.26288709734616,
7.73219962894668));
#26759=CARTESIAN_POINT('Ctrl Pts',(-7.51265726772717,-0.797758154555581,
7.77992165240153));
#26760=CARTESIAN_POINT('Ctrl Pts',(-7.29399992857171,0.398922647608031,
7.82764367585641));
#26761=CARTESIAN_POINT('Ctrl Pts',(-8.18492249268409,1.23067363496886,7.87536569931125));
#26762=CARTESIAN_POINT('Ctrl Pts',(-9.16597666144441,0.979696337426352,
7.91513405219033));
#26763=CARTESIAN_POINT('Ctrl Pts',(-9.55849681005219,0.354274780033274,
7.94694873449355));
#26764=CARTESIAN_POINT('Ctrl Pts',(-9.62153775717122,-0.381422189174436,
7.9787634167968));
#26765=CARTESIAN_POINT('Ctrl Pts',(-8.98921836539449,-1.17238936466715,
8.01853176967584));
#26766=CARTESIAN_POINT('Ctrl Pts',(-7.7771125247792,-1.04451383390958,8.06625379313071));
#26767=CARTESIAN_POINT('Ctrl Pts',(-7.23136243031766,0.0426902907278673,
8.11397581658558));
#26768=CARTESIAN_POINT('Ctrl Pts',(-7.84896512350466,1.09074701037696,8.16169784004043));
#26769=CARTESIAN_POINT('Ctrl Pts',(-9.06692541504432,1.13684959656092,8.20941986349531));
#26770=CARTESIAN_POINT('Ctrl Pts',(-9.64464173069743,0.305164112407195,
8.24918821637434));
#26771=CARTESIAN_POINT('Ctrl Pts',(-9.5322862505581,-0.424630679022379,
8.2810028986776));
#26772=CARTESIAN_POINT('Ctrl Pts',(-9.09861015205532,-1.0222503181763,8.31281758098083));
#26773=CARTESIAN_POINT('Ctrl Pts',(-8.10290335699141,-1.20670861749438,
8.35258593385989));
#26774=CARTESIAN_POINT('Ctrl Pts',(-7.26991055531728,-0.316947013142206,
8.40030795731474));
#26775=CARTESIAN_POINT('Ctrl Pts',(-7.56851998300448,0.862327502791123,
8.44802998076961));
#26776=CARTESIAN_POINT('Ctrl Pts',(-8.72130549715427,1.25083944932549,8.49575200422448));
#26777=CARTESIAN_POINT('Ctrl Pts',(-9.67255596256759,0.488818929738847,
8.54347402767932));
#26778=CARTESIAN_POINT('Ctrl Pts',(-9.56530155789297,-0.518133590791118,
8.58324238055841));
#26779=CARTESIAN_POINT('Ctrl Pts',(-9.0028429994127,-0.996531502060991,
8.61505706286162));
#26780=CARTESIAN_POINT('Ctrl Pts',(-8.28386407323049,-1.16473820591356,
8.64687174516488));
#26781=CARTESIAN_POINT('Ctrl Pts',(-7.41017032490435,-0.652765433141797,
8.68664009804392));
#26782=CARTESIAN_POINT('Ctrl Pts',(-7.36236902101554,0.56512937166147,8.73436212149877));
#26783=CARTESIAN_POINT('Ctrl Pts',(-8.35976785794315,1.26158578402979,8.78208414495366));
#26784=CARTESIAN_POINT('Ctrl Pts',(-9.48576091064866,0.801155963652941,
8.8298061684085));
#26785=CARTESIAN_POINT('Ctrl Pts',(-9.70657326537737,-0.397507719045183,
8.87752819186338));
#26786=CARTESIAN_POINT('Ctrl Pts',(-8.96663395036875,-1.0888446094455,8.91729654474242));
#26787=CARTESIAN_POINT('Ctrl Pts',(-8.22826712547428,-1.0826298358905,8.94911122704566));
#26788=CARTESIAN_POINT('Ctrl Pts',(-7.57448282332976,-0.73942395338778,
8.98092590934891));
#26789=CARTESIAN_POINT('Ctrl Pts',(-7.24872202178017,0.219396564799815,
9.02069426222796));
#26790=CARTESIAN_POINT('Ctrl Pts',(-8.00941503387016,1.17170894084964,9.06841628568281));
#26791=CARTESIAN_POINT('Ctrl Pts',(-9.2193779708416,1.04582937384631,9.1161383091377));
#26792=CARTESIAN_POINT('Ctrl Pts',(-9.76966442671916,-0.0390857337594308,
9.16386033259253));
#26793=CARTESIAN_POINT('Ctrl Pts',(-9.15239411426545,-1.09005199467533,
9.21158235604742));
#26794=CARTESIAN_POINT('Ctrl Pts',(-8.14048539099326,-1.12875111209956,
9.25135070892645));
#26795=CARTESIAN_POINT('Ctrl Pts',(-7.58615922326735,-0.640953314554951,
9.2831653912297));
#26796=CARTESIAN_POINT('Ctrl Pts',(-7.316285050622,0.0463545658407663,9.31498007353294));
#26797=CARTESIAN_POINT('Ctrl Pts',(-7.69726342320074,0.98460419443171,9.35474842641199));
#26798=CARTESIAN_POINT('Ctrl Pts',(-8.895617959699,1.20708818278666,9.40247044986686));
#26799=CARTESIAN_POINT('Ctrl Pts',(-9.72829610040157,0.320238089349479,
9.45019247332171));
#26800=CARTESIAN_POINT('Ctrl Pts',(-9.43461496670731,-0.860273395535559,
9.49791449677658));
#26801=CARTESIAN_POINT('Ctrl Pts',(-8.28017716505078,-1.25120316202397,
9.54563652023144));
#26802=CARTESIAN_POINT('Ctrl Pts',(-7.4895978159432,-0.618398943731734,
9.58540487311049));
#26803=CARTESIAN_POINT('Ctrl Pts',(-7.38954263082771,0.113183691003795,
9.61721955541374));
#26804=CARTESIAN_POINT('Ctrl Pts',(-7.63514045459009,0.809535542066336,
9.64903423771697));
#26805=CARTESIAN_POINT('Ctrl Pts',(-8.537133574773,1.26982381811355,9.68880259059603));
#26806=CARTESIAN_POINT('Ctrl Pts',(-9.58895975750512,0.654019951984606,
9.7365246140509));
#26807=CARTESIAN_POINT('Ctrl Pts',(-9.6384280382287,-0.561467136978377,
9.78424663750574));
#26808=CARTESIAN_POINT('Ctrl Pts',(-8.64394691727858,-1.26208349013273,
9.83196866096063));
#26809=CARTESIAN_POINT('Ctrl Pts',(-7.51512238801277,-0.802401097226443,
9.87969068441545));
#26810=CARTESIAN_POINT('Ctrl Pts',(-7.33127459545891,0.193418602868329,
9.91945903729455));
#26811=CARTESIAN_POINT('Ctrl Pts',(-7.73426663122311,0.812144398860134,
9.95127371959776));
#26812=CARTESIAN_POINT('Ctrl Pts',(-8.37560914334392,1.17807331772501,9.98308840190104));
#26813=CARTESIAN_POINT('Ctrl Pts',(-9.35890135525045,0.936012763466847,
10.02285675478));
#26814=CARTESIAN_POINT('Ctrl Pts',(-9.75144090539661,-0.217878662011005,
10.0705787782349));
#26815=CARTESIAN_POINT('Ctrl Pts',(-8.99358386781122,-1.16946086277756,
10.1183008016898));
#26816=CARTESIAN_POINT('Ctrl Pts',(-7.78310570163958,-1.04863626488784,
10.1660228251447));
#26817=CARTESIAN_POINT('Ctrl Pts',(-7.23018890616732,0.0375661736589278,
10.2137448485995));
#26818=CARTESIAN_POINT('Ctrl Pts',(-7.74269724808928,0.910945865078545,
10.2535132014786));
#26819=CARTESIAN_POINT('Ctrl Pts',(-8.45228056360055,1.11519010578825,10.2853278837818));
#26820=CARTESIAN_POINT('Ctrl Pts',(-9.17671754862795,0.972308174672121,
10.317142566085));
#26821=CARTESIAN_POINT('Ctrl Pts',(-9.76196042907608,0.145901702765871,
10.3569109189641));
#26822=CARTESIAN_POINT('Ctrl Pts',(-9.30385292282665,-0.983562875225906,
10.404632942419));
#26823=CARTESIAN_POINT('Ctrl Pts',(-8.10812083976582,-1.20735018445606,
10.4523549658738));
#26824=CARTESIAN_POINT('Ctrl Pts',(-7.27174569549875,-0.323985824587662,
10.5000769893287));
#26825=CARTESIAN_POINT('Ctrl Pts',(-7.56427989964802,0.859220184365555,
10.5477990127836));
#26826=CARTESIAN_POINT('Ctrl Pts',(-8.5232999629678,1.1843930677275,10.5875673656626));
#26827=CARTESIAN_POINT('Ctrl Pts',(-9.19355740431409,0.87458804221152,10.6193820479658));
#26828=CARTESIAN_POINT('Ctrl Pts',(-9.64793064309135,0.292549253643142,
10.6511967302691));
#26829=CARTESIAN_POINT('Ctrl Pts',(-9.54982217450754,-0.715335469088547,
10.6909650831482));
#26830=CARTESIAN_POINT('Ctrl Pts',(-8.4643919788304,-1.26976671868812,10.738687106603));
#26831=CARTESIAN_POINT('Ctrl Pts',(-7.41369629983366,-0.656664309321609,
10.7864091300579));
#26832=CARTESIAN_POINT('Ctrl Pts',(-7.35915150586694,0.558605553583151,
10.8341311535127));
#26833=CARTESIAN_POINT('Ctrl Pts',(-8.35452822785808,1.26201006134411,10.8818531769676));
#26834=CARTESIAN_POINT('Ctrl Pts',(-9.29254410063642,0.880456515508654,
10.9216215298466));
#26835=CARTESIAN_POINT('Ctrl Pts',(-9.59672961639489,0.207630116265999,
10.9534362121499));
#26836=CARTESIAN_POINT('Ctrl Pts',(-9.55953517254716,-0.529825485693832,
10.9852508944531));
#26837=CARTESIAN_POINT('Ctrl Pts',(-8.82590258181982,-1.22785135036252,
11.0250192473322));
#26838=CARTESIAN_POINT('Ctrl Pts',(-7.64228970867862,-0.936967719412468,
11.072741270787));
#26839=CARTESIAN_POINT('Ctrl Pts',(-7.2488375995026,0.214141055646775,11.1204632942419));
#26840=CARTESIAN_POINT('Ctrl Pts',(-8.00271338065867,1.16888043412647,11.1681853176968));
#26841=CARTESIAN_POINT('Ctrl Pts',(-9.21569307889762,1.04957841452743,11.2159073411516));
#26842=CARTESIAN_POINT('Ctrl Pts',(-9.67542825259376,0.147303259161649,
11.2556756940307));
#26843=CARTESIAN_POINT('Ctrl Pts',(-9.46525342395248,-0.560546112470954,
11.2874903763339));
#26844=CARTESIAN_POINT('Ctrl Pts',(-8.95462334184431,-1.09391381936859,
11.3193050586371));
#26845=CARTESIAN_POINT('Ctrl Pts',(-7.94310764484011,-1.14179785259405,
11.3590734115162));
#26846=CARTESIAN_POINT('Ctrl Pts',(-7.23831550942318,-0.147403179400998,
11.406795434971));
#26847=CARTESIAN_POINT('Ctrl Pts',(-7.6939122603442,0.98055407811529,11.4545174584259));
#26848=CARTESIAN_POINT('Ctrl Pts',(-8.88869917985897,1.20933386566182,11.5022394818808));
#26849=CARTESIAN_POINT('Ctrl Pts',(-9.72796230694971,0.325484260963068,
11.5499615053357));
#26850=CARTESIAN_POINT('Ctrl Pts',(-9.48529893752489,-0.65765935777389,
11.5897298582147));
#26851=CARTESIAN_POINT('Ctrl Pts',(-8.86322259765864,-1.05545983401,11.621544540518));
#26852=CARTESIAN_POINT('Ctrl Pts',(-8.12808565118239,-1.12472643087056,
11.6533592228212));
#26853=CARTESIAN_POINT('Ctrl Pts',(-7.33179403263406,-0.499125484457065,
11.6931275757003));
#26854=CARTESIAN_POINT('Ctrl Pts',(-7.44940412037606,0.714019431652113,
11.7408495991551));
#26855=CARTESIAN_POINT('Ctrl Pts',(-8.53194934097467,1.26895349944086,11.78857162261));
#26856=CARTESIAN_POINT('Ctrl Pts',(-9.58519671026048,0.660245068970213,
11.8362936460648));
#26857=CARTESIAN_POINT('Ctrl Pts',(-9.64160806535992,-0.557281308253744,
11.8840156695197));
#26858=CARTESIAN_POINT('Ctrl Pts',(-8.81484293386192,-1.1420174053632,11.9237840223988));
#26859=CARTESIAN_POINT('Ctrl Pts',(-8.08412316719659,-1.03584389586256,
11.955598704702));
#26860=CARTESIAN_POINT('Ctrl Pts',(-7.48285373565609,-0.607242376721559,
11.9874133870052));
#26861=CARTESIAN_POINT('Ctrl Pts',(-7.28997307136937,0.386867242620354,
12.0271817398843));
#26862=CARTESIAN_POINT('Ctrl Pts',(-8.17265124555415,1.22736231163514,12.0749037633391));
#26863=CARTESIAN_POINT('Ctrl Pts',(-9.35441133005812,0.938746517010956,
12.122625786794));
#26864=CARTESIAN_POINT('Ctrl Pts',(-9.75266805128835,-0.210708814103916,
12.1703478102489));
#26865=CARTESIAN_POINT('Ctrl Pts',(-8.99872747341793,-1.16837594064669,
12.2180698337037));
#26866=CARTESIAN_POINT('Ctrl Pts',(-7.99090309083843,-1.06964955206712,
12.2578381865828));
#26867=CARTESIAN_POINT('Ctrl Pts',(-7.50776093085483,-0.511260937604508,
12.289652868886));
#26868=CARTESIAN_POINT('Ctrl Pts',(-7.3334738690475,0.206268303333894,12.3214675511893));
#26869=CARTESIAN_POINT('Ctrl Pts',(-7.83803220192628,1.08426475813674,12.3612359040683));
#26870=CARTESIAN_POINT('Ctrl Pts',(-9.05547871457524,1.14237421570755,12.4089579275232));
#26871=CARTESIAN_POINT('Ctrl Pts',(-9.76035346995239,0.15090684182913,12.456679950978));
#26872=CARTESIAN_POINT('Ctrl Pts',(-9.30947203638216,-0.978943549636521,
12.5044019744329));
#26873=CARTESIAN_POINT('Ctrl Pts',(-8.11272055027382,-1.20989506125271,
12.5521239978878));
#26874=CARTESIAN_POINT('Ctrl Pts',(-7.41514461007779,-0.475834645766756,
12.5918923507668));
#26875=CARTESIAN_POINT('Ctrl Pts',(-7.4151086511821,0.262558332410862,12.6237070330701));
#26876=CARTESIAN_POINT('Ctrl Pts',(-7.75276774428468,0.919224555358408,
12.6555217153733));
#26877=CARTESIAN_POINT('Ctrl Pts',(-8.70879623786288,1.25309040475067,12.6952900682523));
#26878=CARTESIAN_POINT('Ctrl Pts',(-9.66751399921959,0.500486276221317,
12.7430120917072));
#26879=CARTESIAN_POINT('Ctrl Pts',(-9.55188166335335,-0.710498916559987,
12.7907341151621));
#26880=CARTESIAN_POINT('Ctrl Pts',(-8.47166377950834,-1.26994980596394,
12.8384561386169));
#26881=CARTESIAN_POINT('Ctrl Pts',(-7.41550978691736,-0.661598374508149,
12.8861781620718));
#26882=CARTESIAN_POINT('Ctrl Pts',(-7.3682459272926,0.349946490288843,12.9259465149509));
#26883=CARTESIAN_POINT('Ctrl Pts',(-7.85133369920765,0.908382159046878,
12.9577611972541));
#26884=CARTESIAN_POINT('Ctrl Pts',(-8.53633238175378,1.18406494128969,12.9895758795573));
#26885=CARTESIAN_POINT('Ctrl Pts',(-9.47777349447388,0.811042800922508,
13.0293442324364));
#26886=CARTESIAN_POINT('Ctrl Pts',(-9.71039396279849,-0.385385399153313,
13.0770662558912));
#26887=CARTESIAN_POINT('Ctrl Pts',(-8.83062453150002,-1.22554117160637,
13.1247882793461));
#26888=CARTESIAN_POINT('Ctrl Pts',(-7.64766924194114,-0.941863965722445,
13.172510302801));
#26889=CARTESIAN_POINT('Ctrl Pts',(-7.24698080025217,0.209223126081278,
13.2202323262558));
#26890=CARTESIAN_POINT('Ctrl Pts',(-7.87306983888273,1.00513103635134,13.2600006791349));
#26891=CARTESIAN_POINT('Ctrl Pts',(-8.60377926102454,1.11137571578629,13.2918153614381));
#26892=CARTESIAN_POINT('Ctrl Pts',(-9.30218522440413,0.871681531812472,
13.3236300437414));
#26893=CARTESIAN_POINT('Ctrl Pts',(-9.77009266600105,-0.0263827821550767,
13.3633983966204));
#26894=CARTESIAN_POINT('Ctrl Pts',(-9.16321490783652,-1.08338425181604,
13.4111204200753));
#26895=CARTESIAN_POINT('Ctrl Pts',(-7.94819013624447,-1.14314024441186,
13.4588424435301));
#26896=CARTESIAN_POINT('Ctrl Pts',(-7.2391802885307,-0.154625697185406,
13.506564466985));
#26897=CARTESIAN_POINT('Ctrl Pts',(-7.68929035206307,0.978049742173603,
13.5542864904399));
#26898=CARTESIAN_POINT('Ctrl Pts',(-8.68351804052399,1.17032087734838,13.5940548433189));
#26899=CARTESIAN_POINT('Ctrl Pts',(-9.30563312229838,0.772580991815164,
13.6258695256222));
#26900=CARTESIAN_POINT('Ctrl Pts',(-9.67697809753389,0.134359164483624,
13.6576842079254));
#26901=CARTESIAN_POINT('Ctrl Pts',(-9.44325009763995,-0.85094693414226,
13.6974525608044));
#26902=CARTESIAN_POINT('Ctrl Pts',(-8.2927229897676,-1.25324047656015,13.7451745842593));
#26903=CARTESIAN_POINT('Ctrl Pts',(-7.33475938495617,-0.503466039752598,
13.7928966077142));
#26904=CARTESIAN_POINT('Ctrl Pts',(-7.44533257125672,0.707991571847893,
13.8406186311691));
#26905=CARTESIAN_POINT('Ctrl Pts',(-8.52681547325545,1.27008360426311,13.8883406546239));
#26906=CARTESIAN_POINT('Ctrl Pts',(-9.4045024161679,0.764987062832887,13.928109007503));
#26907=CARTESIAN_POINT('Ctrl Pts',(-9.61474618672592,0.0571581651064585,
13.9599236898062));
#26908=CARTESIAN_POINT('Ctrl Pts',(-9.47800196452181,-0.668462403240976,
13.9917383721095));
#26909=CARTESIAN_POINT('Ctrl Pts',(-8.65657937087898,-1.2606801069419,14.0315067249885));
#26910=CARTESIAN_POINT('Ctrl Pts',(-7.52327723764377,-0.812150291851726,
14.0792287484434));
#26911=CARTESIAN_POINT('Ctrl Pts',(-7.28937569504537,0.381644515727654,
14.1269507718982));
#26912=CARTESIAN_POINT('Ctrl Pts',(-8.16562822136408,1.22546765143414,14.1746727953531));
#26913=CARTESIAN_POINT('Ctrl Pts',(-9.35126822931952,0.942960144001402,
14.2223948188079));
#26914=CARTESIAN_POINT('Ctrl Pts',(-9.68454787080297,-0.0132728644732055,
14.262163171687));
#26915=CARTESIAN_POINT('Ctrl Pts',(-9.38042788824344,-0.686128887499729,
14.2939778539902));
#26916=CARTESIAN_POINT('Ctrl Pts',(-8.80225636879473,-1.14541298869798,
14.3257925362935));
#26917=CARTESIAN_POINT('Ctrl Pts',(-7.7935772406708,-1.05584009988523,14.3655608891725));
#26918=CARTESIAN_POINT('Ctrl Pts',(-7.22997734567405,0.0248577665794866,
14.4132829126274));
#26919=CARTESIAN_POINT('Ctrl Pts',(-7.83416331394744,1.08070590432209,14.4610049360822));
#26920=CARTESIAN_POINT('Ctrl Pts',(-9.04892789296556,1.14553638937609,14.5087269595371));
#26921=CARTESIAN_POINT('Ctrl Pts',(-9.76073337693308,0.156149875811182,
14.556448982992));
#26922=CARTESIAN_POINT('Ctrl Pts',(-9.3871341050952,-0.785062358491584,
14.596217335871));
#26923=CARTESIAN_POINT('Ctrl Pts',(-8.71690684123967,-1.09493266409088,
14.6280320181743));
#26924=CARTESIAN_POINT('Ctrl Pts',(-7.97916280057658,-1.06398234893415,
14.6598467004775));
#26925=CARTESIAN_POINT('Ctrl Pts',(-7.27495151425187,-0.336285056074748,
14.6996150533566));
#26926=CARTESIAN_POINT('Ctrl Pts',(-7.55580506332157,0.849747828921635,
14.7473370768114));
#26927=CARTESIAN_POINT('Ctrl Pts',(-8.70354189550648,1.25293034154821,14.7950591002663));
#26928=CARTESIAN_POINT('Ctrl Pts',(-9.66462886206689,0.50716374522088,14.8427811237211));
#26929=CARTESIAN_POINT('Ctrl Pts',(-9.55559937622805,-0.706782420080516,
14.890503147176));
#26930=CARTESIAN_POINT('Ctrl Pts',(-8.65724835414967,-1.1741391659753,14.930271500055));
#26931=CARTESIAN_POINT('Ctrl Pts',(-7.94764515033822,-0.96996403905036,
14.9620861823583));
#26932=CARTESIAN_POINT('Ctrl Pts',(-7.40997390642474,-0.463867378652346,
14.9939008646615));
#26933=CARTESIAN_POINT('Ctrl Pts',(-7.35352879266581,0.547206716293156,
15.0336692175406));
#26934=CARTESIAN_POINT('Ctrl Pts',(-8.34192153595724,1.26039147291347,15.0813912409955));
#26935=CARTESIAN_POINT('Ctrl Pts',(-9.47369516602269,0.814359548927965,
15.1291132644503));
#26936=CARTESIAN_POINT('Ctrl Pts',(-9.71258097395429,-0.378447839289041,
15.1768352879052));
#26937=CARTESIAN_POINT('Ctrl Pts',(-8.83586773229483,-1.22516301435895,
15.2245573113601));
#26938=CARTESIAN_POINT('Ctrl Pts',(-7.85070500083801,-0.99083086753391,
15.2643256642391));
#26939=CARTESIAN_POINT('Ctrl Pts',(-7.44765287922776,-0.372144466768538,
15.2961403465424));
#26940=CARTESIAN_POINT('Ctrl Pts',(-7.3721652533645,0.362380053367863,15.3279550288456));
#26941=CARTESIAN_POINT('Ctrl Pts',(-7.99100368173551,1.16393843392934,15.3677233817246));
#26942=CARTESIAN_POINT('Ctrl Pts',(-9.20509935271424,1.05660333990528,15.4154454051795));
#26943=CARTESIAN_POINT('Ctrl Pts',(-9.7691800770222,-0.0212073876111575,
15.4631674286343));
#26944=CARTESIAN_POINT('Ctrl Pts',(-9.16940494659641,-1.07956620750791,
15.5108894520892));
#26945=CARTESIAN_POINT('Ctrl Pts',(-7.95240868713248,-1.14628955341283,
15.5586114755441));
#26946=CARTESIAN_POINT('Ctrl Pts',(-7.360678360457,-0.324490753397076,15.5983798284231));
#26947=CARTESIAN_POINT('Ctrl Pts',(-7.46068657418702,0.407081917027667,
15.6301945107264));
#26948=CARTESIAN_POINT('Ctrl Pts',(-7.88413511411916,1.01199674841518,15.6620091930296));
#26949=CARTESIAN_POINT('Ctrl Pts',(-8.87668188965118,1.21320028335118,15.7017775459087));
#26950=CARTESIAN_POINT('Ctrl Pts',(-9.72442683656734,0.33782473088057,15.7494995693635));
#26951=CARTESIAN_POINT('Ctrl Pts',(-9.44616547363274,-0.846612249150427,
15.7972215928184));
#26952=CARTESIAN_POINT('Ctrl Pts',(-8.29949020407744,-1.25407183081511,
15.8449436162733));
#26953=CARTESIAN_POINT('Ctrl Pts',(-7.33668119725462,-0.50924503049874,
15.8926656397281));
#26954=CARTESIAN_POINT('Ctrl Pts',(-7.44249701763682,0.703085044785891,
15.940387663183));
#26955=CARTESIAN_POINT('Ctrl Pts',(-8.51978535451018,1.26984600438471,15.9881096866378));
#26956=CARTESIAN_POINT('Ctrl Pts',(-9.57853041802029,0.669890693554712,
16.0358317100927));
#26957=CARTESIAN_POINT('Ctrl Pts',(-9.6473848859972,-0.544843601674845,
16.0835537335476));
#26958=CARTESIAN_POINT('Ctrl Pts',(-8.66080360141944,-1.2601136358619,16.1312757570025));
#26959=CARTESIAN_POINT('Ctrl Pts',(-7.71812331405291,-0.889997654174616,
16.1710441098815));
#26960=CARTESIAN_POINT('Ctrl Pts',(-7.40587711199952,-0.220869169870984,
16.2028587921847));
#26961=CARTESIAN_POINT('Ctrl Pts',(-7.43412333655584,0.516967103108417,
16.234673474488));
#26962=CARTESIAN_POINT('Ctrl Pts',(-8.15927934511513,1.22382409746097,16.274441827367));
#26963=CARTESIAN_POINT('Ctrl Pts',(-9.34631329395978,0.947269754287392,
16.3221638508219));
#26964=CARTESIAN_POINT('Ctrl Pts',(-9.75366233503884,-0.19899389665094,
16.3698858742767));
#26965=CARTESIAN_POINT('Ctrl Pts',(-9.01138473879162,-1.16278173533473,
16.4176078977316));
#26966=CARTESIAN_POINT('Ctrl Pts',(-7.79705255782462,-1.05815633227033,
16.4653299211865));
#26967=CARTESIAN_POINT('Ctrl Pts',(-7.32643878878709,-0.161507282602953,
16.5050982740655));
#26968=CARTESIAN_POINT('Ctrl Pts',(-7.5280384983639,0.548832220338187,16.5369129563688));
#26969=CARTESIAN_POINT('Ctrl Pts',(-8.03218094264503,1.08833594701741,16.568727638672));
#26970=CARTESIAN_POINT('Ctrl Pts',(-9.04304373573084,1.14844897424026,16.6084959915511));
#26971=CARTESIAN_POINT('Ctrl Pts',(-9.75980963534572,0.162650140327407,
16.6562180150059));
#26972=CARTESIAN_POINT('Ctrl Pts',(-9.31788680540282,-0.970734219451476,
16.7039400384608));
#26973=CARTESIAN_POINT('Ctrl Pts',(-8.12595390549439,-1.21394603873985,
16.7516620619157));
#26974=CARTESIAN_POINT('Ctrl Pts',(-7.2760636253747,-0.340310403120085,
16.7993840853705));
#26975=CARTESIAN_POINT('Ctrl Pts',(-7.50681993013901,0.645695886996063,
16.8391524382496));
#26976=CARTESIAN_POINT('Ctrl Pts',(-8.12404011840559,1.05099014478124,16.8709671205528));
#26977=CARTESIAN_POINT('Ctrl Pts',(-8.85828565453448,1.12914180496286,16.902781802856));
#26978=CARTESIAN_POINT('Ctrl Pts',(-9.66208453803124,0.513216288611988,
16.9425501557351));
#26979=CARTESIAN_POINT('Ctrl Pts',(-9.55915380641066,-0.701262194326414,
16.9902721791899));
#26980=CARTESIAN_POINT('Ctrl Pts',(-8.48339865398978,-1.26924707575363,
17.0379942026449));
#26981=CARTESIAN_POINT('Ctrl Pts',(-7.42286709434953,-0.673320246815119,
17.0857162260997));
#26982=CARTESIAN_POINT('Ctrl Pts',(-7.35173612228207,0.543434907326658,
17.1334382495546));
#26983=CARTESIAN_POINT('Ctrl Pts',(-8.17136948899973,1.13812644920779,17.1732066024336));
#26984=CARTESIAN_POINT('Ctrl Pts',(-8.90331979515647,1.0407974152085,17.2050212847369));
#26985=CARTESIAN_POINT('Ctrl Pts',(-9.50972840593837,0.619498485377158,
17.23683596704));
#26986=CARTESIAN_POINT('Ctrl Pts',(-9.71461689321606,-0.372205902885845,
17.2766043199191));
#26987=CARTESIAN_POINT('Ctrl Pts',(-8.84216750674715,-1.22331387974914,
17.324326343374));
#26988=CARTESIAN_POINT('Ctrl Pts',(-7.65700356119952,-0.949010404737396,
17.3720483668289));
#26989=CARTESIAN_POINT('Ctrl Pts',(-7.2448754144411,0.195544689997025,17.4197703902837));
#26990=CARTESIAN_POINT('Ctrl Pts',(-7.98717963800152,1.16225931174747,17.4674924137386));
#26991=CARTESIAN_POINT('Ctrl Pts',(-8.99612423756339,1.07572792473616,17.5072607666176));
#26992=CARTESIAN_POINT('Ctrl Pts',(-9.48598375104783,0.52322285818574,17.5390754489209));
#26993=CARTESIAN_POINT('Ctrl Pts',(-9.66893526453526,-0.192146232024172,
17.5708901312241));
#26994=CARTESIAN_POINT('Ctrl Pts',(-9.17503157966931,-1.07618018838531,
17.6106584841032));
#26995=CARTESIAN_POINT('Ctrl Pts',(-7.9583768197333,-1.14900817301593,17.658380507558));
#26996=CARTESIAN_POINT('Ctrl Pts',(-7.24156363400886,-0.166137463815073,
17.7061025310129));
#26997=CARTESIAN_POINT('Ctrl Pts',(-7.67874863455965,0.969082889035782,
17.7538245544677));
#26998=CARTESIAN_POINT('Ctrl Pts',(-8.87261967454383,1.21449002036524,17.8015465779226));
#26999=CARTESIAN_POINT('Ctrl Pts',(-9.57902171510171,0.488919180943277,
17.8413149308017));
#27000=CARTESIAN_POINT('Ctrl Pts',(-9.58798717630628,-0.249419367434415,
17.8731296131049));
#27001=CARTESIAN_POINT('Ctrl Pts',(-9.2582939446597,-0.910120937374646,
17.9049442954082));
#27002=CARTESIAN_POINT('Ctrl Pts',(-8.30637285397506,-1.25552377904448,
17.9447126482872));
#27003=CARTESIAN_POINT('Ctrl Pts',(-7.33862383613528,-0.514568612593541,
17.9924346717421));
#27004=CARTESIAN_POINT('Ctrl Pts',(-7.4396030778627,0.697726387385249,18.0401566951969));
#27005=CARTESIAN_POINT('Ctrl Pts',(-8.51297644133385,1.27019961542661,18.0878787186518));
#27006=CARTESIAN_POINT('Ctrl Pts',(-9.57641009434339,0.674664909580691,
18.1356007421067));
#27007=CARTESIAN_POINT('Ctrl Pts',(-9.63590327239758,-0.336234416608025,
18.1753690949857));
#27008=CARTESIAN_POINT('Ctrl Pts',(-9.15960407852556,-0.900471307844259,
18.207183777289));
#27009=CARTESIAN_POINT('Ctrl Pts',(-8.47798936265341,-1.1844177299411,18.2389984595921));
#27010=CARTESIAN_POINT('Ctrl Pts',(-7.53210607607463,-0.822807865453571,
18.2787668124713));
#27011=CARTESIAN_POINT('Ctrl Pts',(-7.28503401962905,0.370719729176766,
18.326488835926));
#27012=CARTESIAN_POINT('Ctrl Pts',(-8.15457897907752,1.22145325839214,18.374210859381));
#27013=CARTESIAN_POINT('Ctrl Pts',(-9.34087831913538,0.952102464794442,
18.4219328828358));
#27014=CARTESIAN_POINT('Ctrl Pts',(-9.7554577416763,-0.194054864120685,
18.4696549062907));
#27015=CARTESIAN_POINT('Ctrl Pts',(-9.13903952802435,-0.997475969022656,
18.5094232591697));
#27016=CARTESIAN_POINT('Ctrl Pts',(-8.40966837294719,-1.11254946578222,
18.541237941473));
#27017=CARTESIAN_POINT('Ctrl Pts',(-7.70841482017917,-0.881318744974411,
18.5730526237762));
#27018=CARTESIAN_POINT('Ctrl Pts',(-7.22968115822663,0.011021418212948,
18.6128209766553));
#27019=CARTESIAN_POINT('Ctrl Pts',(-7.82373204986715,1.07528466495283,18.6605430001101));
#27020=CARTESIAN_POINT('Ctrl Pts',(-9.03794533402332,1.14972977770192,18.708265023565));
#27021=CARTESIAN_POINT('Ctrl Pts',(-9.75885760069877,0.169861685563808,
18.7559870470199));
#27022=CARTESIAN_POINT('Ctrl Pts',(-9.32247807753752,-0.968174180297135,
18.8037090704747));
#27023=CARTESIAN_POINT('Ctrl Pts',(-8.330648257652,-1.17245461085662,18.8434774233538));
#27024=CARTESIAN_POINT('Ctrl Pts',(-7.70376873565747,-0.782267147681539,
18.875292105657));
#27025=CARTESIAN_POINT('Ctrl Pts',(-7.32473279588695,-0.148582724741135,
18.9071067879603));
#27026=CARTESIAN_POINT('Ctrl Pts',(-7.54652823945384,0.839477833694785,
18.9468751408393));
#27027=CARTESIAN_POINT('Ctrl Pts',(-8.69210621464535,1.25565546761611,18.9945971642941));
#27028=CARTESIAN_POINT('Ctrl Pts',(-9.65906691117085,0.517520665829651,
19.0423191877491));
#27029=CARTESIAN_POINT('Ctrl Pts',(-9.56315216209578,-0.695185537314083,
19.0900412112039));
#27030=CARTESIAN_POINT('Ctrl Pts',(-8.48854581274214,-1.27031501330109,
19.1377632346588));
#27031=CARTESIAN_POINT('Ctrl Pts',(-7.60481483699583,-0.775869416263104,
19.1775315875378));
#27032=CARTESIAN_POINT('Ctrl Pts',(-7.38602655189909,-0.0706347901850005,
19.2093462698411));
#27033=CARTESIAN_POINT('Ctrl Pts',(-7.51398572855607,0.656586387053644,
19.2411609521443));
#27034=CARTESIAN_POINT('Ctrl Pts',(-8.32818647186491,1.25869438029001,19.2809293050234));
#27035=CARTESIAN_POINT('Ctrl Pts',(-9.4668298755767,0.823902568725164,19.3286513284782));
#27036=CARTESIAN_POINT('Ctrl Pts',(-9.71515106657892,-0.366976333738334,
19.3763733519331));
#27037=CARTESIAN_POINT('Ctrl Pts',(-8.84916710494986,-1.2213344275343,19.4240953753879));
#27038=CARTESIAN_POINT('Ctrl Pts',(-7.66019738816671,-0.953185713584651,
19.4718173988428));
#27039=CARTESIAN_POINT('Ctrl Pts',(-7.31537823830772,-0.0010530338523334,
19.5115857517218));
#27040=CARTESIAN_POINT('Ctrl Pts',(-7.61133902610286,0.675431558435419,
19.5434004340251));
#27041=CARTESIAN_POINT('Ctrl Pts',(-8.18391407035424,1.14167399560261,19.5752151163283));
#27042=CARTESIAN_POINT('Ctrl Pts',(-9.19360265821437,1.06430577558419,19.6149834692074));
#27043=CARTESIAN_POINT('Ctrl Pts',(-9.77023039295916,-0.00949736081626473,
19.6627054926622));
#27044=CARTESIAN_POINT('Ctrl Pts',(-9.1788571469454,-1.07257480772814,19.7104275161171));
#27045=CARTESIAN_POINT('Ctrl Pts',(-7.96496540298764,-1.15209089531139,
19.758149539572));
#27046=CARTESIAN_POINT('Ctrl Pts',(-7.24124715966354,-0.171384708678441,
19.8058715630268));
#27047=CARTESIAN_POINT('Ctrl Pts',(-7.60343688127647,0.77427669556818,19.8456399159059));
#27048=CARTESIAN_POINT('Ctrl Pts',(-8.26986782341272,1.09222950791374,19.8774545982091));
#27049=CARTESIAN_POINT('Ctrl Pts',(-9.00793220370274,1.0702031132439,19.9092692805124));
#27050=CARTESIAN_POINT('Ctrl Pts',(-9.72089215495525,0.351075173421066,
19.9490376333914));
#27051=CARTESIAN_POINT('Ctrl Pts',(-9.45440202947589,-0.838267390032476,
19.9967596568463));
#27052=CARTESIAN_POINT('Ctrl Pts',(-8.31162487652084,-1.25530018600577,
20.0444816803012));
#27053=CARTESIAN_POINT('Ctrl Pts',(-7.34158951386127,-0.521210702752235,
20.092203703756));
#27054=CARTESIAN_POINT('Ctrl Pts',(-7.43593058134585,0.693965203528907,
20.1399257272109));
#27055=CARTESIAN_POINT('Ctrl Pts',(-8.32856409047539,1.17215167793282,20.1796940800899));
#27056=CARTESIAN_POINT('Ctrl Pts',(-9.04058452848265,0.976572825867848,
20.2115087623932));
#27057=CARTESIAN_POINT('Ctrl Pts',(-9.58433676096464,0.477015320483459,
20.2433234446964));
#27058=CARTESIAN_POINT('Ctrl Pts',(-9.65300483419814,-0.533302244266452,
20.2830917975755));
#27059=CARTESIAN_POINT('Ctrl Pts',(-8.67330901488357,-1.25838763360885,
20.3308138210303));
#27060=CARTESIAN_POINT('Ctrl Pts',(-7.53622422777799,-0.826075060154805,
20.3785358444852));
#27061=CARTESIAN_POINT('Ctrl Pts',(-7.28293104363061,0.36375624599658,20.4262578679401));
#27062=CARTESIAN_POINT('Ctrl Pts',(-8.14934077805168,1.22101168769447,20.4739798913949));
#27063=CARTESIAN_POINT('Ctrl Pts',(-9.13726516704792,0.998610501658501,
20.5137482442739));
#27064=CARTESIAN_POINT('Ctrl Pts',(-9.54776986598246,0.384843376709829,
20.5455629265772));
#27065=CARTESIAN_POINT('Ctrl Pts',(-9.63213434842366,-0.348714273115681,
20.5773776088804));
#27066=CARTESIAN_POINT('Ctrl Pts',(-9.02303531396696,-1.15769835957703,
20.6171459617595));
#27067=CARTESIAN_POINT('Ctrl Pts',(-7.80772900649456,-1.06505226285407,
20.6648679852143));
#27068=CARTESIAN_POINT('Ctrl Pts',(-7.2306578674812,0.00585617149092387,
20.7125900086692));
#27069=CARTESIAN_POINT('Ctrl Pts',(-7.81758560697748,1.07139444055647,20.760312032124));
#27070=CARTESIAN_POINT('Ctrl Pts',(-9.03369501670135,1.15282308294553,20.8080340555789));
#27071=CARTESIAN_POINT('Ctrl Pts',(-9.63530370681369,0.33825333767807,20.847802408458));
#27072=CARTESIAN_POINT('Ctrl Pts',(-9.54417435213954,-0.394494662818509,
20.8796170907612));
#27073=CARTESIAN_POINT('Ctrl Pts',(-9.12802395962112,-1.00444797441034,
20.9114317730645));
#27074=CARTESIAN_POINT('Ctrl Pts',(-8.13808955169642,-1.21772421296146,
20.9512001259435));
#27075=CARTESIAN_POINT('Ctrl Pts',(-7.27962651001226,-0.352510987055423,
20.9989221493984));
#27076=CARTESIAN_POINT('Ctrl Pts',(-7.54388736698447,0.834932558426133,
21.0466441728532));
#27077=CARTESIAN_POINT('Ctrl Pts',(-8.68491265495414,1.25673496056146,21.0943661963081));
#27078=CARTESIAN_POINT('Ctrl Pts',(-9.65787647902049,0.522640881251166,
21.1420882197629));
#27079=CARTESIAN_POINT('Ctrl Pts',(-9.57988922915072,-0.487000082052889,
21.181856572642));
#27080=CARTESIAN_POINT('Ctrl Pts',(-9.03155077607419,-0.981519174093523,
21.2136712549453));
#27081=CARTESIAN_POINT('Ctrl Pts',(-8.31775606126076,-1.17051995879953,
21.2454859372485));
#27082=CARTESIAN_POINT('Ctrl Pts',(-7.42957272949752,-0.684117599531321,
21.2852542901276));
#27083=CARTESIAN_POINT('Ctrl Pts',(-7.34644798530079,0.531877053878988,
21.3329763135824));
#27084=CARTESIAN_POINT('Ctrl Pts',(-8.32321542546207,1.25698486798265,21.3806983370373));
#27085=CARTESIAN_POINT('Ctrl Pts',(-9.46209601166041,0.829425533370407,
21.4284203604922));
#27086=CARTESIAN_POINT('Ctrl Pts',(-9.71760084736768,-0.362325279153129,
21.476142383947));
#27087=CARTESIAN_POINT('Ctrl Pts',(-8.99803592390773,-1.07484419598965,
21.5159107368261));
#27088=CARTESIAN_POINT('Ctrl Pts',(-8.25979972674399,-1.09005960634547,
21.5477254191293));
#27089=CARTESIAN_POINT('Ctrl Pts',(-7.59633087273917,-0.765971236790843,
21.5795401014325));
#27090=CARTESIAN_POINT('Ctrl Pts',(-7.24288209287525,0.182991800390507,
21.6193084543116));
#27091=CARTESIAN_POINT('Ctrl Pts',(-7.97561840692373,1.15697856328559,21.6670304777664));
#27092=CARTESIAN_POINT('Ctrl Pts',(-9.18872478998646,1.06626540213497,21.7147525012213));
#27093=CARTESIAN_POINT('Ctrl Pts',(-9.77026395203898,-0.00222333305725054,
21.7624745246762));
#27094=CARTESIAN_POINT('Ctrl Pts',(-9.18375288880803,-1.07066027220149,
21.810196548131));
#27095=CARTESIAN_POINT('Ctrl Pts',(-8.17339341325626,-1.13870890250796,
21.8499649010101));
#27096=CARTESIAN_POINT('Ctrl Pts',(-7.60514471543686,-0.667203219677276,
21.8817795833133));
#27097=CARTESIAN_POINT('Ctrl Pts',(-7.31543838241809,0.011983376276968,
21.9135942656166));
#27098=CARTESIAN_POINT('Ctrl Pts',(-7.66902808735548,0.960893912885179,
21.9533626184956));
#27099=CARTESIAN_POINT('Ctrl Pts',(-8.86042137271117,1.21806070667787,22.0010846419505));
#27100=CARTESIAN_POINT('Ctrl Pts',(-9.71848539326896,0.355748633900504,
22.0488066654053));
#27101=CARTESIAN_POINT('Ctrl Pts',(-9.45918665172335,-0.832788339384839,
22.0965286888602));
#27102=CARTESIAN_POINT('Ctrl Pts',(-8.31657993781219,-1.25705549289238,
22.144250712315));
#27103=CARTESIAN_POINT('Ctrl Pts',(-7.50796944462182,-0.647460581310789,
22.1840190651941));
#27104=CARTESIAN_POINT('Ctrl Pts',(-7.38672571254854,0.080910305633487,
22.2158337474974));
#27105=CARTESIAN_POINT('Ctrl Pts',(-7.61201181389946,0.78409617299229,22.2476484298006));
#27106=CARTESIAN_POINT('Ctrl Pts',(-8.50026737069875,1.27036662422184,22.2874167826797));
#27107=CARTESIAN_POINT('Ctrl Pts',(-9.56952131288912,0.685346344803542,
22.3351388061345));
#27108=CARTESIAN_POINT('Ctrl Pts',(-9.65424245939207,-0.52819323080524,
22.3828608295894));
#27109=CARTESIAN_POINT('Ctrl Pts',(-8.68051222872802,-1.25737456087645,
22.4305828530443));
#27110=CARTESIAN_POINT('Ctrl Pts',(-7.53882304902558,-0.830644509004543,
22.4783048764991));
#27111=CARTESIAN_POINT('Ctrl Pts',(-7.32615378357976,0.159420473437757,
22.5180732293781));
#27112=CARTESIAN_POINT('Ctrl Pts',(-7.71102053144895,0.789580594279784,
22.5498879116814));
#27113=CARTESIAN_POINT('Ctrl Pts',(-8.34147358890413,1.17396729261948,22.5817025939846));
#27114=CARTESIAN_POINT('Ctrl Pts',(-9.33137631260206,0.960544042857,22.6214709468637));
#27115=CARTESIAN_POINT('Ctrl Pts',(-9.75723671581043,-0.181469808722496,
22.6691929703186));
#27116=CARTESIAN_POINT('Ctrl Pts',(-9.0273139919783,-1.15464440326701,22.7169149937734));
#27117=CARTESIAN_POINT('Ctrl Pts',(-7.813839293024,-1.06899903426609,22.7646370172283));
#27118=CARTESIAN_POINT('Ctrl Pts',(-7.2296335405858,0.000700156646207271,
22.8123590406831));
#27119=CARTESIAN_POINT('Ctrl Pts',(-7.71658035743571,0.888585106109542,
22.8521273935622));
#27120=CARTESIAN_POINT('Ctrl Pts',(-8.41993760159213,1.11333558688271,22.8839420758655));
#27121=CARTESIAN_POINT('Ctrl Pts',(-9.1482159365314,0.991537153505591,22.9157567581687));
#27122=CARTESIAN_POINT('Ctrl Pts',(-9.75719482334863,0.18246261964937,22.9555251110477));
#27123=CARTESIAN_POINT('Ctrl Pts',(-9.33205756918401,-0.959820635651876,
23.0032471345026));
#27124=CARTESIAN_POINT('Ctrl Pts',(-8.14332345540958,-1.21821409722222,
23.0509691579575));
#27125=CARTESIAN_POINT('Ctrl Pts',(-7.28166514512249,-0.359493577759317,
23.0986911814123));
#27126=CARTESIAN_POINT('Ctrl Pts',(-7.5397392445049,0.831703500581703,23.1464132048672));
#27127=CARTESIAN_POINT('Ctrl Pts',(-8.48891880428909,1.18457040071786,23.1861815577462));
#27128=CARTESIAN_POINT('Ctrl Pts',(-9.16788455925829,0.894346874631236,
23.2179962400495));
#27129=CARTESIAN_POINT('Ctrl Pts',(-9.63895731995363,0.325739236935478,
23.2498109223527));
#27130=CARTESIAN_POINT('Ctrl Pts',(-9.57013920684436,-0.684568118888431,
23.2895792752318));
#27131=CARTESIAN_POINT('Ctrl Pts',(-8.50125588334141,-1.27026527694676,
23.3373012986866));
#27132=CARTESIAN_POINT('Ctrl Pts',(-7.43321036561117,-0.687912509039083,
23.3850233221415));
#27133=CARTESIAN_POINT('Ctrl Pts',(-7.34342114791428,0.525262610479453,
23.4327453455963));
#27134=CARTESIAN_POINT('Ctrl Pts',(-8.31796568955919,1.2572569113933,23.4804673690513));
#27135=CARTESIAN_POINT('Ctrl Pts',(-9.26665926046044,0.90308549180325,23.5202357219303));
#27136=CARTESIAN_POINT('Ctrl Pts',(-9.59024222976098,0.239370000426331,
23.5520504042335));
#27137=CARTESIAN_POINT('Ctrl Pts',(-9.57446457380535,-0.498854394380288,
23.5838650865367));
#27138=CARTESIAN_POINT('Ctrl Pts',(-8.86139783388378,-1.21787644573988,
23.6236334394159));
#27139=CARTESIAN_POINT('Ctrl Pts',(-7.66984196271033,-0.961464031663683,
23.6713554628706));
#27140=CARTESIAN_POINT('Ctrl Pts',(-7.24315013794179,0.177741858818465,
23.7190774863255));
#27141=CARTESIAN_POINT('Ctrl Pts',(-7.96900166016501,1.1539567644206,23.7667995097804));
#27142=CARTESIAN_POINT('Ctrl Pts',(-9.1849326520489,1.06990592744461,23.8145215332352));
#27143=CARTESIAN_POINT('Ctrl Pts',(-9.67065841860297,0.181352403097706,
23.8542898861143));
#27144=CARTESIAN_POINT('Ctrl Pts',(-9.48111405364124,-0.532298159311048,
23.8861045684176));
#27145=CARTESIAN_POINT('Ctrl Pts',(-8.98617748353237,-1.08025982136771,
23.9179192507208));
#27146=CARTESIAN_POINT('Ctrl Pts',(-7.97647741697682,-1.1574780933083,23.9576876035999));
#27147=CARTESIAN_POINT('Ctrl Pts',(-7.24312457211183,-0.183955456104287,
24.0054096270547));
#27148=CARTESIAN_POINT('Ctrl Pts',(-7.66579587118509,0.956748250899926,
24.0531316505096));
#27149=CARTESIAN_POINT('Ctrl Pts',(-8.85344033668265,1.22010465922611,24.1008536739644));
#27150=CARTESIAN_POINT('Ctrl Pts',(-9.71799949535745,0.36098290919776,24.1485756974193));
#27151=CARTESIAN_POINT('Ctrl Pts',(-9.50396937211297,-0.628788777742109,
24.1883440502983));
#27152=CARTESIAN_POINT('Ctrl Pts',(-8.89369929202849,-1.04447450141904,
24.2201587326016));
#27153=CARTESIAN_POINT('Ctrl Pts',(-8.16088209878099,-1.13504575953045,
24.2519734149049));
#27154=CARTESIAN_POINT('Ctrl Pts',(-7.34677078253822,-0.532816857293743,
24.2917417677839));
#27155=CARTESIAN_POINT('Ctrl Pts',(-7.42912560559831,0.683230182643023,
24.3394637912387));
#27156=CARTESIAN_POINT('Ctrl Pts',(-8.49511057720914,1.26934622450956,24.3871858146936));
#27157=CARTESIAN_POINT('Ctrl Pts',(-9.56557919629318,0.691459635471783,
24.4349078381484));
#27158=CARTESIAN_POINT('Ctrl Pts',(-9.65729967351157,-0.523916879966565,
24.4826298616034));
#27159=CARTESIAN_POINT('Ctrl Pts',(-8.84785192415903,-1.13239960526931,
24.5223982144823));
#27160=CARTESIAN_POINT('Ctrl Pts',(-8.11435874014051,-1.04747646052419,
24.5542128967857));
#27161=CARTESIAN_POINT('Ctrl Pts',(-7.50090443876472,-0.636504427852052,
24.5860275790888));
#27162=CARTESIAN_POINT('Ctrl Pts',(-7.27925573292454,0.351589058172031,
24.625795931968));
#27163=CARTESIAN_POINT('Ctrl Pts',(-8.13717079459291,1.21734564473828,24.6735179554228));
#27164=CARTESIAN_POINT('Ctrl Pts',(-9.32680884437268,0.963146343500833,
24.7212399788777));
#27165=CARTESIAN_POINT('Ctrl Pts',(-9.75825527430768,-0.174267368536162,
24.7689620023325));
#27166=CARTESIAN_POINT('Ctrl Pts',(-9.03242394654871,-1.15341066952121,
24.8166840257874));
#27167=CARTESIAN_POINT('Ctrl Pts',(-8.02215897329008,-1.08397314558436,
24.8564523786664));
#27168=CARTESIAN_POINT('Ctrl Pts',(-7.52301574135941,-0.539840601498972,
24.8882670609697));
#27169=CARTESIAN_POINT('Ctrl Pts',(-7.32797922977689,0.1723285853273,24.9200817432729));
#27170=CARTESIAN_POINT('Ctrl Pts',(-7.80684540644956,1.06459764271005,24.9598500961519));
#27171=CARTESIAN_POINT('Ctrl Pts',(-9.02209281164555,1.15801318951368,25.0075721196068));
#27172=CARTESIAN_POINT('Ctrl Pts',(-9.75544329080836,0.187419016367583,
25.0552941430617));
#27173=CARTESIAN_POINT('Ctrl Pts',(-9.33754026227136,-0.95504018770629,
25.1030161665166));
#27174=CARTESIAN_POINT('Ctrl Pts',(-8.14799508151347,-1.22062441757699,
25.1507381899714));
#27175=CARTESIAN_POINT('Ctrl Pts',(-7.42941034956166,-0.507116976179599,
25.1905065428505));
#27176=CARTESIAN_POINT('Ctrl Pts',(-7.4079460804348,0.230963965632277,25.2223212251537));
#27177=CARTESIAN_POINT('Ctrl Pts',(-7.72640636278891,0.897152557607554,
25.254135907457));
#27178=CARTESIAN_POINT('Ctrl Pts',(-8.67234334103518,1.25862194650527,25.293904260336));
#27179=CARTESIAN_POINT('Ctrl Pts',(-9.65249805028128,0.534156994859609,
25.3416262837909));
#27180=CARTESIAN_POINT('Ctrl Pts',(-9.57205747047455,-0.679673836580168,
25.3893483072457));
#27181=CARTESIAN_POINT('Ctrl Pts',(-8.50852993454981,-1.27023725786806,
25.4370703307006));
#27182=CARTESIAN_POINT('Ctrl Pts',(-7.43516627654756,-0.69279186832866,
25.4847923541554));
#27183=CARTESIAN_POINT('Ctrl Pts',(-7.3585670705502,0.316955351308209,25.5245607070345));
#27184=CARTESIAN_POINT('Ctrl Pts',(-7.82524545288061,0.889175133368002,
25.5563753893377));
#27185=CARTESIAN_POINT('Ctrl Pts',(-8.50195525644396,1.18462061611619,25.588190071641));
#27186=CARTESIAN_POINT('Ctrl Pts',(-9.45382504141213,0.839076409988411,
25.62795842452));
#27187=CARTESIAN_POINT('Ctrl Pts',(-9.72106814323682,-0.350097187409116,
25.6756804479749));
#27188=CARTESIAN_POINT('Ctrl Pts',(-8.86605075290398,-1.21543020796356,
25.7234024714297));
#27189=CARTESIAN_POINT('Ctrl Pts',(-7.67536132038316,-0.966202100566644,
25.7711244948846));
#27190=CARTESIAN_POINT('Ctrl Pts',(-7.24143684011856,0.172772115843602,
25.8188465183395));
#27191=CARTESIAN_POINT('Ctrl Pts',(-7.84416476429791,0.986514049959185,
25.8586148712185));
#27192=CARTESIAN_POINT('Ctrl Pts',(-8.57148318594807,1.11391932867017,25.8904295535218));
#27193=CARTESIAN_POINT('Ctrl Pts',(-9.27655097556757,0.894593991428686,
25.922244235825));
#27194=CARTESIAN_POINT('Ctrl Pts',(-9.77032336852924,0.0104866959759273,
25.962012588704));
#27195=CARTESIAN_POINT('Ctrl Pts',(-9.19437562557584,-1.06368131583936,
26.0097346121589));
#27196=CARTESIAN_POINT('Ctrl Pts',(-7.98159672426513,-1.15867242473413,
26.0574566356138));
#27197=CARTESIAN_POINT('Ctrl Pts',(-7.24419858603817,-0.191149835864602,
26.1051786590687));
#27198=CARTESIAN_POINT('Ctrl Pts',(-7.66124858591289,0.954110840935556,
26.1529006825235));
#27199=CARTESIAN_POINT('Ctrl Pts',(-8.64947777999604,1.17515370077396,26.1926690354026));
#27200=CARTESIAN_POINT('Ctrl Pts',(-9.28287334059143,0.795635248873192,
26.2244837177058));
#27201=CARTESIAN_POINT('Ctrl Pts',(-9.67258325123935,0.168458736990063,
26.2562984000091));
#27202=CARTESIAN_POINT('Ctrl Pts',(-9.46754748980759,-0.823215212681873,
26.2960667528881));
#27203=CARTESIAN_POINT('Ctrl Pts',(-8.32917960185085,-1.25872786679082,
26.343788776343));
#27204=CARTESIAN_POINT('Ctrl Pts',(-7.3498608497893,-0.537069529283282,
26.3915107997978));
#27205=CARTESIAN_POINT('Ctrl Pts',(-7.42523070112171,0.67708670438005,26.4392328232527));
#27206=CARTESIAN_POINT('Ctrl Pts',(-8.48994607585931,1.27032686739802,26.4869548467075));
#27207=CARTESIAN_POINT('Ctrl Pts',(-9.38192137064002,0.790913726751365,
26.5267231995866));
#27208=CARTESIAN_POINT('Ctrl Pts',(-9.61261794082105,0.0894842691280413,
26.5585378818898));
#27209=CARTESIAN_POINT('Ctrl Pts',(-9.49698897915128,-0.639799032983159,
26.5903525641931));
#27210=CARTESIAN_POINT('Ctrl Pts',(-8.6930986353653,-1.25560517219546,26.6301209170721));
#27211=CARTESIAN_POINT('Ctrl Pts',(-7.54725738779159,-0.840152941994423,
26.677842940527));
#27212=CARTESIAN_POINT('Ctrl Pts',(-7.2788101728749,0.346351194971367,26.7255649639818));
#27213=CARTESIAN_POINT('Ctrl Pts',(-8.13020571177932,1.21524797282651,26.7732869874367));
#27214=CARTESIAN_POINT('Ctrl Pts',(-9.32354478705541,0.967266982346513,
26.8210090108916));
#27215=CARTESIAN_POINT('Ctrl Pts',(-9.68443415000749,0.0211085634589513,
26.8607773637706));
#27216=CARTESIAN_POINT('Ctrl Pts',(-9.3999686838854,-0.660289697544845,
26.8925920460739));
#27217=CARTESIAN_POINT('Ctrl Pts',(-8.83536920081072,-1.13615902333382,
26.9244067283771));
#27218=CARTESIAN_POINT('Ctrl Pts',(-7.82451547856594,-1.07589594883839,
26.9641750812562));
#27219=CARTESIAN_POINT('Ctrl Pts',(-7.22979086994386,-0.0120090374988551,
27.011897104711));
#27220=CARTESIAN_POINT('Ctrl Pts',(-7.80308142666439,1.06092801182352,27.0596191281659));
#27221=CARTESIAN_POINT('Ctrl Pts',(-9.01545298211099,1.16098392507927,27.1073411516207));
#27222=CARTESIAN_POINT('Ctrl Pts',(-9.75567088378897,0.192670867098664,
27.1550631750756));
#27223=CARTESIAN_POINT('Ctrl Pts',(-9.40954314716847,-0.758986884336038,
27.1948315279547));
#27224=CARTESIAN_POINT('Ctrl Pts',(-8.74859067031979,-1.08817682170144,
27.2266462102579));
#27225=CARTESIAN_POINT('Ctrl Pts',(-8.01025916428869,-1.0786490351324,27.2584608925611));
#27226=CARTESIAN_POINT('Ctrl Pts',(-7.28522654001878,-0.371694595533894,
27.2982292454403));
#27227=CARTESIAN_POINT('Ctrl Pts',(-7.53154286743781,0.821989193024468,
27.345951268895));
#27228=CARTESIAN_POINT('Ctrl Pts',(-8.66709585666284,1.25830946861972,27.3936732923499));
#27229=CARTESIAN_POINT('Ctrl Pts',(-9.64942034682812,0.540747924043256,
27.4413953158048));
#27230=CARTESIAN_POINT('Ctrl Pts',(-9.57566576368643,-0.675851016317035,
27.4891173392597));
#27231=CARTESIAN_POINT('Ctrl Pts',(-8.69125590043384,-1.16908126650995,
27.5288856921387));
#27232=CARTESIAN_POINT('Ctrl Pts',(-7.97602635588388,-0.985584971948125,
27.5607003744419));
#27233=CARTESIAN_POINT('Ctrl Pts',(-7.42389453276778,-0.495304805698656,
27.5925150567452));
#27234=CARTESIAN_POINT('Ctrl Pts',(-7.33813159580452,0.513705404639772,
27.6322834096242));
#27235=CARTESIAN_POINT('Ctrl Pts',(-8.30541128545435,1.2552731508445,27.6800054330791));
#27236=CARTESIAN_POINT('Ctrl Pts',(-9.44965216623517,0.842273415997902,
27.727727456534));
#27237=CARTESIAN_POINT('Ctrl Pts',(-9.72305292585927,-0.34309909881355,
27.7754494799888));
#27238=CARTESIAN_POINT('Ctrl Pts',(-8.87128072736936,-1.21490001765905,
27.8231715034437));
#27239=CARTESIAN_POINT('Ctrl Pts',(-7.87973267238346,-1.00925629522272,
27.8629398563227));
#27240=CARTESIAN_POINT('Ctrl Pts',(-7.45889571320355,-0.402526993718913,
27.894754538626));
#27241=CARTESIAN_POINT('Ctrl Pts',(-7.3621241700199,0.329497227154213,27.9265692209292));
#27242=CARTESIAN_POINT('Ctrl Pts',(-7.95743978257428,1.1486774316103,27.9663375738082));
#27243=CARTESIAN_POINT('Ctrl Pts',(-9.17414040953262,1.07661978399751,28.0140595972632));
#27244=CARTESIAN_POINT('Ctrl Pts',(-9.76925935148402,0.0156346666823883,
28.061781620718));
#27245=CARTESIAN_POINT('Ctrl Pts',(-9.20045532592656,-1.05968758954737,
28.1095036441729));
#27246=CARTESIAN_POINT('Ctrl Pts',(-7.98589880216476,-1.16169332864071,
28.1572256676277));
#27247=CARTESIAN_POINT('Ctrl Pts',(-7.37058564730116,-0.35742558256636,
28.1969940205068));
#27248=CARTESIAN_POINT('Ctrl Pts',(-7.44929649627935,0.376760220734205,
28.22880870281));
#27249=CARTESIAN_POINT('Ctrl Pts',(-7.85506071766296,0.993671549987,28.2606233851133));
#27250=CARTESIAN_POINT('Ctrl Pts',(-8.84124247215261,1.22367683912963,28.3003917379923));
#27251=CARTESIAN_POINT('Ctrl Pts',(-9.71423056098527,0.37312142237029,28.3481137614471));
#27252=CARTESIAN_POINT('Ctrl Pts',(-9.4701110321357,-0.818625878810101,
28.3958357849021));
#27253=CARTESIAN_POINT('Ctrl Pts',(-8.33639040638821,-1.25968541784629,
28.4435578083568));
#27254=CARTESIAN_POINT('Ctrl Pts',(-7.35113779671057,-0.542168856810177,
28.4912798318118));
#27255=CARTESIAN_POINT('Ctrl Pts',(-7.4120206186405,0.468647727901989,28.5310481846908));
#27256=CARTESIAN_POINT('Ctrl Pts',(-7.95190825959645,0.972379329670431,
28.5628628669941));
#27257=CARTESIAN_POINT('Ctrl Pts',(-8.66240088239154,1.1734375912628,28.5946775492973));
#27258=CARTESIAN_POINT('Ctrl Pts',(-9.55869172269085,0.702141914089626,
28.6344459021764));
#27259=CARTESIAN_POINT('Ctrl Pts',(-9.66239137790161,-0.51227115470021,
28.6821679256312));
#27260=CARTESIAN_POINT('Ctrl Pts',(-8.69804002694774,-1.25381174500308,
28.7298899490861));
#27261=CARTESIAN_POINT('Ctrl Pts',(-7.55208407768074,-0.845594970502949,
28.7776119725409));
#27262=CARTESIAN_POINT('Ctrl Pts',(-7.27643948470255,0.341659331902066,
28.8253339959958));
#27263=CARTESIAN_POINT('Ctrl Pts',(-7.98383831473153,1.06625838374073,28.8651023488749));
#27264=CARTESIAN_POINT('Ctrl Pts',(-8.7217111041732,1.09396997251344,28.8969170311781));
#27265=CARTESIAN_POINT('Ctrl Pts',(-9.39057170098815,0.781160600976512,
28.9287317134813));
#27266=CARTESIAN_POINT('Ctrl Pts',(-9.76003577755879,-0.161682533818022,
28.9685000663604));
#27267=CARTESIAN_POINT('Ctrl Pts',(-9.04389413728366,-1.14793494130765,
29.0162220898153));
#27268=CARTESIAN_POINT('Ctrl Pts',(-7.82942578787744,-1.07777272054675,
29.0639441132701));
#27269=CARTESIAN_POINT('Ctrl Pts',(-7.22988053396106,-0.0192825748490968,
29.111666136725));
#27270=CARTESIAN_POINT('Ctrl Pts',(-7.79821866312692,1.05893083384072,29.1593881601798));
#27271=CARTESIAN_POINT('Ctrl Pts',(-8.80728164041408,1.14407521357788,29.1991565130589));
#27272=CARTESIAN_POINT('Ctrl Pts',(-9.38343094294497,0.682257445520128,
29.2309711953621));
#27273=CARTESIAN_POINT('Ctrl Pts',(-9.68459549643142,0.00807318411422593,
29.2627858776654));
#27274=CARTESIAN_POINT('Ctrl Pts',(-9.34711913065458,-0.946688199617532,
29.3025542305444));
#27275=CARTESIAN_POINT('Ctrl Pts',(-8.1602548489812,-1.22398743093969,29.3502762539993));
#27276=CARTESIAN_POINT('Ctrl Pts',(-7.2877070281187,-0.376327816437086,
29.3979982774541));
#27277=CARTESIAN_POINT('Ctrl Pts',(-7.52686125179537,0.816432151475763,
29.445720300909));
#27278=CARTESIAN_POINT('Ctrl Pts',(-8.66209281831706,1.25997621452946,29.4934423243638));
#27279=CARTESIAN_POINT('Ctrl Pts',(-9.48095999247722,0.664170613867274,
29.533210677243));
#27280=CARTESIAN_POINT('Ctrl Pts',(-9.61444029499092,-0.0620612536963943,
29.5650253595461));
#27281=CARTESIAN_POINT('Ctrl Pts',(-9.40124341722056,-0.768925025649959,
29.5968400418494));
#27282=CARTESIAN_POINT('Ctrl Pts',(-8.52101122107249,-1.27024239984106,
29.6366083947285));
#27283=CARTESIAN_POINT('Ctrl Pts',(-7.44261890700309,-0.703265592319027,
29.6843304181833));
#27284=CARTESIAN_POINT('Ctrl Pts',(-7.33627786239381,0.508411815248644,
29.7320524416382));
#27285=CARTESIAN_POINT('Ctrl Pts',(-8.2995618713472,1.25445422207268,29.779774465093));
#27286=CARTESIAN_POINT('Ctrl Pts',(-9.25349370071878,0.914194267159221,
29.8195428179721));
#27287=CARTESIAN_POINT('Ctrl Pts',(-9.58672570471092,0.255051675598665,
29.8513575002753));
#27288=CARTESIAN_POINT('Ctrl Pts',(-9.58134081666635,-0.482923354571183,
29.8831721825786));
#27289=CARTESIAN_POINT('Ctrl Pts',(-8.87961978715692,-1.21312531614331,
29.9229405354576));
#27290=CARTESIAN_POINT('Ctrl Pts',(-7.68284834089023,-0.972316947591664,
29.9706625589125));
#27291=CARTESIAN_POINT('Ctrl Pts',(-7.31615319782486,-0.031134755764136,
30.0104309117915));
#27292=CARTESIAN_POINT('Ctrl Pts',(-7.59495772883202,0.655650918756826,
30.0422455940948));
#27293=CARTESIAN_POINT('Ctrl Pts',(-7.87606563100468,0.891954634492901,
30.0581529352464));
#27294=CARTESIAN_POINT('Ctrl Pts',(-8.03748311344989,0.969001292713786,
30.0661066058222));
#27295=CARTESIAN_POINT('Ctrl Pts',(-7.90984029786111,-0.827606761449139,
1.8));
#27296=CARTESIAN_POINT('Ctrl Pts',(-7.77197649840879,-0.729297198731152,
1.80795367057581));
#27297=CARTESIAN_POINT('Ctrl Pts',(-7.54863701760608,-0.4628715196836,1.82386101172743));
#27298=CARTESIAN_POINT('Ctrl Pts',(-7.40132815197149,0.223190340066621,
1.85567569403067));
#27299=CARTESIAN_POINT('Ctrl Pts',(-7.8975843624851,1.04057513890883,1.89544404690973));
#27300=CARTESIAN_POINT('Ctrl Pts',(-9.05290778687487,1.06881550059125,1.94316607036458));
#27301=CARTESIAN_POINT('Ctrl Pts',(-9.58740885957362,0.272911730207072,
1.98293442324364));
#27302=CARTESIAN_POINT('Ctrl Pts',(-9.47139510427018,-0.416034089157043,
2.01474910554688));
#27303=CARTESIAN_POINT('Ctrl Pts',(-9.05259577107697,-0.975943072842501,
2.04656378785012));
#27304=CARTESIAN_POINT('Ctrl Pts',(-8.10737674978987,-1.1367365362355,2.08633214072917));
#27305=CARTESIAN_POINT('Ctrl Pts',(-7.33160128421964,-0.283165032011243,
2.13405416418404));
#27306=CARTESIAN_POINT('Ctrl Pts',(-7.62947585871493,0.829120622165689,
2.1817761876389));
#27307=CARTESIAN_POINT('Ctrl Pts',(-8.72792114609409,1.18088449447148,2.22949821109376));
#27308=CARTESIAN_POINT('Ctrl Pts',(-9.4663990177441,0.569107464161922,2.26926656397281));
#27309=CARTESIAN_POINT('Ctrl Pts',(-9.54924456809875,-0.124914290005348,
2.30108124627605));
#27310=CARTESIAN_POINT('Ctrl Pts',(-9.30568364649701,-0.780136065581114,
2.3328959285793));
#27311=CARTESIAN_POINT('Ctrl Pts',(-8.44448253610224,-1.20134333884891,
2.37266428145834));
#27312=CARTESIAN_POINT('Ctrl Pts',(-7.45877664796192,-0.601610010654219,
2.42038630491321));
#27313=CARTESIAN_POINT('Ctrl Pts',(-7.43142063634725,0.549701954261673,
2.46810832836807));
#27314=CARTESIAN_POINT('Ctrl Pts',(-8.38397803243201,1.19692518514985,2.51583035182294));
#27315=CARTESIAN_POINT('Ctrl Pts',(-9.44509012097467,0.743724623326929,
2.56355237527779));
#27316=CARTESIAN_POINT('Ctrl Pts',(-9.60315220690443,-0.201811312771686,
2.60332072815685));
#27317=CARTESIAN_POINT('Ctrl Pts',(-9.21178449951522,-0.781003980273609,
2.63513541046009));
#27318=CARTESIAN_POINT('Ctrl Pts',(-8.5988604131823,-1.11709346661785,2.66695009276333));
#27319=CARTESIAN_POINT('Ctrl Pts',(-7.67200907556847,-0.872212497622945,
2.70671844564238));
#27320=CARTESIAN_POINT('Ctrl Pts',(-7.31894661150667,0.226289253311605,
2.75444046909725));
#27321=CARTESIAN_POINT('Ctrl Pts',(-8.05154383597101,1.11485849141834,2.80216249255211));
#27322=CARTESIAN_POINT('Ctrl Pts',(-9.19537976741075,0.981091778944714,
2.84988451600697));
#27323=CARTESIAN_POINT('Ctrl Pts',(-9.70133158308663,-0.0559097679809395,
2.89760653946183));
#27324=CARTESIAN_POINT('Ctrl Pts',(-9.20222130442427,-0.874389043558423,
2.93737489234089));
#27325=CARTESIAN_POINT('Ctrl Pts',(-8.52729507837894,-1.05634272967533,
2.96918957464412));
#27326=CARTESIAN_POINT('Ctrl Pts',(-7.84387270007337,-0.90948772098803,
3.00100425694737));
#27327=CARTESIAN_POINT('Ctrl Pts',(-7.3031589137604,-0.117876702228567,
3.04077260982642));
#27328=CARTESIAN_POINT('Ctrl Pts',(-7.75488071429994,0.943870403632135,
3.08849463328128));
#27329=CARTESIAN_POINT('Ctrl Pts',(-8.89028197036155,1.13653082253155,3.13621665673614));
#27330=CARTESIAN_POINT('Ctrl Pts',(-9.66779092684549,0.286981604349885,
3.18393868019101));
#27331=CARTESIAN_POINT('Ctrl Pts',(-9.37193042071709,-0.828287897935989,
3.23166070364586));
#27332=CARTESIAN_POINT('Ctrl Pts',(-8.45896286510886,-1.12070821481404,
3.27142905652493));
#27333=CARTESIAN_POINT('Ctrl Pts',(-7.82949920621424,-0.816721293551666,
3.30324373882816));
#27334=CARTESIAN_POINT('Ctrl Pts',(-7.4087428992097,-0.258512841293276,
3.33505842113141));
#27335=CARTESIAN_POINT('Ctrl Pts',(-7.51776071245581,0.693923254147438,
3.37482677401045));
#27336=CARTESIAN_POINT('Ctrl Pts',(-8.55405558131559,1.20132097455938,3.42254879746531));
#27337=CARTESIAN_POINT('Ctrl Pts',(-9.53876020395445,0.604151939157171,
3.47027082092018));
#27338=CARTESIAN_POINT('Ctrl Pts',(-9.57091178241385,-0.547030203992542,
3.51799284437504));
#27339=CARTESIAN_POINT('Ctrl Pts',(-8.61746895833269,-1.19688117390714,
3.5657148678299));
#27340=CARTESIAN_POINT('Ctrl Pts',(-7.73570976145469,-0.820689576164182,
3.60548322070896));
#27341=CARTESIAN_POINT('Ctrl Pts',(-7.4585680161445,-0.178953649869286,
3.6372979030122));
#27342=CARTESIAN_POINT('Ctrl Pts',(-7.50559368937304,0.518485331080344,
3.66911258531544));
#27343=CARTESIAN_POINT('Ctrl Pts',(-8.21119763983049,1.1674402328969,3.70888093819449));
#27344=CARTESIAN_POINT('Ctrl Pts',(-9.32687871186513,0.873135548271195,
3.75660296164935));
#27345=CARTESIAN_POINT('Ctrl Pts',(-9.68084973637808,-0.222747002236243,
3.80432498510421));
#27346=CARTESIAN_POINT('Ctrl Pts',(-8.95197025619296,-1.11436842081398,
3.85204700855908));
#27347=CARTESIAN_POINT('Ctrl Pts',(-7.80574215880651,-0.982002826150276,
3.89976903201393));
#27348=CARTESIAN_POINT('Ctrl Pts',(-7.38504307341408,-0.120590219414704,
3.939537384893));
#27349=CARTESIAN_POINT('Ctrl Pts',(-7.59532800195641,0.546052709685047,
3.97135206719623));
#27350=CARTESIAN_POINT('Ctrl Pts',(-8.08721095204589,1.0427253478503,4.00316674949948));
#27351=CARTESIAN_POINT('Ctrl Pts',(-9.04542379982193,1.071837851176,4.04293510237852));
#27352=CARTESIAN_POINT('Ctrl Pts',(-9.69660396175139,0.119302340762661,
4.09065712583339));
#27353=CARTESIAN_POINT('Ctrl Pts',(-9.24728286443354,-0.941058259319486,
4.13837914928825));
#27354=CARTESIAN_POINT('Ctrl Pts',(-8.11269623164964,-1.13845943309904,
4.18610117274311));
#27355=CARTESIAN_POINT('Ctrl Pts',(-7.3324614462396,-0.288404622204439,
4.23382319619797));
#27356=CARTESIAN_POINT('Ctrl Pts',(-7.57791048256601,0.638296068450016,
4.27359154907703));
#27357=CARTESIAN_POINT('Ctrl Pts',(-8.17310957881519,1.0048619996478,4.30540623138027));
#27358=CARTESIAN_POINT('Ctrl Pts',(-8.87006013423126,1.05864368236586,4.33722091368351));
#27359=CARTESIAN_POINT('Ctrl Pts',(-9.61375947960335,0.453721635167941,
4.37698926656257));
#27360=CARTESIAN_POINT('Ctrl Pts',(-9.48299272702672,-0.692689965571268,
4.42471129001742));
#27361=CARTESIAN_POINT('Ctrl Pts',(-8.44942055884309,-1.20060986462784,
4.4724333134723));
#27362=CARTESIAN_POINT('Ctrl Pts',(-7.46223022206171,-0.607559032348711,
4.52015533692714));
#27363=CARTESIAN_POINT('Ctrl Pts',(-7.42834802491375,0.545788919747837,
4.56787736038202));
#27364=CARTESIAN_POINT('Ctrl Pts',(-8.22029040779656,1.08601726192072,4.60764571326106));
#27365=CARTESIAN_POINT('Ctrl Pts',(-8.91024806509605,0.973807738151371,
4.6394603955643));
#27366=CARTESIAN_POINT('Ctrl Pts',(-9.47250745857794,0.558480252265651,
4.67127507786755));
#27367=CARTESIAN_POINT('Ctrl Pts',(-9.63914480964413,-0.385580864782726,
4.71104343074659));
#27368=CARTESIAN_POINT('Ctrl Pts',(-8.79017906601008,-1.16700051389882,
4.75876545420146));
#27369=CARTESIAN_POINT('Ctrl Pts',(-7.6762153949145,-0.874872134276515,
4.80648747765633));
#27370=CARTESIAN_POINT('Ctrl Pts',(-7.3176700873064,0.219522361823356,4.85420950111118));
#27371=CARTESIAN_POINT('Ctrl Pts',(-8.04665782451571,1.11391398795103,4.90193152456605));
#27372=CARTESIAN_POINT('Ctrl Pts',(-8.99902690165246,1.00431225253282,4.9416998774451));
#27373=CARTESIAN_POINT('Ctrl Pts',(-9.4473933441329,0.468028671441437,4.97351455974835));
#27374=CARTESIAN_POINT('Ctrl Pts',(-9.60086385536787,-0.213938591901918,
5.00532924205157));
#27375=CARTESIAN_POINT('Ctrl Pts',(-9.10920461013546,-1.03691525382525,
5.04509759493064));
#27376=CARTESIAN_POINT('Ctrl Pts',(-7.95590503741594,-1.07240606184469,
5.09281961838549));
#27377=CARTESIAN_POINT('Ctrl Pts',(-7.30459975514546,-0.122640048561389,
5.14054164184036));
#27378=CARTESIAN_POINT('Ctrl Pts',(-7.74948793304144,0.939588062472147,
5.18826366529521));
#27379=CARTESIAN_POINT('Ctrl Pts',(-8.88596892398453,1.13901338462022,5.23598568875008));
#27380=CARTESIAN_POINT('Ctrl Pts',(-9.53449109503047,0.433011689753366,
5.27575404162913));
#27381=CARTESIAN_POINT('Ctrl Pts',(-9.52269065962012,-0.265911264380261,
5.30756872393238));
#27382=CARTESIAN_POINT('Ctrl Pts',(-9.19255643359114,-0.882063793300652,
5.33938340623562));
#27383=CARTESIAN_POINT('Ctrl Pts',(-8.2822812089624,-1.18276034286533,5.37915175911467));
#27384=CARTESIAN_POINT('Ctrl Pts',(-7.38687368970327,-0.455020776575932,
5.42687378256953));
#27385=CARTESIAN_POINT('Ctrl Pts',(-7.51573379599412,0.689378246365011,
5.47459580602439));
#27386=CARTESIAN_POINT('Ctrl Pts',(-8.54717542720796,1.20161082254544,5.52231782947927));
#27387=CARTESIAN_POINT('Ctrl Pts',(-9.53712273626146,0.608851320566278,
5.57003985293409));
#27388=CARTESIAN_POINT('Ctrl Pts',(-9.56564774971944,-0.349379196115496,
5.60980820581319));
#27389=CARTESIAN_POINT('Ctrl Pts',(-9.09943307031321,-0.870221224754611,
5.6416228881164));
#27390=CARTESIAN_POINT('Ctrl Pts',(-8.44663234976153,-1.1201887533217,5.67343757041967));
#27391=CARTESIAN_POINT('Ctrl Pts',(-7.56149427253223,-0.752017619564837,
5.7132059232987));
#27392=CARTESIAN_POINT('Ctrl Pts',(-7.36048402589915,0.384184115444124,
5.76092794675357));
#27393=CARTESIAN_POINT('Ctrl Pts',(-8.20669107470487,1.16532922440469,5.80864997020842));
#27394=CARTESIAN_POINT('Ctrl Pts',(-9.32186521390639,0.87785628662166,5.8563719936633));
#27395=CARTESIAN_POINT('Ctrl Pts',(-9.6826861022262,-0.218121718833277,
5.90409401711814));
#27396=CARTESIAN_POINT('Ctrl Pts',(-9.07730820347234,-0.961450044133312,
5.94386236999722));
#27397=CARTESIAN_POINT('Ctrl Pts',(-8.3839558401117,-1.05030411727003,5.97567705230044));
#27398=CARTESIAN_POINT('Ctrl Pts',(-7.72672464100434,-0.812229135361763,
6.00749173460371));
#27399=CARTESIAN_POINT('Ctrl Pts',(-7.29822264555078,0.0453286990641955,
6.04726008748272));
#27400=CARTESIAN_POINT('Ctrl Pts',(-7.88960083185226,1.03610180258269,6.09498211093762));
#27401=CARTESIAN_POINT('Ctrl Pts',(-9.04063450660887,1.07318994459191,6.14270413439245));
#27402=CARTESIAN_POINT('Ctrl Pts',(-9.69590116689828,0.126152640883819,
6.19042615784734));
#27403=CARTESIAN_POINT('Ctrl Pts',(-9.25169784766887,-0.938761868865437,
6.23814818130218));
#27404=CARTESIAN_POINT('Ctrl Pts',(-8.30753474198256,-1.10482038070298,
6.27791653418125));
#27405=CARTESIAN_POINT('Ctrl Pts',(-7.72504936719716,-0.718370727770171,
6.30973121648449));
#27406=CARTESIAN_POINT('Ctrl Pts',(-7.38378353437386,-0.10831320799179,
6.34154589878772));
#27407=CARTESIAN_POINT('Ctrl Pts',(-7.62080949776357,0.820577577930954,
6.38131425166678));
#27408=CARTESIAN_POINT('Ctrl Pts',(-8.71628317856752,1.18292674179735,6.42903627512163));
#27409=CARTESIAN_POINT('Ctrl Pts',(-9.61102220693821,0.457877693931059,
6.4767582985765));
#27410=CARTESIAN_POINT('Ctrl Pts',(-9.48694324310275,-0.687049579495082,
6.52448032203136));
#27411=CARTESIAN_POINT('Ctrl Pts',(-8.45426188445871,-1.20176184221855,
6.57220234548622));
#27412=CARTESIAN_POINT('Ctrl Pts',(-7.63158681559905,-0.709598118880692,
6.61197069836528));
#27413=CARTESIAN_POINT('Ctrl Pts',(-7.44392618126472,-0.0362363792399661,
6.64378538066852));
#27414=CARTESIAN_POINT('Ctrl Pts',(-7.58499054185306,0.648404688957481,
6.67560006297176));
#27415=CARTESIAN_POINT('Ctrl Pts',(-8.37199588104198,1.19580033707788,6.71536841585081));
#27416=CARTESIAN_POINT('Ctrl Pts',(-9.43752891208507,0.75308275029716,6.76309043930567));
#27417=CARTESIAN_POINT('Ctrl Pts',(-9.6397939597727,-0.380646891718703,
6.81081246276053));
#27418=CARTESIAN_POINT('Ctrl Pts',(-8.7968570426639,-1.16531969262148,6.85853448621541));
#27419=CARTESIAN_POINT('Ctrl Pts',(-7.67912294882438,-0.878910898486879,
6.90625650967025));
#27420=CARTESIAN_POINT('Ctrl Pts',(-7.37898454940943,0.0315485133979244,
6.94602486254932));
#27421=CARTESIAN_POINT('Ctrl Pts',(-7.67763196849479,0.663562963521021,
6.97783954485255));
#27422=CARTESIAN_POINT('Ctrl Pts',(-8.23225858352771,1.08902960614752,7.0096542271558));
#27423=CARTESIAN_POINT('Ctrl Pts',(-9.18558342222681,0.988078373305267,
7.04942258003485));
#27424=CARTESIAN_POINT('Ctrl Pts',(-9.70173552716583,-0.0438840806899642,
7.09714460348971));
#27425=CARTESIAN_POINT('Ctrl Pts',(-9.1129237266811,-1.03360864556213,7.14486662694457));
#27426=CARTESIAN_POINT('Ctrl Pts',(-7.96205500537781,-1.07550419457644,
7.19258865039944));
#27427=CARTESIAN_POINT('Ctrl Pts',(-7.30415612412785,-0.127596728660616,
7.24031067385429));
#27428=CARTESIAN_POINT('Ctrl Pts',(-7.67286987062921,0.757315454911259,
7.28007902673335));
#27429=CARTESIAN_POINT('Ctrl Pts',(-8.31223670967161,1.03987976834036,7.31189370903659));
#27430=CARTESIAN_POINT('Ctrl Pts',(-9.0100487876404,0.998759822673581,7.34370839133983));
#27431=CARTESIAN_POINT('Ctrl Pts',(-9.66495359809054,0.298674764454046,
7.38347674421889));
#27432=CARTESIAN_POINT('Ctrl Pts',(-9.38010405357526,-0.819457713778441,
7.43119876767374));
#27433=CARTESIAN_POINT('Ctrl Pts',(-8.28725724730808,-1.18269304897191,
7.47892079112861));
#27434=CARTESIAN_POINT('Ctrl Pts',(-7.38949758043417,-0.461387544184974,
7.52664281458347));
#27435=CARTESIAN_POINT('Ctrl Pts',(-7.51215524722395,0.685919999007586,
7.57436483803833));
#27436=CARTESIAN_POINT('Ctrl Pts',(-8.3699756368797,1.11389614154802,7.61413319091739));
#27437=CARTESIAN_POINT('Ctrl Pts',(-9.03837480793247,0.909262092018708,
7.64594787322062));
#27438=CARTESIAN_POINT('Ctrl Pts',(-9.53919359505327,0.421601258490334,
7.67776255552388));
#27439=CARTESIAN_POINT('Ctrl Pts',(-9.57641663143542,-0.536330808545463,
7.71753090840291));
#27440=CARTESIAN_POINT('Ctrl Pts',(-8.62942769870831,-1.1955511534843,7.76525293185779));
#27441=CARTESIAN_POINT('Ctrl Pts',(-7.56530144703071,-0.755222445367275,
7.81297495531264));
#27442=CARTESIAN_POINT('Ctrl Pts',(-7.35830271009327,0.377652469884987,
7.86069697876751));
#27443=CARTESIAN_POINT('Ctrl Pts',(-8.20172212694212,1.16505528240931,7.90841900222237));
#27444=CARTESIAN_POINT('Ctrl Pts',(-9.13046741664916,0.927459856653719,
7.94818735510142));
#27445=CARTESIAN_POINT('Ctrl Pts',(-9.50205876271649,0.335385184320401,
7.98000203740466));
#27446=CARTESIAN_POINT('Ctrl Pts',(-9.56173842624569,-0.361085119319172,
8.01181671970791));
#27447=CARTESIAN_POINT('Ctrl Pts',(-8.96313370552467,-1.10987867419497,
8.05158507258695));
#27448=CARTESIAN_POINT('Ctrl Pts',(-7.8156562002608,-0.988821345617644,
8.09930709604182));
#27449=CARTESIAN_POINT('Ctrl Pts',(-7.29900498391781,0.0404140848611043,
8.14702911949668));
#27450=CARTESIAN_POINT('Ctrl Pts',(-7.88367768647865,1.03258941290634,8.19475114295154));
#27451=CARTESIAN_POINT('Ctrl Pts',(-9.03669748888875,1.07623385286206,8.24247316640641));
#27452=CARTESIAN_POINT('Ctrl Pts',(-9.58361051778681,0.288893050976006,
8.28224151928546));
#27453=CARTESIAN_POINT('Ctrl Pts',(-9.47724572542883,-0.401989773414212,
8.3140562015887));
#27454=CARTESIAN_POINT('Ctrl Pts',(-9.06669282573335,-0.967744899455822,
8.34587088389194));
#27455=CARTESIAN_POINT('Ctrl Pts',(-8.12407617387874,-1.14236805696769,
8.385639236771));
#27456=CARTESIAN_POINT('Ctrl Pts',(-7.3354977594041,-0.300047698604244,
8.43336126022585));
#27457=CARTESIAN_POINT('Ctrl Pts',(-7.61818561524077,0.816349017112872,
8.48108328368072));
#27458=CARTESIAN_POINT('Ctrl Pts',(-8.70950569765978,1.18414587464495,8.52880530713558));
#27459=CARTESIAN_POINT('Ctrl Pts',(-9.61003638925317,0.462755567399852,
8.57652733059045));
#27460=CARTESIAN_POINT('Ctrl Pts',(-9.50850068784772,-0.490507198490582,
8.61629568346948));
#27461=CARTESIAN_POINT('Ctrl Pts',(-8.97603188696186,-0.943397386255697,
8.64811036577274));
#27462=CARTESIAN_POINT('Ctrl Pts',(-8.2953882361285,-1.10263546797924,8.67992504807597));
#27463=CARTESIAN_POINT('Ctrl Pts',(-7.46827901092664,-0.617960598526543,
8.71969340095504));
#27464=CARTESIAN_POINT('Ctrl Pts',(-7.42302642728513,0.53499720883791,8.76741542440988));
#27465=CARTESIAN_POINT('Ctrl Pts',(-8.36724490293383,1.19431922496139,8.81513744786476));
#27466=CARTESIAN_POINT('Ctrl Pts',(-9.43320107257588,0.758439086501866,
8.86285947131961));
#27467=CARTESIAN_POINT('Ctrl Pts',(-9.64223992169735,-0.376312983972933,
8.91058149477448));
#27468=CARTESIAN_POINT('Ctrl Pts',(-8.94175347011682,-1.03078844619066,
8.95034984765353));
#27469=CARTESIAN_POINT('Ctrl Pts',(-8.24275566496688,-1.02490503847523,
8.98216452995676));
#27470=CARTESIAN_POINT('Ctrl Pts',(-7.62383052256787,-0.699998568553337,
9.01397921226003));
#27471=CARTESIAN_POINT('Ctrl Pts',(-7.315438978406,0.207698547770401,9.05374756513905));
#27472=CARTESIAN_POINT('Ctrl Pts',(-8.03557255959679,1.10923452993093,9.10146958859394));
#27473=CARTESIAN_POINT('Ctrl Pts',(-9.18102141880938,0.990066742210993,
9.14919161204878));
#27474=CARTESIAN_POINT('Ctrl Pts',(-9.70196712207443,-0.0370017194560962,
9.19691363550366));
#27475=CARTESIAN_POINT('Ctrl Pts',(-9.11760907802098,-1.03193145478362,
9.24463565895851));
#27476=CARTESIAN_POINT('Ctrl Pts',(-8.15965436942419,-1.06856717192152,
9.28440401183757));
#27477=CARTESIAN_POINT('Ctrl Pts',(-7.63488434792032,-0.606778290914648,
9.3162186941408));
#27478=CARTESIAN_POINT('Ctrl Pts',(-7.37939961054365,0.0438829842956811,
9.34803337644406));
#27479=CARTESIAN_POINT('Ctrl Pts',(-7.74006457714768,0.932106031371996,
9.38780172932309));
#27480=CARTESIAN_POINT('Ctrl Pts',(-8.87452398480516,1.1427273841981,9.43552375277797));
#27481=CARTESIAN_POINT('Ctrl Pts',(-9.66280451573322,0.303163297745353,
9.48324577623282));
#27482=CARTESIAN_POINT('Ctrl Pts',(-9.38478218192171,-0.814404432910586,
9.53096779968769));
#27483=CARTESIAN_POINT('Ctrl Pts',(-8.29189791040081,-1.18449019452684,
9.57868982314254));
#27484=CARTESIAN_POINT('Ctrl Pts',(-7.54347150337463,-0.585426497780913,
9.61845817602161));
#27485=CARTESIAN_POINT('Ctrl Pts',(-7.44875116596018,0.10714884380356,9.65027285832483));
#27486=CARTESIAN_POINT('Ctrl Pts',(-7.68125394638234,0.766371873730981,
9.6820875406281));
#27487=CARTESIAN_POINT('Ctrl Pts',(-8.5351536477378,1.20211801487063,9.72185589350713));
#27488=CARTESIAN_POINT('Ctrl Pts',(-9.5308974546648,0.619148227612896,9.769577916962));
#27489=CARTESIAN_POINT('Ctrl Pts',(-9.57772813351517,-0.531530241039361,
9.81729994041686));
#27490=CARTESIAN_POINT('Ctrl Pts',(-8.63627180399159,-1.19479039384633,
9.86502196387173));
#27491=CARTESIAN_POINT('Ctrl Pts',(-7.56763512943757,-0.759617830732582,
9.91274398732659));
#27492=CARTESIAN_POINT('Ctrl Pts',(-7.3935899270475,0.183105706163565,9.95251234020563));
#27493=CARTESIAN_POINT('Ctrl Pts',(-7.77509480916662,0.768841628751572,
9.98432702250888));
#27494=CARTESIAN_POINT('Ctrl Pts',(-8.38224154600145,1.11525956425949,10.0161417048121));
#27495=CARTESIAN_POINT('Ctrl Pts',(-9.31310554851392,0.886105449481985,
10.0559100576912));
#27496=CARTESIAN_POINT('Ctrl Pts',(-9.68471526164804,-0.206261578120577,
10.103632081146));
#27497=CARTESIAN_POINT('Ctrl Pts',(-8.96726644348741,-1.10710631725235,
10.1513541046009));
#27498=CARTESIAN_POINT('Ctrl Pts',(-7.82132982660755,-0.992723972480789,
10.1990761280558));
#27499=CARTESIAN_POINT('Ctrl Pts',(-7.29789403096364,0.0355631808608681,
10.2467981515106));
#27500=CARTESIAN_POINT('Ctrl Pts',(-7.7830759135267,0.862375094372996,10.2865665043897));
#27501=CARTESIAN_POINT('Ctrl Pts',(-8.45482491875085,1.05572922562212,10.3183811866929));
#27502=CARTESIAN_POINT('Ctrl Pts',(-9.14063560990152,0.920465623739701,
10.3501958689962));
#27503=CARTESIAN_POINT('Ctrl Pts',(-9.69467389428866,0.138122362168207,
10.3899642218752));
#27504=CARTESIAN_POINT('Ctrl Pts',(-9.2609922463669,-0.931120234319938,
10.4376862453301));
#27505=CARTESIAN_POINT('Ctrl Pts',(-8.12901546541348,-1.14297541618665,
10.4854082687849));
#27506=CARTESIAN_POINT('Ctrl Pts',(-7.33723505164926,-0.306711207290376,
10.5331302922398));
#27507=CARTESIAN_POINT('Ctrl Pts',(-7.61417160911282,0.813407377962594,
10.5808523156946));
#27508=CARTESIAN_POINT('Ctrl Pts',(-8.52205763101126,1.12124235117773,10.6206206685737));
#27509=CARTESIAN_POINT('Ctrl Pts',(-9.1565775804327,0.82795583618433,10.6524353508769));
#27510=CARTESIAN_POINT('Ctrl Pts',(-9.58672406848702,0.276950804532839,
10.6842500331802));
#27511=CARTESIAN_POINT('Ctrl Pts',(-9.49384665052284,-0.677194459420877,
10.7240183860592));
#27512=CARTESIAN_POINT('Ctrl Pts',(-8.46629056479243,-1.20206395993249,
10.7717404095141));
#27513=CARTESIAN_POINT('Ctrl Pts',(-7.47161698421242,-0.621651590321344,
10.819462432969));
#27514=CARTESIAN_POINT('Ctrl Pts',(-7.41998046699672,0.528821234560362,
10.8671844564238));
#27515=CARTESIAN_POINT('Ctrl Pts',(-8.36228464496208,1.19472088021117,10.9149064798787));
#27516=CARTESIAN_POINT('Ctrl Pts',(-9.25028639986432,0.833511408043712,
10.9546748327577));
#27517=CARTESIAN_POINT('Ctrl Pts',(-9.53825303203799,0.196559475127789,
10.986489515061));
#27518=CARTESIAN_POINT('Ctrl Pts',(-9.50304176070681,-0.501575692631294,
11.0183041973642));
#27519=CARTESIAN_POINT('Ctrl Pts',(-8.80852576484242,-1.162383479345,11.0580725502433));
#27520=CARTESIAN_POINT('Ctrl Pts',(-7.68802200901459,-0.88700948808109,
11.1057945736981));
#27521=CARTESIAN_POINT('Ctrl Pts',(-7.31554839363375,0.202723257387539,
11.153516597153));
#27522=CARTESIAN_POINT('Ctrl Pts',(-8.02922823218693,1.10655683650717,11.2012386206079));
#27523=CARTESIAN_POINT('Ctrl Pts',(-9.17753300181366,0.993615887593974,
11.2489606440627));
#27524=CARTESIAN_POINT('Ctrl Pts',(-9.6127555314957,0.139449188904468,11.2887289969418));
#27525=CARTESIAN_POINT('Ctrl Pts',(-9.41378702564638,-0.530658324686323,
11.320543679245));
#27526=CARTESIAN_POINT('Ctrl Pts',(-8.9303832558628,-1.03558737064206,11.3523583615483));
#27527=CARTESIAN_POINT('Ctrl Pts',(-7.97280061774567,-1.08091827257034,
11.3921267144273));
#27528=CARTESIAN_POINT('Ctrl Pts',(-7.30558733143117,-0.139543781491302,
11.4398487378822));
#27529=CARTESIAN_POINT('Ctrl Pts',(-7.73689209512053,0.928271863421417,
11.487570761337));
#27530=CARTESIAN_POINT('Ctrl Pts',(-8.86797410775294,1.1448533293894,11.5352927847919));
#27531=CARTESIAN_POINT('Ctrl Pts',(-9.66248851983205,0.308129748457519,
11.5830148082468));
#27532=CARTESIAN_POINT('Ctrl Pts',(-9.43276373142163,-0.622593583732446,
11.6227831611258));
#27533=CARTESIAN_POINT('Ctrl Pts',(-8.84385591278509,-0.999183715360338,
11.6545978434291));
#27534=CARTESIAN_POINT('Ctrl Pts',(-8.14791577199536,-1.06475708288359,
11.6864125257323));
#27535=CARTESIAN_POINT('Ctrl Pts',(-7.39408166832453,-0.472512586382552,
11.7261808786113));
#27536=CARTESIAN_POINT('Ctrl Pts',(-7.50542089758475,0.675948591854042,
11.7739029020662));
#27537=CARTESIAN_POINT('Ctrl Pts',(-8.53024583237525,1.20129410076524,11.8216249255211));
#27538=CARTESIAN_POINT('Ctrl Pts',(-9.52733504953497,0.625041427257073,
11.8693469489759));
#27539=CARTESIAN_POINT('Ctrl Pts',(-9.5807386046118,-0.527567596737633,
11.9170689724308));
#27540=CARTESIAN_POINT('Ctrl Pts',(-8.79805580683824,-1.08112611899371,
11.9568373253098));
#27541=CARTESIAN_POINT('Ctrl Pts',(-8.10629732601575,-0.980613680455361,
11.9886520076131));
#27542=CARTESIAN_POINT('Ctrl Pts',(-7.53708701106063,-0.574864788356556,
12.0204666899163));
#27543=CARTESIAN_POINT('Ctrl Pts',(-7.35449056110284,0.366239847672738,
12.0602350427954));
#27544=CARTESIAN_POINT('Ctrl Pts',(-8.19010517108621,1.16192051569936,12.1079570662502));
#27545=CARTESIAN_POINT('Ctrl Pts',(-9.30885492721204,0.888693441876452,
12.1556790897051));
#27546=CARTESIAN_POINT('Ctrl Pts',(-9.68587697728314,-0.199474019712831,
12.20340111316));
#27547=CARTESIAN_POINT('Ctrl Pts',(-8.97213579691505,-1.10607924214188,
12.2511231366148));
#27548=CARTESIAN_POINT('Ctrl Pts',(-8.01804765583374,-1.0126168510908,12.2908914894939));
#27549=CARTESIAN_POINT('Ctrl Pts',(-7.56066617820273,-0.484000988662495,
12.3227061717971));
#27550=CARTESIAN_POINT('Ctrl Pts',(-7.39567193745142,0.195270272771156,
12.3545208541003));
#27551=CARTESIAN_POINT('Ctrl Pts',(-7.87332769792352,1.02645278821577,12.3942892069794));
#27552=CARTESIAN_POINT('Ctrl Pts',(-9.02586111564668,1.08146390454855,12.4420112304343));
#27553=CARTESIAN_POINT('Ctrl Pts',(-9.6931526167034,0.142860631957331,12.4897332538892));
#27554=CARTESIAN_POINT('Ctrl Pts',(-9.26631175410989,-0.926747206795693,
12.537455277344));
#27555=CARTESIAN_POINT('Ctrl Pts',(-8.13336992371389,-1.14538460256293,
12.5851773007989));
#27556=CARTESIAN_POINT('Ctrl Pts',(-7.47298807192611,-0.450463593150824,
12.6249456536779));
#27557=CARTESIAN_POINT('Ctrl Pts',(-7.47295403032462,0.248558970813969,
12.6567603359812));
#27558=CARTESIAN_POINT('Ctrl Pts',(-7.79260946040346,0.87021237272846,12.6885750182844));
#27559=CARTESIAN_POINT('Ctrl Pts',(-8.69766342022542,1.1862768112589,12.7283433711635));
#27560=CARTESIAN_POINT('Ctrl Pts',(-9.60526325861529,0.473800822018835,
12.7760653946183));
#27561=CARTESIAN_POINT('Ctrl Pts',(-9.49579632937404,-0.672615787292102,
12.8237874180732));
#27562=CARTESIAN_POINT('Ctrl Pts',(-8.47317463994588,-1.20223728516817,
12.871509441528));
#27563=CARTESIAN_POINT('Ctrl Pts',(-7.47333377788248,-0.626322575825536,
12.9192314649829));
#27564=CARTESIAN_POINT('Ctrl Pts',(-7.42858998248594,0.331287674885324,
12.958999817862));
#27565=CARTESIAN_POINT('Ctrl Pts',(-7.88591997196862,0.859948082718679,
12.9908145001652));
#27566=CARTESIAN_POINT('Ctrl Pts',(-8.53439517357149,1.1209317201308,13.0226291824684));
#27567=CARTESIAN_POINT('Ctrl Pts',(-9.42563953786609,0.767798766972735,
13.0623975353475));
#27568=CARTESIAN_POINT('Ctrl Pts',(-9.64585690315083,-0.3648370146958,13.1101195588024));
#27569=CARTESIAN_POINT('Ctrl Pts',(-8.81299594463815,-1.16019647713199,
13.1578415822572));
#27570=CARTESIAN_POINT('Ctrl Pts',(-7.69311471065889,-0.891644671175397,
13.2055636057121));
#27571=CARTESIAN_POINT('Ctrl Pts',(-7.31379059716063,0.198067547168361,
13.2532856291669));
#27572=CARTESIAN_POINT('Ctrl Pts',(-7.90649716126405,0.951538401522895,
13.293053982046));
#27573=CARTESIAN_POINT('Ctrl Pts',(-8.59824584912319,1.0521182152822,13.3248686643492));
#27574=CARTESIAN_POINT('Ctrl Pts',(-9.25941346804454,0.82520429816681,13.3566833466525));
#27575=CARTESIAN_POINT('Ctrl Pts',(-9.70237252804341,-0.0249760771994319,
13.3964516995315));
#27576=CARTESIAN_POINT('Ctrl Pts',(-9.12785291712797,-1.0256192296581,13.4441737229864));
#27577=CARTESIAN_POINT('Ctrl Pts',(-7.97761211552232,-1.0821890893279,13.4918957464413));
#27578=CARTESIAN_POINT('Ctrl Pts',(-7.30640600133578,-0.146381201468398,
13.5396177698961));
#27579=CARTESIAN_POINT('Ctrl Pts',(-7.7325166226112,0.92590105630011,13.587339793351));
#27580=CARTESIAN_POINT('Ctrl Pts',(-8.67373303242592,1.10792047666089,13.62710814623));
#27581=CARTESIAN_POINT('Ctrl Pts',(-9.26267752728879,0.731387705097111,
13.6589228285333));
#27582=CARTESIAN_POINT('Ctrl Pts',(-9.61422274017161,0.127195261094417,
13.6907375108365));
#27583=CARTESIAN_POINT('Ctrl Pts',(-9.39295689585196,-0.805575249605032,
13.7305058637156));
#27584=CARTESIAN_POINT('Ctrl Pts',(-8.30377480362676,-1.18641888138164,
13.7782278871704));
#27585=CARTESIAN_POINT('Ctrl Pts',(-7.39688891086951,-0.476621707380971,
13.8259499106253));
#27586=CARTESIAN_POINT('Ctrl Pts',(-7.501566439608,0.670242131825176,13.8736719340801));
#27587=CARTESIAN_POINT('Ctrl Pts',(-8.52538569762017,1.20236394946876,13.921393957535));
#27588=CARTESIAN_POINT('Ctrl Pts',(-9.35627520405521,0.724198677215438,
13.9611623104141));
#27589=CARTESIAN_POINT('Ctrl Pts',(-9.55530897590372,0.0541105458815738,
13.9929769927173));
#27590=CARTESIAN_POINT('Ctrl Pts',(-9.42585582610759,-0.632820621047547,
14.0247916750206));
#27591=CARTESIAN_POINT('Ctrl Pts',(-8.64823070713109,-1.19346183771799,
14.0645600278996));
#27592=CARTESIAN_POINT('Ctrl Pts',(-7.57535517021029,-0.768847207534589,
14.1122820513545));
#27593=CARTESIAN_POINT('Ctrl Pts',(-7.35392503631861,0.361295591631145,
14.1600040748093));
#27594=CARTESIAN_POINT('Ctrl Pts',(-8.18345660789396,1.16012687698571,14.2077260982642));
#27595=CARTESIAN_POINT('Ctrl Pts',(-9.30587941362775,0.892682402266787,
14.2554481217191));
#27596=CARTESIAN_POINT('Ctrl Pts',(-9.62138890029986,-0.0125651679110466,
14.2952164745981));
#27597=CARTESIAN_POINT('Ctrl Pts',(-9.33348430715714,-0.649545145098795,
14.3270311569014));
#27598=CARTESIAN_POINT('Ctrl Pts',(-8.78614034549885,-1.08434065304129,
14.3588458392046));
#27599=CARTESIAN_POINT('Ctrl Pts',(-7.83124303309593,-0.99954370581937,
14.3986141920837));
#27600=CARTESIAN_POINT('Ctrl Pts',(-7.2976937506755,0.0235323740098842,
14.4463362155385));
#27601=CARTESIAN_POINT('Ctrl Pts',(-7.86966509538718,1.02308368911568,14.4940582389934));
#27602=CARTESIAN_POINT('Ctrl Pts',(-9.01965957764054,1.0844574741122,14.5417802624482));
#27603=CARTESIAN_POINT('Ctrl Pts',(-9.69351226740367,0.147824112333504,
14.5895022859031));
#27604=CARTESIAN_POINT('Ctrl Pts',(-9.33983295487833,-0.743203577124169,
14.6292706387821));
#27605=CARTESIAN_POINT('Ctrl Pts',(-8.7053415739125,-1.0365518915288,14.6610853210854));
#27606=CARTESIAN_POINT('Ctrl Pts',(-8.00693334672862,-1.00725181786108,
14.6929000033886));
#27607=CARTESIAN_POINT('Ctrl Pts',(-7.34026993918294,-0.318354655404035,
14.7326683562677));
#27608=CARTESIAN_POINT('Ctrl Pts',(-7.60614864303216,0.804440079539016,
14.7803903797225));
#27609=CARTESIAN_POINT('Ctrl Pts',(-8.69268923442672,1.18612528247478,14.8281124031774));
#27610=CARTESIAN_POINT('Ctrl Pts',(-9.60253195424284,0.480122254696041,
14.8758344266322));
#27611=CARTESIAN_POINT('Ctrl Pts',(-9.49931581731957,-0.669097450884765,
14.9235564500871));
#27612=CARTESIAN_POINT('Ctrl Pts',(-8.64886402084744,-1.11153517775476,
14.9633248029661));
#27613=CARTESIAN_POINT('Ctrl Pts',(-7.97709618774838,-0.918246475208985,
14.9951394852694));
#27614=CARTESIAN_POINT('Ctrl Pts',(-7.46809306529431,-0.439134409383918,
15.0269541675726));
#27615=CARTESIAN_POINT('Ctrl Pts',(-7.4146575515378,0.518030172478034,15.0667225204517));
#27616=CARTESIAN_POINT('Ctrl Pts',(-8.35035012993273,1.19318859338258,15.1144445439066));
#27617=CARTESIAN_POINT('Ctrl Pts',(-9.42177866202504,0.770938669116064,
15.1621665673614));
#27618=CARTESIAN_POINT('Ctrl Pts',(-9.64792730494328,-0.358269358952444,
15.2098885908163));
#27619=CARTESIAN_POINT('Ctrl Pts',(-8.81795958293278,-1.15983848287083,
15.2576106142711));
#27620=CARTESIAN_POINT('Ctrl Pts',(-7.88532479520075,-0.938000704162233,
15.2973789671502));
#27621=CARTESIAN_POINT('Ctrl Pts',(-7.50376303095584,-0.352302076284569,
15.3291936494535));
#27622=CARTESIAN_POINT('Ctrl Pts',(-7.43230033380396,0.343058292157666,
15.3610083317567));
#27623=CARTESIAN_POINT('Ctrl Pts',(-8.01814288331926,1.10187833907963,15.4007766846357));
#27624=CARTESIAN_POINT('Ctrl Pts',(-9.16750412307632,1.00026625060447,15.4484987080906));
#27625=CARTESIAN_POINT('Ctrl Pts',(-9.70150859744452,-0.0200766297906168,
15.4962207315455));
#27626=CARTESIAN_POINT('Ctrl Pts',(-9.13371290888423,-1.02200475985614,
15.5439427550003));
#27627=CARTESIAN_POINT('Ctrl Pts',(-7.98160573727265,-1.08517048015587,
15.5916647784552));
#27628=CARTESIAN_POINT('Ctrl Pts',(-7.4214259111463,-0.307189213773918,
15.6314331313343));
#27629=CARTESIAN_POINT('Ctrl Pts',(-7.51610178164494,0.385376694787397,
15.6632478136375));
#27630=CARTESIAN_POINT('Ctrl Pts',(-7.91697244650555,0.958038040322487,
15.6950624959408));
#27631=CARTESIAN_POINT('Ctrl Pts',(-8.85659756807664,1.14851359334971,15.7348308488197));
#27632=CARTESIAN_POINT('Ctrl Pts',(-9.65914155738177,0.319812236207544,
15.7825528722747));
#27633=CARTESIAN_POINT('Ctrl Pts',(-9.39571682675819,-0.801471685911283,
15.8302748957295));
#27634=CARTESIAN_POINT('Ctrl Pts',(-8.31018119647929,-1.18720590861515,
15.8779969191844));
#27635=CARTESIAN_POINT('Ctrl Pts',(-7.39870825395651,-0.482092567814215,
15.9257189426392));
#27636=CARTESIAN_POINT('Ctrl Pts',(-7.49888207502137,0.665597216138805,
15.9734409660941));
#27637=CARTESIAN_POINT('Ctrl Pts',(-8.51873041814767,1.20213901819083,16.0211629895489));
#27638=CARTESIAN_POINT('Ctrl Pts',(-9.52102419768294,0.634172756274771,
16.0688850130038));
#27639=CARTESIAN_POINT('Ctrl Pts',(-9.58620741064431,-0.5157930568929,16.1166070364587));
#27640=CARTESIAN_POINT('Ctrl Pts',(-8.65222970570018,-1.19292557033944,
16.1643290599136));
#27641=CARTESIAN_POINT('Ctrl Pts',(-7.75981223837764,-0.842543822233083,
16.2040974127926));
#27642=CARTESIAN_POINT('Ctrl Pts',(-7.46421470806744,-0.209092634934189,
16.2359120950958));
#27643=CARTESIAN_POINT('Ctrl Pts',(-7.49095487068437,0.48940290682626,16.2677267773991));
#27644=CARTESIAN_POINT('Ctrl Pts',(-8.17744624771311,1.15857095575367,16.3074951302781));
#27645=CARTESIAN_POINT('Ctrl Pts',(-9.30118867072826,0.896762228214262,
16.355217153733));
#27646=CARTESIAN_POINT('Ctrl Pts',(-9.6868182467658,-0.18838373056243,16.4029391771878));
#27647=CARTESIAN_POINT('Ctrl Pts',(-8.9841181888876,-1.1007833145585,16.4506612006427));
#27648=CARTESIAN_POINT('Ctrl Pts',(-7.83453304963084,-1.00173643888757,
16.4983832240976));
#27649=CARTESIAN_POINT('Ctrl Pts',(-7.38901196100714,-0.152895867269504,
16.5381515769766));
#27650=CARTESIAN_POINT('Ctrl Pts',(-7.5798625650184,0.519569006187027,16.5699662592799));
#27651=CARTESIAN_POINT('Ctrl Pts',(-8.05712461167899,1.03030690516145,16.6017809415831));
#27652=CARTESIAN_POINT('Ctrl Pts',(-9.01408915809622,1.08721476271011,16.6415492944621));
#27653=CARTESIAN_POINT('Ctrl Pts',(-9.69263777884286,0.15397778890258,16.6892713179171));
#27654=CARTESIAN_POINT('Ctrl Pts',(-9.27427785561657,-0.918975590320485,
16.7369933413719));
#27655=CARTESIAN_POINT('Ctrl Pts',(-8.14589768896835,-1.14921958576742,
16.7847153648267));
#27656=CARTESIAN_POINT('Ctrl Pts',(-7.34132275359406,-0.322165374757602,
16.8324373882816));
#27657=CARTESIAN_POINT('Ctrl Pts',(-7.55977535075367,0.611267993885054,
16.8722057411606));
#27658=CARTESIAN_POINT('Ctrl Pts',(-8.14408594319423,0.994952345727702,
16.9040204234639));
#27659=CARTESIAN_POINT('Ctrl Pts',(-8.83918220279198,1.0689370334114,16.9358351057671));
#27660=CARTESIAN_POINT('Ctrl Pts',(-9.60012329115488,0.485852082206321,
16.9756034586462));
#27661=CARTESIAN_POINT('Ctrl Pts',(-9.50268072865149,-0.663871558339279,
17.023325482101));
#27662=CARTESIAN_POINT('Ctrl Pts',(-8.48428382203488,-1.20157202386707,
17.0710475055559));
#27663=CARTESIAN_POINT('Ctrl Pts',(-7.480298800651,-0.637419449003703,17.1187695290108));
#27664=CARTESIAN_POINT('Ctrl Pts',(-7.41296046464096,0.514459472793085,
17.1664915524657));
#27665=CARTESIAN_POINT('Ctrl Pts',(-8.18889175657724,1.07744262493511,17.2062599053447));
#27666=CARTESIAN_POINT('Ctrl Pts',(-8.881815165691,0.985303082841596,17.2380745876479));
#27667=CARTESIAN_POINT('Ctrl Pts',(-9.45589064371805,0.586467412907256,
17.2698892699512));
#27668=CARTESIAN_POINT('Ctrl Pts',(-9.64985467091836,-0.352360236686092,
17.3096576228302));
#27669=CARTESIAN_POINT('Ctrl Pts',(-8.82392345937827,-1.15808794236697,
17.3573796462851));
#27670=CARTESIAN_POINT('Ctrl Pts',(-7.70195133285558,-0.898410068830963,
17.4051016697399));
#27671=CARTESIAN_POINT('Ctrl Pts',(-7.31179746852686,0.185118432340318,
17.4528236931948));
#27672=CARTESIAN_POINT('Ctrl Pts',(-8.01452273397517,1.10028874610208,17.5005457166497));
#27673=CARTESIAN_POINT('Ctrl Pts',(-8.96967136313036,1.01837113068638,17.5403140695287));
#27674=CARTESIAN_POINT('Ctrl Pts',(-9.43341203133604,0.495325110968304,
17.572128751832));
#27675=CARTESIAN_POINT('Ctrl Pts',(-9.60660874341056,-0.181901176927666,
17.6039434341352));
#27676=CARTESIAN_POINT('Ctrl Pts',(-9.13903953521102,-1.01879928006603,
17.6437117870143));
#27677=CARTESIAN_POINT('Ctrl Pts',(-7.98725565469605,-1.08774414553672,
17.6914338104691));
#27678=CARTESIAN_POINT('Ctrl Pts',(-7.30866226909047,-0.157279171604971,
17.739155833924));
#27679=CARTESIAN_POINT('Ctrl Pts',(-7.72253697950026,0.917412307278465,
17.7868778573789));
#27680=CARTESIAN_POINT('Ctrl Pts',(-8.85275194643118,1.14973456280779,17.8345998808337));
#27681=CARTESIAN_POINT('Ctrl Pts',(-9.52148929926934,0.462850473305008,
17.8743682337128));
#27682=CARTESIAN_POINT('Ctrl Pts',(-9.52997673057435,-0.236120563005232,
17.906182916016));
#27683=CARTESIAN_POINT('Ctrl Pts',(-9.21786242976372,-0.86159415103292,
17.9379975983193));
#27684=CARTESIAN_POINT('Ctrl Pts',(-8.31669687000343,-1.18858044034017,
17.9777659511983));
#27685=CARTESIAN_POINT('Ctrl Pts',(-7.40054731317204,-0.487132301554058,
18.0254879746532));
#27686=CARTESIAN_POINT('Ctrl Pts',(-7.49614243737496,0.660524277275207,
18.073209998108));
#27687=CARTESIAN_POINT('Ctrl Pts',(-8.51228454977271,1.2024737750269,18.1209320215629));
#27688=CARTESIAN_POINT('Ctrl Pts',(-9.51901692765617,0.638692415624239,
18.1686540450178));
#27689=CARTESIAN_POINT('Ctrl Pts',(-9.57533798580677,-0.318306715985504,
18.2084223978968));
#27690=CARTESIAN_POINT('Ctrl Pts',(-9.12443461381578,-0.852459030609261,
18.2402370802));
#27691=CARTESIAN_POINT('Ctrl Pts',(-8.47916294898904,-1.12126569842547,
18.2720517625033));
#27692=CARTESIAN_POINT('Ctrl Pts',(-7.5837132633384,-0.778936529406515,
18.3118201153824));
#27693=CARTESIAN_POINT('Ctrl Pts',(-7.3498148549232,0.350953304351522,18.3595421388372));
#27694=CARTESIAN_POINT('Ctrl Pts',(-8.17299650074059,1.1563265275784,18.4072641622921));
#27695=CARTESIAN_POINT('Ctrl Pts',(-9.29604348361364,0.901337263174473,
18.4549861857469));
#27696=CARTESIAN_POINT('Ctrl Pts',(-9.68851792402192,-0.183708042568584,
18.5027082092018));
#27697=CARTESIAN_POINT('Ctrl Pts',(-9.10496654566918,-0.944291495133526,
18.5424765620808));
#27698=CARTESIAN_POINT('Ctrl Pts',(-8.41448476974234,-1.05322938204008,
18.5742912443841));
#27699=CARTESIAN_POINT('Ctrl Pts',(-7.75062139220164,-0.834327664251033,
18.6061059266873));
#27700=CARTESIAN_POINT('Ctrl Pts',(-7.29741335566221,0.0104337666328781,
18.6458742795664));
#27701=CARTESIAN_POINT('Ctrl Pts',(-7.85979001642749,1.01795150509475,18.6935963030212));
#27702=CARTESIAN_POINT('Ctrl Pts',(-9.00926259833872,1.08842727494434,18.7413183264761));
#27703=CARTESIAN_POINT('Ctrl Pts',(-9.69173650578151,0.160804821377532,
18.789040349931));
#27704=CARTESIAN_POINT('Ctrl Pts',(-9.2786243254698,-0.91655205002906,18.8367623733858));
#27705=CARTESIAN_POINT('Ctrl Pts',(-8.33967793214922,-1.10994044151948,
18.8765307262649));
#27706=CARTESIAN_POINT('Ctrl Pts',(-7.746223032506,-0.740557404307124,18.9083454085681));
#27707=CARTESIAN_POINT('Ctrl Pts',(-7.38739693003254,-0.140660434591127,
18.9401600908714));
#27708=CARTESIAN_POINT('Ctrl Pts',(-7.59736645062633,0.79471767073023,18.9799284437504));
#27709=CARTESIAN_POINT('Ctrl Pts',(-8.68186329323757,1.1887051074019,19.0276504672053));
#27710=CARTESIAN_POINT('Ctrl Pts',(-9.59726656130047,0.489926954107713,
19.0753724906601));
#27711=CARTESIAN_POINT('Ctrl Pts',(-9.50646589579862,-0.658118902923217,
19.123094514115));
#27712=CARTESIAN_POINT('Ctrl Pts',(-8.48915653915779,-1.20258301999602,
19.1708165375699));
#27713=CARTESIAN_POINT('Ctrl Pts',(-7.65254526199483,-0.734500793868192,
19.2105848904489));
#27714=CARTESIAN_POINT('Ctrl Pts',(-7.44542256102972,-0.0668686100755817,
19.2423995727522));
#27715=CARTESIAN_POINT('Ctrl Pts',(-7.56655907558636,0.621577822794718,
19.2742142550554));
#27716=CARTESIAN_POINT('Ctrl Pts',(-8.33734740644836,1.19158198813036,19.3139826079345));
#27717=CARTESIAN_POINT('Ctrl Pts',(-9.41527942236304,0.779972864136537,
19.3617046313893));
#27718=CARTESIAN_POINT('Ctrl Pts',(-9.65036036266347,-0.347409503212236,
19.4094266548442));
#27719=CARTESIAN_POINT('Ctrl Pts',(-8.83054984563462,-1.15621403266934,
19.457148678299));
#27720=CARTESIAN_POINT('Ctrl Pts',(-7.704974867994,-0.902362754165209,19.5048707017539));
#27721=CARTESIAN_POINT('Ctrl Pts',(-7.37854114860306,-0.000996887084833204,
19.5446390546329));
#27722=CARTESIAN_POINT('Ctrl Pts',(-7.65872158751808,0.639418187488004,
19.5764537369362));
#27723=CARTESIAN_POINT('Ctrl Pts',(-8.20076747273577,1.0808010195163,19.6082684192394));
#27724=CARTESIAN_POINT('Ctrl Pts',(-9.15662042143786,1.00755799970849,19.6480367721185));
#27725=CARTESIAN_POINT('Ctrl Pts',(-9.70250291153056,-0.00899097053304161,
19.6957587955733));
#27726=CARTESIAN_POINT('Ctrl Pts',(-9.14266112686343,-1.01538613489058,
19.7434808190282));
#27727=CARTESIAN_POINT('Ctrl Pts',(-7.99349294093177,-1.09066249999925,
19.7912028424831));
#27728=CARTESIAN_POINT('Ctrl Pts',(-7.3083626688575,-0.162246638342256,
19.8389248659379));
#27729=CARTESIAN_POINT('Ctrl Pts',(-7.65124077756914,0.732992995531986,
19.878693218817));
#27730=CARTESIAN_POINT('Ctrl Pts',(-8.28213825309398,1.03399286507868,19.9105079011202));
#27731=CARTESIAN_POINT('Ctrl Pts',(-8.9808497396993,1.01314089690995,19.9423225834235));
#27732=CARTESIAN_POINT('Ctrl Pts',(-9.65579534164531,0.332356177702199,
19.9820909363025));
#27733=CARTESIAN_POINT('Ctrl Pts',(-9.40351421724518,-0.793571766777498,
20.0298129597574));
#27734=CARTESIAN_POINT('Ctrl Pts',(-8.32166885968162,-1.18836876907051,
20.0775349832122));
#27735=CARTESIAN_POINT('Ctrl Pts',(-7.40335486377068,-0.493420241756677,
20.1252570066671));
#27736=CARTESIAN_POINT('Ctrl Pts',(-7.49266575489391,0.656963636179604,
20.1729790301219));
#27737=CARTESIAN_POINT('Ctrl Pts',(-8.33770489079221,1.10965366069221,20.2127473830011));
#27738=CARTESIAN_POINT('Ctrl Pts',(-9.01176107344925,0.924502887773008,
20.2445620653043));
#27739=CARTESIAN_POINT('Ctrl Pts',(-9.52652095192111,0.451581315409929,
20.2763767476075));
#27740=CARTESIAN_POINT('Ctrl Pts',(-9.59152770853021,-0.504867073729894,
20.3161451004866));
#27741=CARTESIAN_POINT('Ctrl Pts',(-8.66406834236317,-1.1912915968917,20.3638671239414));
#27742=CARTESIAN_POINT('Ctrl Pts',(-7.58761183909353,-0.782029520380867,
20.4115891473963));
#27743=CARTESIAN_POINT('Ctrl Pts',(-7.34782400761312,0.344361107498901,
20.4593111708512));
#27744=CARTESIAN_POINT('Ctrl Pts',(-8.16803759563199,1.15590850101208,20.507033194306));
#27745=CARTESIAN_POINT('Ctrl Pts',(-9.10328679193923,0.945365535563934,
20.546801547185));
#27746=CARTESIAN_POINT('Ctrl Pts',(-9.49190376914431,0.364323892375815,
20.5786162294883));
#27747=CARTESIAN_POINT('Ctrl Pts',(-9.57177001728932,-0.330121158364715,
20.6104309117915));
#27748=CARTESIAN_POINT('Ctrl Pts',(-8.99514756642966,-1.09597097958138,
20.6501992646706));
#27749=CARTESIAN_POINT('Ctrl Pts',(-7.84464024017011,-1.0082646849842,20.6979212881254));
#27750=CARTESIAN_POINT('Ctrl Pts',(-7.29833798770444,0.0055439259737052,
20.7456433115803));
#27751=CARTESIAN_POINT('Ctrl Pts',(-7.85397129605098,1.0142687037785,20.7933653350352));
#27752=CARTESIAN_POINT('Ctrl Pts',(-9.00523890391058,1.09135564808224,20.8410873584901));
#27753=CARTESIAN_POINT('Ctrl Pts',(-9.57477038849185,0.320217990096556,
20.8808557113691));
#27754=CARTESIAN_POINT('Ctrl Pts',(-9.48849996469401,-0.373460581050405,
20.9126703936724));
#27755=CARTESIAN_POINT('Ctrl Pts',(-9.0945383169396,-0.950891759797607,
20.9444850759755));
#27756=CARTESIAN_POINT('Ctrl Pts',(-8.1573862740094,-1.15279631131811,20.9842534288547));
#27757=CARTESIAN_POINT('Ctrl Pts',(-7.34469566859739,-0.333715435113531,
21.0319754523094));
#27758=CARTESIAN_POINT('Ctrl Pts',(-7.59486638697568,0.790414745233752,
21.0796974757644));
#27759=CARTESIAN_POINT('Ctrl Pts',(-8.67505328733558,1.18972704280586,21.1274194992192));
#27760=CARTESIAN_POINT('Ctrl Pts',(-9.59613960186481,0.494774164492666,
21.1751415226741));
#27761=CARTESIAN_POINT('Ctrl Pts',(-9.52231055829104,-0.461033698949551,
21.2149098755531));
#27762=CARTESIAN_POINT('Ctrl Pts',(-9.00320899216289,-0.929185501396226,
21.2467245578564));
#27763=CARTESIAN_POINT('Ctrl Pts',(-8.32747313545848,-1.10810894327763,
21.2785392401596));
#27764=CARTESIAN_POINT('Ctrl Pts',(-7.48664689768428,-0.647641097100003,
21.3183075930387));
#27765=CARTESIAN_POINT('Ctrl Pts',(-7.40795428611476,0.503517873143993,
21.3660296164935));
#27766=CARTESIAN_POINT('Ctrl Pts',(-8.3326414115313,1.18996362540003,21.4137516399484));
#27767=CARTESIAN_POINT('Ctrl Pts',(-9.41079796358698,0.785201349538081,
21.4614736634033));
#27768=CARTESIAN_POINT('Ctrl Pts',(-9.65267952346093,-0.343006438452175,
21.5091956868581));
#27769=CARTESIAN_POINT('Ctrl Pts',(-8.97148112016971,-1.01753452151951,
21.5489640397372));
#27770=CARTESIAN_POINT('Ctrl Pts',(-8.27260697780362,-1.0319386606068,21.5807787220404));
#27771=CARTESIAN_POINT('Ctrl Pts',(-7.6445136546766,-0.725130375950133,
21.6125934043437));
#27772=CARTESIAN_POINT('Ctrl Pts',(-7.30991042897887,0.173234850917899,
21.6523617572227));
#27773=CARTESIAN_POINT('Ctrl Pts',(-8.00357793678801,1.09528956214643,21.7000837806776));
#27774=CARTESIAN_POINT('Ctrl Pts',(-9.15200263652367,1.00941314082768,21.7478058041324));
#27775=CARTESIAN_POINT('Ctrl Pts',(-9.70253468127204,-0.00210478704439917,
21.7955278275873));
#27776=CARTESIAN_POINT('Ctrl Pts',(-9.14729583240704,-1.01357368058483,
21.8432498510421));
#27777=CARTESIAN_POINT('Ctrl Pts',(-8.19080776710961,-1.07799402237706,
21.8830182039212));
#27778=CARTESIAN_POINT('Ctrl Pts',(-7.65285755162984,-0.63162857595897,
21.9148328862244));
#27779=CARTESIAN_POINT('Ctrl Pts',(-7.37859808588644,0.0113444340040694,
21.9466475685277));
#27780=CARTESIAN_POINT('Ctrl Pts',(-7.71333472266603,0.909659959579857,
21.9864159214067));
#27781=CARTESIAN_POINT('Ctrl Pts',(-8.84120404649836,1.15311486350827,22.0341379448616));
#27782=CARTESIAN_POINT('Ctrl Pts',(-9.65351690621254,0.336780453695434,
22.0818599683164));
#27783=CARTESIAN_POINT('Ctrl Pts',(-9.40804372796624,-0.788384853920802,
22.1295819917713));
#27784=CARTESIAN_POINT('Ctrl Pts',(-8.3263597217982,-1.1900304846565,22.1773040152262));
#27785=CARTESIAN_POINT('Ctrl Pts',(-7.56086357421315,-0.61293859637056,
22.2170723681052));
#27786=CARTESIAN_POINT('Ctrl Pts',(-7.44608444309555,0.076596244772818,
22.2488870504085));
#27787=CARTESIAN_POINT('Ctrl Pts',(-7.65935850290658,0.742288907720554,
22.2807017327117));
#27788=CARTESIAN_POINT('Ctrl Pts',(-8.50025311474624,1.20263187907136,22.3204700855908));
#27789=CARTESIAN_POINT('Ctrl Pts',(-9.5124954495042,0.648804326838139,22.3681921090456));
#27790=CARTESIAN_POINT('Ctrl Pts',(-9.59269934472105,-0.500030468027331,
22.4159141325005));
#27791=CARTESIAN_POINT('Ctrl Pts',(-8.67088748766811,-1.19033254023784,
22.4636361559554));
#27792=CARTESIAN_POINT('Ctrl Pts',(-7.59007209365373,-0.786355330545981,
22.5113581794102));
#27793=CARTESIAN_POINT('Ctrl Pts',(-7.38874215200747,0.150920324792225,
22.5511265322893));
#27794=CARTESIAN_POINT('Ctrl Pts',(-7.75308816941443,0.747480904859688,
22.5829412145925));
#27795=CARTESIAN_POINT('Ctrl Pts',(-8.3499260669922,1.11137246852348,22.6147558968957));
#27796=CARTESIAN_POINT('Ctrl Pts',(-9.28704811506866,0.909328744290342,
22.6545242497748));
#27797=CARTESIAN_POINT('Ctrl Pts',(-9.69020204494021,-0.171794010404042,
22.7022462732297));
#27798=CARTESIAN_POINT('Ctrl Pts',(-8.99919810938205,-1.09307985732919,
22.7499682966845));
#27799=CARTESIAN_POINT('Ctrl Pts',(-7.8504247320093,-1.01200101828279,22.7976903201394));
#27800=CARTESIAN_POINT('Ctrl Pts',(-7.29736827694888,0.000662824956886309,
22.8454123435943));
#27801=CARTESIAN_POINT('Ctrl Pts',(-7.75835155074568,0.841206589892776,
22.8851806964733));
#27802=CARTESIAN_POINT('Ctrl Pts',(-8.42420645284244,1.05397358790808,22.9169953787766));
#27803=CARTESIAN_POINT('Ctrl Pts',(-9.11365367676609,0.938669331634874,
22.9488100610797));
#27804=CARTESIAN_POINT('Ctrl Pts',(-9.69016238614474,0.172733885592879,
22.9885784139589));
#27805=CARTESIAN_POINT('Ctrl Pts',(-9.2876930476951,-0.908643908472059,
23.0363004374137));
#27806=CARTESIAN_POINT('Ctrl Pts',(-8.16234111093395,-1.15326007541409,
23.0840224608686));
#27807=CARTESIAN_POINT('Ctrl Pts',(-7.34662560561449,-0.340325720694794,
23.1317444843235));
#27808=CARTESIAN_POINT('Ctrl Pts',(-7.59093943845774,0.787357857695122,
23.1794665077782));
#27809=CARTESIAN_POINT('Ctrl Pts',(-8.48950964314851,1.12141022894101,23.2192348606574));
#27810=CARTESIAN_POINT('Ctrl Pts',(-9.13227358715871,0.846661146374397,
23.2510495429606));
#27811=CARTESIAN_POINT('Ctrl Pts',(-9.57822919443977,0.308371129352578,
23.2828642252638));
#27812=CARTESIAN_POINT('Ctrl Pts',(-9.51308039793912,-0.64806759519152,
23.3226325781429));
#27813=CARTESIAN_POINT('Ctrl Pts',(-8.5011889208313,-1.20253593553699,23.3703546015977));
#27814=CARTESIAN_POINT('Ctrl Pts',(-7.49009057848581,-0.651233665627234,
23.4180766250526));
#27815=CARTESIAN_POINT('Ctrl Pts',(-7.40508883683077,0.497256105601518,
23.4657986485074));
#27816=CARTESIAN_POINT('Ctrl Pts',(-8.32767158657437,1.1902211637137,23.5135206719624));
#27817=CARTESIAN_POINT('Ctrl Pts',(-9.22578171484917,0.854933828755763,
23.5532890248414));
#27818=CARTESIAN_POINT('Ctrl Pts',(-9.53211154671474,0.226607018727755,
23.5851037071447));
#27819=CARTESIAN_POINT('Ctrl Pts',(-9.51717514043059,-0.472255950571703,
23.6169183894479));
#27820=CARTESIAN_POINT('Ctrl Pts',(-8.84212844368635,-1.1529404271889,23.6566867423269));
#27821=CARTESIAN_POINT('Ctrl Pts',(-7.71410520295799,-0.91019968016524,
23.7044087657818));
#27822=CARTESIAN_POINT('Ctrl Pts',(-7.31016418213637,0.168264831257892,
23.7521307892367));
#27823=CARTESIAN_POINT('Ctrl Pts',(-7.99731398869925,1.09242888273476,23.7998528126915));
#27824=CARTESIAN_POINT('Ctrl Pts',(-9.14841269178917,1.01285955677601,23.8475748361464));
#27825=CARTESIAN_POINT('Ctrl Pts',(-9.60824002053544,0.171682864736176,
23.8873431890254));
#27826=CARTESIAN_POINT('Ctrl Pts',(-9.42880198158284,-0.503916525633289,
23.9191578713287));
#27827=CARTESIAN_POINT('Ctrl Pts',(-8.96025496060319,-1.02266139088192,
23.9509725536319));
#27828=CARTESIAN_POINT('Ctrl Pts',(-8.00439114523888,-1.09576245770156,
23.9907409065109));
#27829=CARTESIAN_POINT('Ctrl Pts',(-7.31013997945228,-0.174147125421988,
24.0384629299658));
#27830=CARTESIAN_POINT('Ctrl Pts',(-7.71027484520036,0.905735340365012,
24.0861849534207));
#27831=CARTESIAN_POINT('Ctrl Pts',(-8.83459523269867,1.15504983444261,24.1339069768756));
#27832=CARTESIAN_POINT('Ctrl Pts',(-9.65305691591741,0.34173564239159,24.1816290003304));
#27833=CARTESIAN_POINT('Ctrl Pts',(-9.45043867612152,-0.595262355682614,
24.2213973532095));
#27834=CARTESIAN_POINT('Ctrl Pts',(-8.87270761867775,-0.988784110298152,
24.2532120355127));
#27835=CARTESIAN_POINT('Ctrl Pts',(-8.17896354407182,-1.07452619471349,
24.285026717816));
#27836=CARTESIAN_POINT('Ctrl Pts',(-7.40825987210933,-0.504407567131031,
24.324795070695));
#27837=CARTESIAN_POINT('Ctrl Pts',(-7.48622361400777,0.646800996439465,
24.3725170941499));
#27838=CARTESIAN_POINT('Ctrl Pts',(-8.49537127660111,1.20166588610525,24.4202391176047));
#27839=CARTESIAN_POINT('Ctrl Pts',(-9.50876352283132,0.654591662638275,
24.4679611410596));
#27840=CARTESIAN_POINT('Ctrl Pts',(-9.59559355107939,-0.495982128164943,
24.5156831645145));
#27841=CARTESIAN_POINT('Ctrl Pts',(-8.82930478903784,-1.07202113089114,
24.5554515173935));
#27842=CARTESIAN_POINT('Ctrl Pts',(-8.13492076684851,-0.991626007787244,
24.5872661996968));
#27843=CARTESIAN_POINT('Ctrl Pts',(-7.5541752677766,-0.602566614636904,
24.619080882));
#27844=CARTESIAN_POINT('Ctrl Pts',(-7.34434466099276,0.332842662604764,
24.658849234879));
#27845=CARTESIAN_POINT('Ctrl Pts',(-8.15651650416419,1.15243792799395,24.7065712583339));
#27846=CARTESIAN_POINT('Ctrl Pts',(-9.2827241799191,0.911792292728668,24.7542932817887));
#27847=CARTESIAN_POINT('Ctrl Pts',(-9.69116629486312,-0.16497559750651,
24.8020153052437));
#27848=CARTESIAN_POINT('Ctrl Pts',(-9.00403560601477,-1.09191190509816,
24.8497373286984));
#27849=CARTESIAN_POINT('Ctrl Pts',(-8.04763700423772,-1.02617672416858,
24.8895056815775));
#27850=CARTESIAN_POINT('Ctrl Pts',(-7.57510761666008,-0.511056811947901,
24.9213203638808));
#27851=CARTESIAN_POINT('Ctrl Pts',(-7.39047026714238,0.163140188381993,
24.953135046184));
#27852=CARTESIAN_POINT('Ctrl Pts',(-7.8438037528424,1.00783430475553,24.9929033990631));
#27853=CARTESIAN_POINT('Ctrl Pts',(-8.99425531743911,1.09626902308409,25.0406254225179));
#27854=CARTESIAN_POINT('Ctrl Pts',(-9.68850424366054,0.177426011932626,
25.0883474459728));
#27855=CARTESIAN_POINT('Ctrl Pts',(-9.29288340878006,-0.904118349483034,
25.1360694694276));
#27856=CARTESIAN_POINT('Ctrl Pts',(-8.16676365035883,-1.15554187977053,
25.1837914928825));
#27857=CARTESIAN_POINT('Ctrl Pts',(-7.48649317569277,-0.480077979335733,
25.2235598457615));
#27858=CARTESIAN_POINT('Ctrl Pts',(-7.4661733610654,0.218649185746783,25.2553745280648));
#27859=CARTESIAN_POINT('Ctrl Pts',(-7.76765364280032,0.849317232991748,
25.287189210368));
#27860=CARTESIAN_POINT('Ctrl Pts',(-8.6631541573295,1.19151341644644,25.3269575632471));
#27861=CARTESIAN_POINT('Ctrl Pts',(-9.59104794585171,0.505676249831224,
25.3746795867019));
#27862=CARTESIAN_POINT('Ctrl Pts',(-9.51489638156947,-0.643434271380218,
25.4224016101568));
#27863=CARTESIAN_POINT('Ctrl Pts',(-8.50807512651903,-1.20250941040903,
25.4701236336117));
#27864=CARTESIAN_POINT('Ctrl Pts',(-7.49194220210365,-0.655852862101074,
25.5178456570665));
#27865=CARTESIAN_POINT('Ctrl Pts',(-7.41942719321752,0.300055592186921,
25.5576140099456));
#27866=CARTESIAN_POINT('Ctrl Pts',(-7.86122272622574,0.841765157456683,
25.5894286922488));
#27867=CARTESIAN_POINT('Ctrl Pts',(-8.50185100402222,1.12145776690186,25.6212433745521));
#27868=CARTESIAN_POINT('Ctrl Pts',(-9.40296799363835,0.794337650555834,
25.6610117274311));
#27869=CARTESIAN_POINT('Ctrl Pts',(-9.65596194639845,-0.331430336977873,
25.708733750886));
#27870=CARTESIAN_POINT('Ctrl Pts',(-8.84653327347151,-1.15062462049382,
25.7564557743408));
#27871=CARTESIAN_POINT('Ctrl Pts',(-7.71933027370747,-0.91468511972205,
25.8041777977958));
#27872=CARTESIAN_POINT('Ctrl Pts',(-7.30854223573027,0.163560070271257,
25.8518998212506));
#27873=CARTESIAN_POINT('Ctrl Pts',(-7.87913327787808,0.933914055211717,
25.8916681741297));
#27874=CARTESIAN_POINT('Ctrl Pts',(-8.56767177017992,1.05452620513634,25.9234828564328));
#27875=CARTESIAN_POINT('Ctrl Pts',(-9.23514601307596,0.846895087138279,
25.9552975387362));
#27876=CARTESIAN_POINT('Ctrl Pts',(-9.70259092973129,0.00992755527928493,
25.9950658916151));
#27877=CARTESIAN_POINT('Ctrl Pts',(-9.15735217491194,-1.00696683556567,
26.04278791507));
#27878=CARTESIAN_POINT('Ctrl Pts',(-8.00923749591142,-1.096893108507,26.0905099385249));
#27879=CARTESIAN_POINT('Ctrl Pts',(-7.31115672797335,-0.180957907667782,
26.1382319619798));
#27880=CARTESIAN_POINT('Ctrl Pts',(-7.70597001687183,0.903238554601866,
26.1859539854346));
#27881=CARTESIAN_POINT('Ctrl Pts',(-8.64150776634741,1.11249561851891,26.2257223383137));
#27882=CARTESIAN_POINT('Ctrl Pts',(-9.24113127558509,0.753212731005102,
26.2575370206169));
#27883=CARTESIAN_POINT('Ctrl Pts',(-9.61006222291879,0.159476676692902,
26.2893517029202));
#27884=CARTESIAN_POINT('Ctrl Pts',(-9.415958774083,-0.77932215726626,26.3291200557992));
#27885=CARTESIAN_POINT('Ctrl Pts',(-8.33828758368432,-1.19161368916269,
26.3768420792541));
#27886=CARTESIAN_POINT('Ctrl Pts',(-7.41118517990141,-0.508433490678091,
26.4245641027089));
#27887=CARTESIAN_POINT('Ctrl Pts',(-7.48253638214871,0.640985082618556,
26.4722861261638));
#27888=CARTESIAN_POINT('Ctrl Pts',(-8.49048214157161,1.20259424204372,26.5200081496186));
#27889=CARTESIAN_POINT('Ctrl Pts',(-9.33489815848678,0.748742955970736,
26.5597765024977));
#27890=CARTESIAN_POINT('Ctrl Pts',(-9.5532942060547,0.0847130526550384,
26.5915911848009));
#27891=CARTESIAN_POINT('Ctrl Pts',(-9.44383047110093,-0.605685554542794,
26.6234058671042));
#27892=CARTESIAN_POINT('Ctrl Pts',(-8.68280279902496,-1.18865749368541,
26.6631742199832));
#27893=CARTESIAN_POINT('Ctrl Pts',(-7.59805672146549,-0.795356782894942,
26.7108962434381));
#27894=CARTESIAN_POINT('Ctrl Pts',(-7.34392285778294,0.327884077308811,
26.758618266893));
#27895=CARTESIAN_POINT('Ctrl Pts',(-8.14992279296913,1.15045210196167,26.8063402903478));
#27896=CARTESIAN_POINT('Ctrl Pts',(-9.27963415904636,0.915693223014039,
26.8540623138027));
#27897=CARTESIAN_POINT('Ctrl Pts',(-9.62128124298946,0.0199830748488219,
26.8938306666817));
#27898=CARTESIAN_POINT('Ctrl Pts',(-9.35198320608394,-0.625083676278201,
26.925645348985));
#27899=CARTESIAN_POINT('Ctrl Pts',(-8.81748763267519,-1.07558010034525,
26.9574600312882));
#27900=CARTESIAN_POINT('Ctrl Pts',(-7.8605316734503,-1.01853019590265,26.9972283841673));
#27901=CARTESIAN_POINT('Ctrl Pts',(-7.2975172176546,-0.0113687269941268,
27.0449504076221));
#27902=CARTESIAN_POINT('Ctrl Pts',(-7.84024046489426,1.00436033511211,27.092672431077));
#27903=CARTESIAN_POINT('Ctrl Pts',(-8.98796951732628,1.09908136184312,27.1403944545319));
#27904=CARTESIAN_POINT('Ctrl Pts',(-9.68871970159898,0.18239783895712,27.1881164779867));
#27905=CARTESIAN_POINT('Ctrl Pts',(-9.36104716805341,-0.71851842255269,
27.2278848308658));
#27906=CARTESIAN_POINT('Ctrl Pts',(-8.73533605123604,-1.03015626425663,
27.259699513169));
#27907=CARTESIAN_POINT('Ctrl Pts',(-8.03637168178112,-1.02113649024308,
27.2915141954723));
#27908=CARTESIAN_POINT('Ctrl Pts',(-7.34999711030817,-0.351876191758067,
27.3312825483513));
#27909=CARTESIAN_POINT('Ctrl Pts',(-7.58318008445249,0.778161507815739,
27.3790045718062));
#27910=CARTESIAN_POINT('Ctrl Pts',(-8.65818646385365,1.19121759958578,27.426726595261));
#27911=CARTESIAN_POINT('Ctrl Pts',(-9.58813434263154,0.511915756913528,
27.4744486187159));
#27912=CARTESIAN_POINT('Ctrl Pts',(-9.51831228400498,-0.639815280272654,
27.5221706421708));
#27913=CARTESIAN_POINT('Ctrl Pts',(-8.68105831697462,-1.1067469606982,27.5619389950498));
#27914=CARTESIAN_POINT('Ctrl Pts',(-8.00396413429619,-0.933034514760314,
27.5937536773531));
#27915=CARTESIAN_POINT('Ctrl Pts',(-7.48127145702591,-0.468895622596703,
27.6255683596563));
#27916=CARTESIAN_POINT('Ctrl Pts',(-7.40008131862942,0.486315119030573,
27.6653367125354));
#27917=CARTESIAN_POINT('Ctrl Pts',(-8.31578657140523,1.18834317539839,27.7130587359902));
#27918=CARTESIAN_POINT('Ctrl Pts',(-9.39901761221339,0.797364195233005,
27.7607807594451));
#27919=CARTESIAN_POINT('Ctrl Pts',(-9.65784090229139,-0.324805379837842,
27.8085027828999));
#27920=CARTESIAN_POINT('Ctrl Pts',(-8.85148439065207,-1.15012269943416,
27.8562248063548));
#27921=CARTESIAN_POINT('Ctrl Pts',(-7.9128047387935,-0.955443705498678,
27.8959931592339));
#27922=CARTESIAN_POINT('Ctrl Pts',(-7.51440640767294,-0.381064635675364,
27.9278078415371));
#27923=CARTESIAN_POINT('Ctrl Pts',(-7.42279463151268,0.311928747092104,
27.9596225238404));
#27924=CARTESIAN_POINT('Ctrl Pts',(-7.9863685794706,1.08743103894948,27.9993908767193));
#27925=CARTESIAN_POINT('Ctrl Pts',(-9.13819588142177,1.01921543685667,28.0471129001743));
#27926=CARTESIAN_POINT('Ctrl Pts',(-9.70158364506713,0.0148010410636816,
28.0948349236291));
#27927=CARTESIAN_POINT('Ctrl Pts',(-9.16310771139847,-1.00318605097683,
28.142556947084));
#27928=CARTESIAN_POINT('Ctrl Pts',(-8.01331019109225,-1.09975294067858,
28.1902789705388));
#27929=CARTESIAN_POINT('Ctrl Pts',(-7.43080495083982,-0.338367989046775,
28.2300473234179));
#27930=CARTESIAN_POINT('Ctrl Pts',(-7.50531901190296,0.356671722620504,
28.2618620057211));
#27931=CARTESIAN_POINT('Ctrl Pts',(-7.88944826933002,0.940689924117418,
28.2936766880244));
#27932=CARTESIAN_POINT('Ctrl Pts',(-8.8230477467519,1.15843154909714,28.3334450409034));
#27933=CARTESIAN_POINT('Ctrl Pts',(-9.64948893755617,0.353226941538994,
28.3811670643583));
#27934=CARTESIAN_POINT('Ctrl Pts',(-9.41838563076225,-0.774977522329652,
28.4288890878132));
#27935=CARTESIAN_POINT('Ctrl Pts',(-8.34511391495364,-1.19252018450285,
28.476611111268));
#27936=CARTESIAN_POINT('Ctrl Pts',(-7.4123940412223,-0.513260926891183,
28.5243331347229));
#27937=CARTESIAN_POINT('Ctrl Pts',(-7.47003064875324,0.443659874939181,
28.5641014876019));
#27938=CARTESIAN_POINT('Ctrl Pts',(-7.98113199205868,0.920532984820785,
28.5959161699052));
#27939=CARTESIAN_POINT('Ctrl Pts',(-8.65374182116355,1.11087101034145,28.6277308522084));
#27940=CARTESIAN_POINT('Ctrl Pts',(-9.50224328279785,0.664704372278146,
28.6674992050875));
#27941=CARTESIAN_POINT('Ctrl Pts',(-9.60041377061406,-0.484957341939309,
28.7152212285423));
#27942=CARTESIAN_POINT('Ctrl Pts',(-8.68748072028854,-1.18695969033224,
28.7629432519972));
#27943=CARTESIAN_POINT('Ctrl Pts',(-7.60262605682145,-0.800508647597918,
28.810665275452));
#27944=CARTESIAN_POINT('Ctrl Pts',(-7.34167857245849,0.323442379934373,
28.8583872989069));
#27945=CARTESIAN_POINT('Ctrl Pts',(-8.01135956689715,1.00940649664747,28.8981556517859));
#27946=CARTESIAN_POINT('Ctrl Pts',(-8.70988967809667,1.03564052975447,28.9299703340892));
#27947=CARTESIAN_POINT('Ctrl Pts',(-9.3430872614141,0.739509857624331,28.9617850163924));
#27948=CARTESIAN_POINT('Ctrl Pts',(-9.69285186336733,-0.153061774255562,
29.0015533692715));
#27949=CARTESIAN_POINT('Ctrl Pts',(-9.01489421704395,-1.0867281375265,29.0492753927263));
#27950=CARTESIAN_POINT('Ctrl Pts',(-7.8651801697202,-1.02030689992113,29.0969974161812));
#27951=CARTESIAN_POINT('Ctrl Pts',(-7.29760210087134,-0.0182544462221305,
29.1447194396361));
#27952=CARTESIAN_POINT('Ctrl Pts',(-7.83563697930274,1.00246964476768,29.192441463091));
#27953=CARTESIAN_POINT('Ctrl Pts',(-8.79089767439502,1.08307420682354,29.23220981597));
#27954=CARTESIAN_POINT('Ctrl Pts',(-9.33632724182628,0.645880124738788,
29.2640244982732));
#27955=CARTESIAN_POINT('Ctrl Pts',(-9.62143398657489,0.00764272958403749,
29.2958391805765));
#27956=CARTESIAN_POINT('Ctrl Pts',(-9.3019515409739,-0.896211681488417,
29.3356075334555));
#27957=CARTESIAN_POINT('Ctrl Pts',(-8.17836973863726,-1.15872558044607,
29.3833295569104));
#27958=CARTESIAN_POINT('Ctrl Pts',(-7.35234534113202,-0.356262373711148,
29.4310515803652));
#27959=CARTESIAN_POINT('Ctrl Pts',(-7.57874808812184,0.772900762458947,
29.4787736038201));
#27960=CARTESIAN_POINT('Ctrl Pts',(-8.65345018277372,1.19279547618231,29.526495627275));
#27961=CARTESIAN_POINT('Ctrl Pts',(-9.42865613481405,0.628757665818371,
29.566263980154));
#27962=CARTESIAN_POINT('Ctrl Pts',(-9.55501939402632,-0.0587522064317555,
29.5980786624573));
#27963=CARTESIAN_POINT('Ctrl Pts',(-9.35318997184504,-0.727926671584861,
29.6298933447605));
#27964=CARTESIAN_POINT('Ctrl Pts',(-8.51989092266622,-1.2025142782169,29.6696616976397));
#27965=CARTESIAN_POINT('Ctrl Pts',(-7.4989974653622,-0.66576813704867,29.7173837210943));
#27966=CARTESIAN_POINT('Ctrl Pts',(-7.39832642452834,0.48130377881185,29.7651057445494));
#27967=CARTESIAN_POINT('Ctrl Pts',(-8.3102490425179,1.18756791113303,29.8128277680041));
#27968=CARTESIAN_POINT('Ctrl Pts',(-9.21331813028293,0.865450294731648,
29.8525961208832));
#27969=CARTESIAN_POINT('Ctrl Pts',(-9.52878251944959,0.241452561833112,
29.8844108031864));
#27970=CARTESIAN_POINT('Ctrl Pts',(-9.52368474853521,-0.457174338715818,
29.9162254854897));
#27971=CARTESIAN_POINT('Ctrl Pts',(-8.85937881967026,-1.1484426233223,29.9559938383687));
#27972=CARTESIAN_POINT('Ctrl Pts',(-7.72641809337258,-0.920473928895496,
30.0037158618236));
#27973=CARTESIAN_POINT('Ctrl Pts',(-7.3792747880128,-0.0294746800767998,
30.0434842147026));
#27974=CARTESIAN_POINT('Ctrl Pts',(-7.64321372550183,0.620692232781446,
30.0752988970059));
#27975=CARTESIAN_POINT('Ctrl Pts',(-7.90933322058758,0.844396458214266,
30.0912062381575));
#27976=CARTESIAN_POINT('Ctrl Pts',(-8.06214407575858,0.917335061595102,
30.0991599087333));
#27977=CARTESIAN_POINT('',(-7.9881611888325,1.07233375495115,30.));
#27978=CARTESIAN_POINT('Ctrl Pts',(-7.90984029786115,-0.827606761449162,
30.));
#27979=CARTESIAN_POINT('Ctrl Pts',(-7.79482765977711,-0.758933651579334,
30.));
#27980=CARTESIAN_POINT('Ctrl Pts',(-7.69456529374308,-0.668153006100937,
30.));
#27981=CARTESIAN_POINT('Ctrl Pts',(-7.53132804516273,-0.450356182128115,
30.));
#27982=CARTESIAN_POINT('Ctrl Pts',(-7.47119836686902,-0.324509106703349,
30.));
#27983=CARTESIAN_POINT('Ctrl Pts',(-7.40075075771614,-0.05295558696816,
30.));
#27984=CARTESIAN_POINT('Ctrl Pts',(-7.3926420328952,0.0905106217809897,
30.));
#27985=CARTESIAN_POINT('Ctrl Pts',(-7.43167638457232,0.376768385136799,
30.));
#27986=CARTESIAN_POINT('Ctrl Pts',(-7.48000224762515,0.516568235233513,
30.));
#27987=CARTESIAN_POINT('Ctrl Pts',(-7.60465705262832,0.731837239747291,
30.));
#27988=CARTESIAN_POINT('Ctrl Pts',(-7.66748861751526,0.812979534738878,
30.));
#27989=CARTESIAN_POINT('Ctrl Pts',(-7.81408314327503,0.958099062268137,
30.));
#27990=CARTESIAN_POINT('Ctrl Pts',(-7.89754686751452,1.02107277613379,30.));
#27991=CARTESIAN_POINT('Ctrl Pts',(-7.98816118883251,1.07233375495116,30.));
#27992=CARTESIAN_POINT('Ctrl Pts',(-7.98816118883246,1.07233375495113,30.));
#27993=CARTESIAN_POINT('Ctrl Pts',(-7.7185827492918,0.943660468883421,29.9879968132107));
#27994=CARTESIAN_POINT('Ctrl Pts',(-7.5011118191916,0.709457822903462,29.9759936264214));
#27995=CARTESIAN_POINT('Ctrl Pts',(-7.39273625402487,0.431098187741625,
29.9639904396321));
#27996=CARTESIAN_POINT('Ctrl Pts',(-7.28436068885813,0.152738552579788,
29.9519872528427));
#27997=CARTESIAN_POINT('Ctrl Pts',(-7.28621794011163,-0.166856559148227,
29.9399840660534));
#27998=CARTESIAN_POINT('Ctrl Pts',(-7.39782131852533,-0.443937838810512,
29.9279808792641));
#27999=CARTESIAN_POINT('Ctrl Pts',(-7.50942469693902,-0.721019118472796,
29.9159776924748));
#28000=CARTESIAN_POINT('Ctrl Pts',(-7.72960287363902,-0.952678470383577,
29.9039745056855));
#28001=CARTESIAN_POINT('Ctrl Pts',(-8.00065856416201,-1.07820998932502,
29.8919713188961));
#28002=CARTESIAN_POINT('Ctrl Pts',(-8.271714254685,-1.20374150826646,29.8799681321068));
#28003=CARTESIAN_POINT('Ctrl Pts',(-8.5908026046793,-1.22182768311292,29.8679649453175));
#28004=CARTESIAN_POINT('Ctrl Pts',(-8.87430710148917,-1.12772906515695,
29.8559617585282));
#28005=CARTESIAN_POINT('Ctrl Pts',(-9.15781159829903,-1.03363044720099,
29.8439585717389));
#28006=CARTESIAN_POINT('Ctrl Pts',(-9.40275673161545,-0.828334644790751,
29.8319553849496));
#28007=CARTESIAN_POINT('Ctrl Pts',(-9.54495508174642,-0.565639043699543,
29.8199521981602));
#28008=CARTESIAN_POINT('Ctrl Pts',(-9.63850099762682,-0.39282339162483,
29.8120558400052));
#28009=CARTESIAN_POINT('Ctrl Pts',(-9.68822500000028,-0.196509765607819,
29.8041594818502));
#28010=CARTESIAN_POINT('Ctrl Pts',(-9.688225,1.70996550252767E-12,29.7962631236951));
#28011=CARTESIAN_POINT('Origin',(-8.5,0.,30.));
#28012=CARTESIAN_POINT('Origin',(-8.5,0.,30.));
#28013=CARTESIAN_POINT('Origin',(-8.5,0.,1.8));
#28014=CARTESIAN_POINT('',(0.,0.,0.));
#28015=CARTESIAN_POINT('Origin',(-10.7,1.5,0.6));
#28016=CARTESIAN_POINT('',(-10.85,1.5,1.8));
#28017=CARTESIAN_POINT('Origin',(-10.7,1.5,1.8));
#28018=CARTESIAN_POINT('',(-10.85,1.5,0.6));
#28019=CARTESIAN_POINT('',(-10.85,1.5,0.6));
#28020=CARTESIAN_POINT('Origin',(-10.7,1.5,0.6));
#28021=CARTESIAN_POINT('Origin',(-10.7,1.5,1.8));
#28022=CARTESIAN_POINT('Origin',(-10.7,1.5,0.6));
#28023=CARTESIAN_POINT('',(0.,0.,0.));
#28024=CARTESIAN_POINT('Origin',(-6.3,-1.5,0.6));
#28025=CARTESIAN_POINT('',(-6.45,-1.5,1.8));
#28026=CARTESIAN_POINT('Origin',(-6.3,-1.5,1.8));
#28027=CARTESIAN_POINT('',(-6.45,-1.5,0.6));
#28028=CARTESIAN_POINT('',(-6.45,-1.5,0.6));
#28029=CARTESIAN_POINT('Origin',(-6.3,-1.5,0.6));
#28030=CARTESIAN_POINT('Origin',(-6.3,-1.5,1.8));
#28031=CARTESIAN_POINT('Origin',(-6.3,-1.5,0.6));
#28032=CARTESIAN_POINT('',(0.,0.,0.));
#28033=CARTESIAN_POINT('Origin',(0.,-1.1,18.));
#28034=CARTESIAN_POINT('',(1.09971587239614,-1.,17.975));
#28035=CARTESIAN_POINT('',(-1.09971587239614,-1.,17.975));
#28036=CARTESIAN_POINT('Origin',(0.,-1.,18.));
#28037=CARTESIAN_POINT('',(1.09971587239614,1.,17.975));
#28038=CARTESIAN_POINT('',(1.09971587239614,-1.1,17.975));
#28039=CARTESIAN_POINT('',(-1.09971587239614,1.,17.975));
#28040=CARTESIAN_POINT('Origin',(0.,1.,18.));
#28041=CARTESIAN_POINT('',(-1.09971587239614,-1.1,17.975));
#28042=CARTESIAN_POINT('Origin',(0.,1.,18.));
#28043=CARTESIAN_POINT('',(1.99984374389601,1.,17.975));
#28044=CARTESIAN_POINT('',(2.,1.,17.975));
#28045=CARTESIAN_POINT('',(0.8,1.,16.1669697220177));
#28046=CARTESIAN_POINT('Origin',(0.,1.,18.));
#28047=CARTESIAN_POINT('',(0.8,1.,16.2));
#28048=CARTESIAN_POINT('',(0.8,1.,17.1));
#28049=CARTESIAN_POINT('',(-0.8,1.,16.2));
#28050=CARTESIAN_POINT('',(-0.4,1.,16.2));
#28051=CARTESIAN_POINT('',(-0.8,1.,16.1669697220177));
#28052=CARTESIAN_POINT('',(-0.8,1.,16.5));
#28053=CARTESIAN_POINT('',(-1.99984374389601,1.,17.975));
#28054=CARTESIAN_POINT('Origin',(0.,1.,18.));
#28055=CARTESIAN_POINT('',(2.,1.,17.975));
#28056=CARTESIAN_POINT('Origin',(4.,-1.1,17.975));
#28057=CARTESIAN_POINT('',(1.99984374389601,-1.,17.975));
#28058=CARTESIAN_POINT('',(2.,-1.,17.975));
#28059=CARTESIAN_POINT('',(1.99984374389601,-1.,17.975));
#28060=CARTESIAN_POINT('Origin',(-8.5,0.,14.9));
#28061=CARTESIAN_POINT('',(-9.71,-1.4818226269683E-16,15.));
#28062=CARTESIAN_POINT('Origin',(-8.5,0.,15.));
#28063=CARTESIAN_POINT('',(-9.71,1.4818226269683E-16,16.2));
#28064=CARTESIAN_POINT('',(-9.71,-1.4818226269683E-16,14.9));
#28065=CARTESIAN_POINT('Origin',(-8.5,0.,16.2));
#28066=CARTESIAN_POINT('Origin',(-8.5,0.,15.));
#28067=CARTESIAN_POINT('',(-6.9,1.2,16.2));
#28068=CARTESIAN_POINT('',(-6.9,1.2,15.));
#28069=CARTESIAN_POINT('',(-6.9,1.2,15.));
#28070=CARTESIAN_POINT('',(-8.5,2.,16.2));
#28071=CARTESIAN_POINT('Origin',(-8.5,0.,16.2));
#28072=CARTESIAN_POINT('',(-8.5,2.,15.));
#28073=CARTESIAN_POINT('',(-8.5,2.,15.));
#28074=CARTESIAN_POINT('Origin',(-8.5,0.,15.));
#28075=CARTESIAN_POINT('Origin',(-4.25,1.2,15.6));
#28076=CARTESIAN_POINT('',(-0.8,1.2,15.));
#28077=CARTESIAN_POINT('',(-8.5,1.2,15.));
#28078=CARTESIAN_POINT('',(-0.8,1.2,16.2));
#28079=CARTESIAN_POINT('',(-0.8,1.2,15.3));
#28080=CARTESIAN_POINT('',(0.,1.2,16.2));
#28081=CARTESIAN_POINT('Origin',(0.8,-1.,15.));
#28082=CARTESIAN_POINT('',(-8.5,3.2,15.));
#28083=CARTESIAN_POINT('',(-8.5,1.2,15.));
#28084=CARTESIAN_POINT('',(0.8,3.2,15.));
#28085=CARTESIAN_POINT('',(-0.8,3.2,15.));
#28086=CARTESIAN_POINT('',(0.8,-1.,15.));
#28087=CARTESIAN_POINT('',(0.8,-1.,15.));
#28088=CARTESIAN_POINT('',(-0.8,-1.,15.));
#28089=CARTESIAN_POINT('',(-0.8,-1.,15.));
#28090=CARTESIAN_POINT('',(-0.8,-1.,15.));
#28091=CARTESIAN_POINT('Origin',(-8.5,1.2,15.));
#28092=CARTESIAN_POINT('',(-8.5,3.2,16.2));
#28093=CARTESIAN_POINT('',(-8.5,1.2,16.2));
#28094=CARTESIAN_POINT('',(-8.5,3.2,16.2));
#28095=CARTESIAN_POINT('Origin',(0.,3.2,15.6));
#28096=CARTESIAN_POINT('',(0.8,3.2,16.2));
#28097=CARTESIAN_POINT('',(0.,3.2,16.2));
#28098=CARTESIAN_POINT('',(0.8,3.2,15.));
#28099=CARTESIAN_POINT('Origin',(-0.8,-1.,16.2));
#28100=CARTESIAN_POINT('',(-0.8,-1.,16.2));
#28101=CARTESIAN_POINT('',(0.8,-1.,16.2));
#28102=CARTESIAN_POINT('Origin',(-0.8,-1.,15.));
#28103=CARTESIAN_POINT('',(-0.8,-1.,16.1669697220177));
#28104=CARTESIAN_POINT('',(-0.8,-1.,16.2));
#28105=CARTESIAN_POINT('',(-0.8,-1.,16.1669697220177));
#28106=CARTESIAN_POINT('Origin',(0.8,-1.,16.2));
#28107=CARTESIAN_POINT('',(0.8,-1.,16.1669697220177));
#28108=CARTESIAN_POINT('',(0.8,-1.,16.1669697220177));
#28109=CARTESIAN_POINT('',(0.8,-1.,15.));
#28110=CARTESIAN_POINT('Origin',(0.,-1.,18.));
#28111=CARTESIAN_POINT('',(-1.99984374389601,-1.,17.975));
#28112=CARTESIAN_POINT('',(2.,-1.,17.975));
#28113=CARTESIAN_POINT('Origin',(0.,-1.,18.));
#28114=CARTESIAN_POINT('Origin',(0.,-1.,18.));
#28115=CARTESIAN_POINT('Origin',(0.,-1.,18.));
#28116=CARTESIAN_POINT('Origin',(0.,-1.,18.));
#28117=CARTESIAN_POINT('',(-1.99984374389601,-1.,17.975));
#28118=CARTESIAN_POINT('Origin',(4.,-1.1,17.975));
#28119=CARTESIAN_POINT('Origin',(-3.,0.,16.7));
#28120=CARTESIAN_POINT('',(-3.425,-5.20474889637625E-17,16.8));
#28121=CARTESIAN_POINT('Origin',(-3.,0.,16.8));
#28122=CARTESIAN_POINT('',(-3.425,5.20474889637625E-17,17.975));
#28123=CARTESIAN_POINT('',(-3.425,-5.20474889637625E-17,16.7));
#28124=CARTESIAN_POINT('Origin',(-3.,0.,17.975));
#28125=CARTESIAN_POINT('Origin',(-4.,-1.,16.8));
#28126=CARTESIAN_POINT('',(-4.,-1.,17.975));
#28127=CARTESIAN_POINT('',(-4.,-1.,16.8));
#28128=CARTESIAN_POINT('',(-4.,-1.,17.975));
#28129=CARTESIAN_POINT('',(-4.,1.,17.975));
#28130=CARTESIAN_POINT('',(-4.,-1.,17.975));
#28131=CARTESIAN_POINT('',(-4.,1.,16.8));
#28132=CARTESIAN_POINT('',(-4.,1.,17.975));
#28133=CARTESIAN_POINT('',(-4.,-1.,16.8));
#28134=CARTESIAN_POINT('Origin',(-2.,-1.,16.8));
#28135=CARTESIAN_POINT('',(-2.,-1.,16.8));
#28136=CARTESIAN_POINT('',(-4.,-1.,16.8));
#28137=CARTESIAN_POINT('',(-2.,1.,16.8));
#28138=CARTESIAN_POINT('',(-4.,1.,16.8));
#28139=CARTESIAN_POINT('',(-2.,-1.,16.8));
#28140=CARTESIAN_POINT('Origin',(-2.,-1.,17.975));
#28141=CARTESIAN_POINT('',(-2.,-1.,17.975));
#28142=CARTESIAN_POINT('',(-2.,-1.,16.8));
#28143=CARTESIAN_POINT('',(-2.,1.,17.975));
#28144=CARTESIAN_POINT('',(-2.,1.,16.8));
#28145=CARTESIAN_POINT('',(-2.,-1.,17.975));
#28146=CARTESIAN_POINT('Origin',(-4.,-1.,17.975));
#28147=CARTESIAN_POINT('',(-2.,-1.,17.975));
#28148=CARTESIAN_POINT('',(-2.,1.,17.975));
#28149=CARTESIAN_POINT('Origin',(-3.,1.,17.3875));
#28150=CARTESIAN_POINT('Origin',(-3.,-1.,17.3875));
#28151=CARTESIAN_POINT('Origin',(3.,0.,16.7));
#28152=CARTESIAN_POINT('',(2.575,-5.20474889637625E-17,16.8));
#28153=CARTESIAN_POINT('Origin',(3.,0.,16.8));
#28154=CARTESIAN_POINT('',(2.575,5.20474889637625E-17,17.975));
#28155=CARTESIAN_POINT('',(2.575,-5.20474889637625E-17,16.7));
#28156=CARTESIAN_POINT('Origin',(3.,0.,17.975));
#28157=CARTESIAN_POINT('Origin',(2.,-1.,16.8));
#28158=CARTESIAN_POINT('',(2.,-1.,17.975));
#28159=CARTESIAN_POINT('',(2.,-1.,16.8));
#28160=CARTESIAN_POINT('',(2.,-1.,17.975));
#28161=CARTESIAN_POINT('',(2.,1.,17.975));
#28162=CARTESIAN_POINT('',(2.,-1.,17.975));
#28163=CARTESIAN_POINT('',(2.,1.,16.8));
#28164=CARTESIAN_POINT('',(2.,1.,17.975));
#28165=CARTESIAN_POINT('',(2.,-1.,16.8));
#28166=CARTESIAN_POINT('Origin',(4.,-1.,16.8));
#28167=CARTESIAN_POINT('',(4.,-1.,16.8));
#28168=CARTESIAN_POINT('',(2.,-1.,16.8));
#28169=CARTESIAN_POINT('',(4.,1.,16.8));
#28170=CARTESIAN_POINT('',(2.,1.,16.8));
#28171=CARTESIAN_POINT('',(4.,-1.,16.8));
#28172=CARTESIAN_POINT('Origin',(4.,-1.,17.975));
#28173=CARTESIAN_POINT('',(4.,-1.,17.975));
#28174=CARTESIAN_POINT('',(4.,-1.,16.8));
#28175=CARTESIAN_POINT('',(4.,1.,17.975));
#28176=CARTESIAN_POINT('',(4.,1.,16.8));
#28177=CARTESIAN_POINT('',(4.,-1.,17.975));
#28178=CARTESIAN_POINT('Origin',(2.,-1.,17.975));
#28179=CARTESIAN_POINT('',(4.,-1.,17.975));
#28180=CARTESIAN_POINT('',(4.,1.,17.975));
#28181=CARTESIAN_POINT('Origin',(3.,1.,17.3875));
#28182=CARTESIAN_POINT('Origin',(3.,-1.,17.3875));
#28183=CARTESIAN_POINT('',(0.,0.,0.));
#28184=CARTESIAN_POINT('Origin',(0.,-1.1,18.));
#28185=CARTESIAN_POINT('',(-1.09971587239614,1.,18.025));
#28186=CARTESIAN_POINT('',(-1.09971587239614,-1.,18.025));
#28187=CARTESIAN_POINT('',(-1.09971587239614,-1.1,18.025));
#28188=CARTESIAN_POINT('',(1.09971587239614,1.,18.025));
#28189=CARTESIAN_POINT('Origin',(0.,1.,18.));
#28190=CARTESIAN_POINT('',(1.09971587239614,-1.,18.025));
#28191=CARTESIAN_POINT('',(1.09971587239614,-1.1,18.025));
#28192=CARTESIAN_POINT('Origin',(0.,-1.,18.));
#28193=CARTESIAN_POINT('Origin',(0.,1.,18.));
#28194=CARTESIAN_POINT('',(-1.99984374389601,1.,18.025));
#28195=CARTESIAN_POINT('',(-2.,1.,18.025));
#28196=CARTESIAN_POINT('',(1.99984374389601,1.,18.025));
#28197=CARTESIAN_POINT('Origin',(0.,1.,18.));
#28198=CARTESIAN_POINT('',(-2.,1.,18.025));
#28199=CARTESIAN_POINT('Origin',(-4.,-1.1,18.025));
#28200=CARTESIAN_POINT('',(-1.99984374389601,-1.,18.025));
#28201=CARTESIAN_POINT('',(-2.,-1.,18.025));
#28202=CARTESIAN_POINT('',(-1.99984374389601,-1.,18.025));
#28203=CARTESIAN_POINT('Origin',(-4.,-1.1,18.025));
#28204=CARTESIAN_POINT('',(1.99984374389601,-1.,18.025));
#28205=CARTESIAN_POINT('',(1.99984374389601,-1.,18.025));
#28206=CARTESIAN_POINT('',(-2.,-1.,18.025));
#28207=CARTESIAN_POINT('Origin',(0.,-1.,18.));
#28208=CARTESIAN_POINT('Origin',(0.,-1.,18.));
#28209=CARTESIAN_POINT('Origin',(0.,-1.,18.));
#28210=CARTESIAN_POINT('Origin',(-3.,0.,16.7));
#28211=CARTESIAN_POINT('',(-3.425,-5.20474889637625E-17,18.025));
#28212=CARTESIAN_POINT('Origin',(-3.,0.,18.025));
#28213=CARTESIAN_POINT('',(-3.425,5.20474889637625E-17,19.2));
#28214=CARTESIAN_POINT('',(-3.425,-5.20474889637625E-17,16.7));
#28215=CARTESIAN_POINT('Origin',(-3.,0.,19.2));
#28216=CARTESIAN_POINT('Origin',(-4.,-1.,18.025));
#28217=CARTESIAN_POINT('',(-4.,-1.,19.2));
#28218=CARTESIAN_POINT('',(-4.,-1.,18.025));
#28219=CARTESIAN_POINT('',(-4.,-1.,19.2));
#28220=CARTESIAN_POINT('',(-4.,1.,19.2));
#28221=CARTESIAN_POINT('',(-4.,-1.,19.2));
#28222=CARTESIAN_POINT('',(-4.,1.,18.025));
#28223=CARTESIAN_POINT('',(-4.,1.,19.2));
#28224=CARTESIAN_POINT('',(-4.,-1.,18.025));
#28225=CARTESIAN_POINT('Origin',(-2.,-1.,18.025));
#28226=CARTESIAN_POINT('',(-2.,-1.,18.025));
#28227=CARTESIAN_POINT('',(-4.,-1.,18.025));
#28228=CARTESIAN_POINT('',(-2.,1.,18.025));
#28229=CARTESIAN_POINT('',(-4.,1.,18.025));
#28230=CARTESIAN_POINT('',(-2.,-1.,18.025));
#28231=CARTESIAN_POINT('Origin',(-2.,-1.,19.2));
#28232=CARTESIAN_POINT('',(-2.,-1.,19.2));
#28233=CARTESIAN_POINT('',(-2.,-1.,18.025));
#28234=CARTESIAN_POINT('',(-2.,1.,19.2));
#28235=CARTESIAN_POINT('',(-2.,1.,18.025));
#28236=CARTESIAN_POINT('',(-2.,-1.,19.2));
#28237=CARTESIAN_POINT('Origin',(-4.,-1.,19.2));
#28238=CARTESIAN_POINT('',(-2.,-1.,19.2));
#28239=CARTESIAN_POINT('',(-2.,1.,19.2));
#28240=CARTESIAN_POINT('Origin',(-3.,1.,18.6125));
#28241=CARTESIAN_POINT('Origin',(-3.,-1.,18.6125));
#28242=CARTESIAN_POINT('Origin',(3.,0.,16.7));
#28243=CARTESIAN_POINT('',(2.575,-5.20474889637625E-17,18.025));
#28244=CARTESIAN_POINT('Origin',(3.,0.,18.025));
#28245=CARTESIAN_POINT('',(2.575,5.20474889637625E-17,19.2));
#28246=CARTESIAN_POINT('',(2.575,-5.20474889637625E-17,16.7));
#28247=CARTESIAN_POINT('Origin',(3.,0.,19.2));
#28248=CARTESIAN_POINT('Origin',(2.,-1.,18.025));
#28249=CARTESIAN_POINT('',(2.,-1.,19.2));
#28250=CARTESIAN_POINT('',(2.,-1.,18.025));
#28251=CARTESIAN_POINT('',(2.,-1.,19.2));
#28252=CARTESIAN_POINT('',(2.,1.,19.2));
#28253=CARTESIAN_POINT('',(2.,-1.,19.2));
#28254=CARTESIAN_POINT('',(2.,1.,18.025));
#28255=CARTESIAN_POINT('',(2.,1.,19.2));
#28256=CARTESIAN_POINT('',(2.,-1.,18.025));
#28257=CARTESIAN_POINT('Origin',(4.,-1.,18.025));
#28258=CARTESIAN_POINT('',(4.,-1.,18.025));
#28259=CARTESIAN_POINT('',(2.,-1.,18.025));
#28260=CARTESIAN_POINT('',(4.,1.,18.025));
#28261=CARTESIAN_POINT('',(2.,1.,18.025));
#28262=CARTESIAN_POINT('',(4.,-1.,18.025));
#28263=CARTESIAN_POINT('Origin',(4.,-1.,19.2));
#28264=CARTESIAN_POINT('',(4.,-1.,19.2));
#28265=CARTESIAN_POINT('',(4.,-1.,18.025));
#28266=CARTESIAN_POINT('',(4.,1.,19.2));
#28267=CARTESIAN_POINT('',(4.,1.,18.025));
#28268=CARTESIAN_POINT('',(4.,-1.,19.2));
#28269=CARTESIAN_POINT('Origin',(2.,-1.,19.2));
#28270=CARTESIAN_POINT('',(4.,-1.,19.2));
#28271=CARTESIAN_POINT('',(4.,1.,19.2));
#28272=CARTESIAN_POINT('Origin',(3.,1.,18.6125));
#28273=CARTESIAN_POINT('Origin',(3.,-1.,18.6125));
#28274=CARTESIAN_POINT('',(0.,0.,0.));
#28275=CARTESIAN_POINT('Origin',(4.,-1.1,17.975));
#28276=CARTESIAN_POINT('',(1.09971587239614,1.,17.975));
#28277=CARTESIAN_POINT('',(1.09971587239614,-1.,17.975));
#28278=CARTESIAN_POINT('',(1.09971587239614,-1.,17.975));
#28279=CARTESIAN_POINT('',(0.99968745115661,1.,17.975));
#28280=CARTESIAN_POINT('',(2.,1.,17.975));
#28281=CARTESIAN_POINT('',(0.99968745115661,-1.,17.975));
#28282=CARTESIAN_POINT('',(0.99968745115661,-1.,17.975));
#28283=CARTESIAN_POINT('',(2.,-1.,17.975));
#28284=CARTESIAN_POINT('Origin',(4.,-1.1,17.975));
#28285=CARTESIAN_POINT('',(-1.09971587239614,-1.,17.975));
#28286=CARTESIAN_POINT('',(-1.09971587239614,1.,17.975));
#28287=CARTESIAN_POINT('',(-1.09971587239614,-1.,17.975));
#28288=CARTESIAN_POINT('',(-0.99968745115661,-1.,17.975));
#28289=CARTESIAN_POINT('',(2.,-1.,17.975));
#28290=CARTESIAN_POINT('',(-0.99968745115661,1.,17.975));
#28291=CARTESIAN_POINT('',(-0.99968745115661,-1.,17.975));
#28292=CARTESIAN_POINT('',(2.,1.,17.975));
#28293=CARTESIAN_POINT('Origin',(0.,-1.,18.));
#28294=CARTESIAN_POINT('Origin',(0.,-1.,18.));
#28295=CARTESIAN_POINT('Origin',(0.,-1.,18.));
#28296=CARTESIAN_POINT('Origin',(0.,-1.,18.));
#28297=CARTESIAN_POINT('Origin',(0.,1.,18.));
#28298=CARTESIAN_POINT('Origin',(0.,-1.,18.));
#28299=CARTESIAN_POINT('Origin',(0.,1.,18.));
#28300=CARTESIAN_POINT('Origin',(0.,1.,18.));
#28301=CARTESIAN_POINT('',(0.,0.,0.));
#28302=CARTESIAN_POINT('Origin',(-4.,-1.1,18.025));
#28303=CARTESIAN_POINT('',(-1.09971587239614,1.,18.025));
#28304=CARTESIAN_POINT('',(-1.09971587239614,-1.,18.025));
#28305=CARTESIAN_POINT('',(-1.09971587239614,-1.,18.025));
#28306=CARTESIAN_POINT('',(-0.99968745115661,1.,18.025));
#28307=CARTESIAN_POINT('',(-2.,1.,18.025));
#28308=CARTESIAN_POINT('',(-0.99968745115661,-1.,18.025));
#28309=CARTESIAN_POINT('',(-0.99968745115661,-1.,18.025));
#28310=CARTESIAN_POINT('',(-2.,-1.,18.025));
#28311=CARTESIAN_POINT('Origin',(-4.,-1.1,18.025));
#28312=CARTESIAN_POINT('',(1.09971587239614,-1.,18.025));
#28313=CARTESIAN_POINT('',(1.09971587239614,1.,18.025));
#28314=CARTESIAN_POINT('',(1.09971587239614,-1.,18.025));
#28315=CARTESIAN_POINT('',(0.99968745115661,-1.,18.025));
#28316=CARTESIAN_POINT('',(-2.,-1.,18.025));
#28317=CARTESIAN_POINT('',(0.99968745115661,1.,18.025));
#28318=CARTESIAN_POINT('',(0.99968745115661,-1.,18.025));
#28319=CARTESIAN_POINT('',(-2.,1.,18.025));
#28320=CARTESIAN_POINT('Origin',(0.,-1.,18.));
#28321=CARTESIAN_POINT('Origin',(0.,-1.,18.));
#28322=CARTESIAN_POINT('Origin',(0.,-1.,18.));
#28323=CARTESIAN_POINT('Origin',(0.,-1.,18.));
#28324=CARTESIAN_POINT('Origin',(0.,1.,18.));
#28325=CARTESIAN_POINT('Origin',(0.,-1.,18.));
#28326=CARTESIAN_POINT('Origin',(0.,1.,18.));
#28327=CARTESIAN_POINT('Origin',(0.,1.,18.));
#28328=CARTESIAN_POINT('',(0.,0.,0.));
#28329=CARTESIAN_POINT('Origin',(0.,-1.1,28.));
#28330=CARTESIAN_POINT('',(0.8,1.1,25.0050041736256));
#28331=CARTESIAN_POINT('',(0.8,1.,25.0050041736256));
#28332=CARTESIAN_POINT('',(0.8,-1.1,25.0050041736256));
#28333=CARTESIAN_POINT('',(-0.8,1.1,25.0050041736256));
#28334=CARTESIAN_POINT('Origin',(0.,1.1,28.));
#28335=CARTESIAN_POINT('',(-0.8,1.,25.0050041736256));
#28336=CARTESIAN_POINT('',(-0.8,-1.1,25.0050041736256));
#28337=CARTESIAN_POINT('',(-3.09989919190931,1.,27.975));
#28338=CARTESIAN_POINT('Origin',(0.,1.,28.));
#28339=CARTESIAN_POINT('',(-3.09989919190931,-1.,27.975));
#28340=CARTESIAN_POINT('',(-3.09989919190931,-1.1,27.975));
#28341=CARTESIAN_POINT('',(3.09989919190931,-1.,27.975));
#28342=CARTESIAN_POINT('Origin',(0.,-1.,28.));
#28343=CARTESIAN_POINT('',(3.09989919190931,1.,27.975));
#28344=CARTESIAN_POINT('',(3.09989919190931,-1.1,27.975));
#28345=CARTESIAN_POINT('Origin',(0.,1.,28.));
#28346=CARTESIAN_POINT('Origin',(0.,1.1,28.));
#28347=CARTESIAN_POINT('',(0.8,1.1,25.2));
#28348=CARTESIAN_POINT('',(0.8,1.1,26.6));
#28349=CARTESIAN_POINT('',(-0.8,1.1,25.2));
#28350=CARTESIAN_POINT('',(-0.4,1.1,25.2));
#28351=CARTESIAN_POINT('',(-0.8,1.1,26.));
#28352=CARTESIAN_POINT('Origin',(0.,-1.,28.));
#28353=CARTESIAN_POINT('',(-4.19992559457903,-1.,27.975));
#28354=CARTESIAN_POINT('',(4.2,-1.,27.975));
#28355=CARTESIAN_POINT('',(4.19992559457903,-1.,27.975));
#28356=CARTESIAN_POINT('Origin',(0.,-1.,28.));
#28357=CARTESIAN_POINT('',(4.2,-1.,27.975));
#28358=CARTESIAN_POINT('Origin',(8.4,-1.1,27.975));
#28359=CARTESIAN_POINT('',(-4.19992559457903,1.,27.975));
#28360=CARTESIAN_POINT('',(4.2,1.,27.975));
#28361=CARTESIAN_POINT('',(-4.19992559457903,-1.,27.975));
#28362=CARTESIAN_POINT('Origin',(-0.8,-1.,24.));
#28363=CARTESIAN_POINT('',(-0.8,1.2,25.2));
#28364=CARTESIAN_POINT('',(-0.8,-1.,25.2));
#28365=CARTESIAN_POINT('',(-0.8,1.2,24.));
#28366=CARTESIAN_POINT('',(-0.8,1.2,24.3));
#28367=CARTESIAN_POINT('',(-0.8,1.,24.));
#28368=CARTESIAN_POINT('',(-0.8,-1.,24.));
#28369=CARTESIAN_POINT('',(-0.8,1.,26.));
#28370=CARTESIAN_POINT('Origin',(-8.5,0.,23.9));
#28371=CARTESIAN_POINT('',(-9.71,-1.4818226269683E-16,24.));
#28372=CARTESIAN_POINT('Origin',(-8.5,0.,24.));
#28373=CARTESIAN_POINT('',(-9.71,1.4818226269683E-16,25.2));
#28374=CARTESIAN_POINT('',(-9.71,-1.4818226269683E-16,23.9));
#28375=CARTESIAN_POINT('Origin',(-8.5,0.,25.2));
#28376=CARTESIAN_POINT('Origin',(-8.5,0.,24.));
#28377=CARTESIAN_POINT('',(-6.9,1.2,25.2));
#28378=CARTESIAN_POINT('',(-6.9,1.2,24.));
#28379=CARTESIAN_POINT('',(-6.9,1.2,24.));
#28380=CARTESIAN_POINT('',(-8.5,2.,25.2));
#28381=CARTESIAN_POINT('Origin',(-8.5,0.,25.2));
#28382=CARTESIAN_POINT('',(-8.5,2.,24.));
#28383=CARTESIAN_POINT('',(-8.5,2.,24.));
#28384=CARTESIAN_POINT('Origin',(-8.5,0.,24.));
#28385=CARTESIAN_POINT('Origin',(-4.25,1.2,24.6));
#28386=CARTESIAN_POINT('',(-8.5,1.2,24.));
#28387=CARTESIAN_POINT('',(0.,1.2,25.2));
#28388=CARTESIAN_POINT('Origin',(0.8,-1.,24.));
#28389=CARTESIAN_POINT('',(-8.5,3.2,24.));
#28390=CARTESIAN_POINT('',(-8.5,1.2,24.));
#28391=CARTESIAN_POINT('',(0.8,3.2,24.));
#28392=CARTESIAN_POINT('',(-0.8,3.2,24.));
#28393=CARTESIAN_POINT('',(0.8,1.,24.));
#28394=CARTESIAN_POINT('',(0.8,-1.,24.));
#28395=CARTESIAN_POINT('',(0.4,1.,24.));
#28396=CARTESIAN_POINT('Origin',(-8.5,1.2,24.));
#28397=CARTESIAN_POINT('',(-8.5,3.2,25.2));
#28398=CARTESIAN_POINT('',(-8.5,1.2,25.2));
#28399=CARTESIAN_POINT('',(-8.5,3.2,25.2));
#28400=CARTESIAN_POINT('Origin',(0.,3.2,24.6));
#28401=CARTESIAN_POINT('',(0.8,3.2,25.2));
#28402=CARTESIAN_POINT('',(0.,3.2,25.2));
#28403=CARTESIAN_POINT('',(0.8,3.2,24.));
#28404=CARTESIAN_POINT('Origin',(-0.8,-1.,25.2));
#28405=CARTESIAN_POINT('',(0.8,-1.,25.2));
#28406=CARTESIAN_POINT('Origin',(0.8,-1.,25.2));
#28407=CARTESIAN_POINT('',(0.8,1.,26.6));
#28408=CARTESIAN_POINT('Origin',(8.4,-1.1,27.975));
#28409=CARTESIAN_POINT('',(4.19992559457903,1.,27.975));
#28410=CARTESIAN_POINT('',(4.19992559457903,-1.,27.975));
#28411=CARTESIAN_POINT('',(4.2,1.,27.975));
#28412=CARTESIAN_POINT('Origin',(0.,1.,28.));
#28413=CARTESIAN_POINT('Origin',(0.,1.,28.));
#28414=CARTESIAN_POINT('Origin',(0.,-1.,28.));
#28415=CARTESIAN_POINT('Origin',(-5.2,0.,26.7));
#28416=CARTESIAN_POINT('',(-5.625,-5.20474889637625E-17,26.8));
#28417=CARTESIAN_POINT('Origin',(-5.2,0.,26.8));
#28418=CARTESIAN_POINT('',(-5.625,5.20474889637625E-17,27.975));
#28419=CARTESIAN_POINT('',(-5.625,-5.20474889637625E-17,26.7));
#28420=CARTESIAN_POINT('Origin',(-5.2,0.,27.975));
#28421=CARTESIAN_POINT('Origin',(-6.2,-1.,26.8));
#28422=CARTESIAN_POINT('',(-6.2,-1.,27.975));
#28423=CARTESIAN_POINT('',(-6.2,-1.,26.8));
#28424=CARTESIAN_POINT('',(-6.2,-1.,27.975));
#28425=CARTESIAN_POINT('',(-6.2,1.,27.975));
#28426=CARTESIAN_POINT('',(-6.2,-1.,27.975));
#28427=CARTESIAN_POINT('',(-6.2,1.,26.8));
#28428=CARTESIAN_POINT('',(-6.2,1.,27.975));
#28429=CARTESIAN_POINT('',(-6.2,-1.,26.8));
#28430=CARTESIAN_POINT('Origin',(-4.2,-1.,26.8));
#28431=CARTESIAN_POINT('',(-4.2,-1.,26.8));
#28432=CARTESIAN_POINT('',(-6.2,-1.,26.8));
#28433=CARTESIAN_POINT('',(-4.2,1.,26.8));
#28434=CARTESIAN_POINT('',(-6.2,1.,26.8));
#28435=CARTESIAN_POINT('',(-4.2,-1.,26.8));
#28436=CARTESIAN_POINT('Origin',(-4.2,-1.,27.975));
#28437=CARTESIAN_POINT('',(-4.2,-1.,27.975));
#28438=CARTESIAN_POINT('',(-4.2,-1.,26.8));
#28439=CARTESIAN_POINT('',(-4.2,1.,27.975));
#28440=CARTESIAN_POINT('',(-4.2,1.,26.8));
#28441=CARTESIAN_POINT('',(-4.2,-1.,27.975));
#28442=CARTESIAN_POINT('Origin',(-6.2,-1.,27.975));
#28443=CARTESIAN_POINT('',(-4.2,-1.,27.975));
#28444=CARTESIAN_POINT('',(-4.2,1.,27.975));
#28445=CARTESIAN_POINT('Origin',(-5.2,1.,27.3875));
#28446=CARTESIAN_POINT('Origin',(-5.2,-1.,27.3875));
#28447=CARTESIAN_POINT('Origin',(5.2,0.,26.7));
#28448=CARTESIAN_POINT('',(4.775,-5.20474889637625E-17,26.8));
#28449=CARTESIAN_POINT('Origin',(5.2,0.,26.8));
#28450=CARTESIAN_POINT('',(4.775,5.20474889637625E-17,27.975));
#28451=CARTESIAN_POINT('',(4.775,-5.20474889637625E-17,26.7));
#28452=CARTESIAN_POINT('Origin',(5.2,0.,27.975));
#28453=CARTESIAN_POINT('Origin',(4.2,-1.,26.8));
#28454=CARTESIAN_POINT('',(4.2,-1.,27.975));
#28455=CARTESIAN_POINT('',(4.2,-1.,26.8));
#28456=CARTESIAN_POINT('',(4.2,-1.,27.975));
#28457=CARTESIAN_POINT('',(4.2,1.,27.975));
#28458=CARTESIAN_POINT('',(4.2,-1.,27.975));
#28459=CARTESIAN_POINT('',(4.2,1.,26.8));
#28460=CARTESIAN_POINT('',(4.2,1.,27.975));
#28461=CARTESIAN_POINT('',(4.2,-1.,26.8));
#28462=CARTESIAN_POINT('Origin',(6.2,-1.,26.8));
#28463=CARTESIAN_POINT('',(6.2,-1.,26.8));
#28464=CARTESIAN_POINT('',(4.2,-1.,26.8));
#28465=CARTESIAN_POINT('',(6.2,1.,26.8));
#28466=CARTESIAN_POINT('',(4.2,1.,26.8));
#28467=CARTESIAN_POINT('',(6.2,-1.,26.8));
#28468=CARTESIAN_POINT('Origin',(6.2,-1.,27.975));
#28469=CARTESIAN_POINT('',(6.2,-1.,27.975));
#28470=CARTESIAN_POINT('',(6.2,-1.,26.8));
#28471=CARTESIAN_POINT('',(6.2,1.,27.975));
#28472=CARTESIAN_POINT('',(6.2,1.,26.8));
#28473=CARTESIAN_POINT('',(6.2,-1.,27.975));
#28474=CARTESIAN_POINT('Origin',(4.2,-1.,27.975));
#28475=CARTESIAN_POINT('',(6.2,-1.,27.975));
#28476=CARTESIAN_POINT('',(6.2,1.,27.975));
#28477=CARTESIAN_POINT('Origin',(5.2,1.,27.3875));
#28478=CARTESIAN_POINT('Origin',(5.2,-1.,27.3875));
#28479=CARTESIAN_POINT('',(0.,0.,0.));
#28480=CARTESIAN_POINT('Origin',(0.,-1.1,28.));
#28481=CARTESIAN_POINT('',(-3.09989919190931,1.,28.025));
#28482=CARTESIAN_POINT('',(-3.09989919190931,-1.,28.025));
#28483=CARTESIAN_POINT('',(-3.09989919190931,-1.1,28.025));
#28484=CARTESIAN_POINT('',(3.09989919190931,1.,28.025));
#28485=CARTESIAN_POINT('Origin',(0.,1.,28.));
#28486=CARTESIAN_POINT('',(3.09989919190931,-1.,28.025));
#28487=CARTESIAN_POINT('',(3.09989919190931,-1.1,28.025));
#28488=CARTESIAN_POINT('Origin',(0.,-1.,28.));
#28489=CARTESIAN_POINT('Origin',(0.,1.,28.));
#28490=CARTESIAN_POINT('',(-4.19992559457903,1.,28.025));
#28491=CARTESIAN_POINT('',(-4.2,1.,28.025));
#28492=CARTESIAN_POINT('',(4.19992559457903,1.,28.025));
#28493=CARTESIAN_POINT('Origin',(0.,1.,28.));
#28494=CARTESIAN_POINT('',(-4.2,1.,28.025));
#28495=CARTESIAN_POINT('Origin',(-8.4,-1.1,28.025));
#28496=CARTESIAN_POINT('',(-4.19992559457903,-1.,28.025));
#28497=CARTESIAN_POINT('',(-4.2,-1.,28.025));
#28498=CARTESIAN_POINT('',(-4.19992559457903,-1.,28.025));
#28499=CARTESIAN_POINT('Origin',(-8.4,-1.1,28.025));
#28500=CARTESIAN_POINT('',(4.19992559457903,-1.,28.025));
#28501=CARTESIAN_POINT('',(4.19992559457903,-1.,28.025));
#28502=CARTESIAN_POINT('',(-4.2,-1.,28.025));
#28503=CARTESIAN_POINT('Origin',(0.,-1.,28.));
#28504=CARTESIAN_POINT('Origin',(0.,-1.,28.));
#28505=CARTESIAN_POINT('Origin',(0.,-1.,28.));
#28506=CARTESIAN_POINT('Origin',(-5.2,0.,26.7));
#28507=CARTESIAN_POINT('',(-5.625,-5.20474889637625E-17,28.025));
#28508=CARTESIAN_POINT('Origin',(-5.2,0.,28.025));
#28509=CARTESIAN_POINT('',(-5.625,5.20474889637625E-17,29.2));
#28510=CARTESIAN_POINT('',(-5.625,-5.20474889637625E-17,26.7));
#28511=CARTESIAN_POINT('Origin',(-5.2,0.,29.2));
#28512=CARTESIAN_POINT('Origin',(-6.2,-1.,28.025));
#28513=CARTESIAN_POINT('',(-6.2,-1.,29.2));
#28514=CARTESIAN_POINT('',(-6.2,-1.,28.025));
#28515=CARTESIAN_POINT('',(-6.2,-1.,29.2));
#28516=CARTESIAN_POINT('',(-6.2,1.,29.2));
#28517=CARTESIAN_POINT('',(-6.2,-1.,29.2));
#28518=CARTESIAN_POINT('',(-6.2,1.,28.025));
#28519=CARTESIAN_POINT('',(-6.2,1.,29.2));
#28520=CARTESIAN_POINT('',(-6.2,-1.,28.025));
#28521=CARTESIAN_POINT('Origin',(-4.2,-1.,28.025));
#28522=CARTESIAN_POINT('',(-4.2,-1.,28.025));
#28523=CARTESIAN_POINT('',(-6.2,-1.,28.025));
#28524=CARTESIAN_POINT('',(-4.2,1.,28.025));
#28525=CARTESIAN_POINT('',(-6.2,1.,28.025));
#28526=CARTESIAN_POINT('',(-4.2,-1.,28.025));
#28527=CARTESIAN_POINT('Origin',(-4.2,-1.,29.2));
#28528=CARTESIAN_POINT('',(-4.2,-1.,29.2));
#28529=CARTESIAN_POINT('',(-4.2,-1.,28.025));
#28530=CARTESIAN_POINT('',(-4.2,1.,29.2));
#28531=CARTESIAN_POINT('',(-4.2,1.,28.025));
#28532=CARTESIAN_POINT('',(-4.2,-1.,29.2));
#28533=CARTESIAN_POINT('Origin',(-6.2,-1.,29.2));
#28534=CARTESIAN_POINT('',(-4.2,-1.,29.2));
#28535=CARTESIAN_POINT('',(-4.2,1.,29.2));
#28536=CARTESIAN_POINT('Origin',(-5.2,1.,28.6125));
#28537=CARTESIAN_POINT('Origin',(-5.2,-1.,28.6125));
#28538=CARTESIAN_POINT('Origin',(5.2,0.,26.7));
#28539=CARTESIAN_POINT('',(4.775,-5.20474889637625E-17,28.025));
#28540=CARTESIAN_POINT('Origin',(5.2,0.,28.025));
#28541=CARTESIAN_POINT('',(4.775,5.20474889637625E-17,29.2));
#28542=CARTESIAN_POINT('',(4.775,-5.20474889637625E-17,26.7));
#28543=CARTESIAN_POINT('Origin',(5.2,0.,29.2));
#28544=CARTESIAN_POINT('Origin',(4.2,-1.,28.025));
#28545=CARTESIAN_POINT('',(4.2,-1.,29.2));
#28546=CARTESIAN_POINT('',(4.2,-1.,28.025));
#28547=CARTESIAN_POINT('',(4.2,-1.,29.2));
#28548=CARTESIAN_POINT('',(4.2,1.,29.2));
#28549=CARTESIAN_POINT('',(4.2,-1.,29.2));
#28550=CARTESIAN_POINT('',(4.2,1.,28.025));
#28551=CARTESIAN_POINT('',(4.2,1.,29.2));
#28552=CARTESIAN_POINT('',(4.2,-1.,28.025));
#28553=CARTESIAN_POINT('Origin',(6.2,-1.,28.025));
#28554=CARTESIAN_POINT('',(6.2,-1.,28.025));
#28555=CARTESIAN_POINT('',(4.2,-1.,28.025));
#28556=CARTESIAN_POINT('',(6.2,1.,28.025));
#28557=CARTESIAN_POINT('',(4.2,1.,28.025));
#28558=CARTESIAN_POINT('',(6.2,-1.,28.025));
#28559=CARTESIAN_POINT('Origin',(6.2,-1.,29.2));
#28560=CARTESIAN_POINT('',(6.2,-1.,29.2));
#28561=CARTESIAN_POINT('',(6.2,-1.,28.025));
#28562=CARTESIAN_POINT('',(6.2,1.,29.2));
#28563=CARTESIAN_POINT('',(6.2,1.,28.025));
#28564=CARTESIAN_POINT('',(6.2,-1.,29.2));
#28565=CARTESIAN_POINT('Origin',(4.2,-1.,29.2));
#28566=CARTESIAN_POINT('',(6.2,-1.,29.2));
#28567=CARTESIAN_POINT('',(6.2,1.,29.2));
#28568=CARTESIAN_POINT('Origin',(5.2,1.,28.6125));
#28569=CARTESIAN_POINT('Origin',(5.2,-1.,28.6125));
#28570=CARTESIAN_POINT('',(0.,0.,0.));
#28571=CARTESIAN_POINT('Origin',(8.4,-1.1,27.975));
#28572=CARTESIAN_POINT('',(3.09989919190931,1.,27.975));
#28573=CARTESIAN_POINT('',(3.09989919190931,-1.,27.975));
#28574=CARTESIAN_POINT('',(3.09989919190931,-1.,27.975));
#28575=CARTESIAN_POINT('',(2.99989583152482,1.,27.975));
#28576=CARTESIAN_POINT('',(4.2,1.,27.975));
#28577=CARTESIAN_POINT('',(2.99989583152482,-1.,27.975));
#28578=CARTESIAN_POINT('',(2.99989583152482,-1.,27.975));
#28579=CARTESIAN_POINT('',(4.2,-1.,27.975));
#28580=CARTESIAN_POINT('Origin',(8.4,-1.1,27.975));
#28581=CARTESIAN_POINT('',(-3.09989919190931,-1.,27.975));
#28582=CARTESIAN_POINT('',(-3.09989919190931,1.,27.975));
#28583=CARTESIAN_POINT('',(-3.09989919190931,-1.,27.975));
#28584=CARTESIAN_POINT('',(-2.99989583152482,-1.,27.975));
#28585=CARTESIAN_POINT('',(4.2,-1.,27.975));
#28586=CARTESIAN_POINT('',(-2.99989583152482,1.,27.975));
#28587=CARTESIAN_POINT('',(-2.99989583152482,-1.,27.975));
#28588=CARTESIAN_POINT('',(4.2,1.,27.975));
#28589=CARTESIAN_POINT('Origin',(0.,-1.,28.));
#28590=CARTESIAN_POINT('Origin',(0.,-1.,28.));
#28591=CARTESIAN_POINT('Origin',(0.,-1.,28.));
#28592=CARTESIAN_POINT('Origin',(0.,-1.,28.));
#28593=CARTESIAN_POINT('Origin',(0.,1.,28.));
#28594=CARTESIAN_POINT('Origin',(0.,-1.,28.));
#28595=CARTESIAN_POINT('Origin',(0.,1.,28.));
#28596=CARTESIAN_POINT('Origin',(0.,1.,28.));
#28597=CARTESIAN_POINT('',(0.,0.,0.));
#28598=CARTESIAN_POINT('Origin',(-8.4,-1.1,28.025));
#28599=CARTESIAN_POINT('',(-3.09989919190931,1.,28.025));
#28600=CARTESIAN_POINT('',(-3.09989919190931,-1.,28.025));
#28601=CARTESIAN_POINT('',(-3.09989919190931,-1.,28.025));
#28602=CARTESIAN_POINT('',(-2.99989583152482,1.,28.025));
#28603=CARTESIAN_POINT('',(-4.2,1.,28.025));
#28604=CARTESIAN_POINT('',(-2.99989583152482,-1.,28.025));
#28605=CARTESIAN_POINT('',(-2.99989583152482,-1.,28.025));
#28606=CARTESIAN_POINT('',(-4.2,-1.,28.025));
#28607=CARTESIAN_POINT('Origin',(-8.4,-1.1,28.025));
#28608=CARTESIAN_POINT('',(3.09989919190931,-1.,28.025));
#28609=CARTESIAN_POINT('',(3.09989919190931,1.,28.025));
#28610=CARTESIAN_POINT('',(3.09989919190931,-1.,28.025));
#28611=CARTESIAN_POINT('',(2.99989583152482,-1.,28.025));
#28612=CARTESIAN_POINT('',(-4.2,-1.,28.025));
#28613=CARTESIAN_POINT('',(2.99989583152482,1.,28.025));
#28614=CARTESIAN_POINT('',(2.99989583152482,-1.,28.025));
#28615=CARTESIAN_POINT('',(-4.2,1.,28.025));
#28616=CARTESIAN_POINT('Origin',(0.,-1.,28.));
#28617=CARTESIAN_POINT('Origin',(0.,-1.,28.));
#28618=CARTESIAN_POINT('Origin',(0.,-1.,28.));
#28619=CARTESIAN_POINT('Origin',(0.,-1.,28.));
#28620=CARTESIAN_POINT('Origin',(0.,1.,28.));
#28621=CARTESIAN_POINT('Origin',(0.,-1.,28.));
#28622=CARTESIAN_POINT('Origin',(0.,1.,28.));
#28623=CARTESIAN_POINT('Origin',(0.,1.,28.));
#28624=CARTESIAN_POINT('',(0.,0.,0.));
#28625=CARTESIAN_POINT('Origin',(-11.5,7.,-0.8));
#28626=CARTESIAN_POINT('',(-11.5,7.,-0.8));
#28627=CARTESIAN_POINT('',(-13.5,7.,-0.8));
#28628=CARTESIAN_POINT('',(-11.5,7.,-0.8));
#28629=CARTESIAN_POINT('',(-13.5,7.,0.));
#28630=CARTESIAN_POINT('',(-13.5,7.,-0.8));
#28631=CARTESIAN_POINT('',(-11.5,7.,0.));
#28632=CARTESIAN_POINT('',(-11.5,7.,0.));
#28633=CARTESIAN_POINT('',(-11.5,7.,-0.8));
#28634=CARTESIAN_POINT('Origin',(-11.5,-7.,-0.8));
#28635=CARTESIAN_POINT('',(-11.5,-7.,-0.8));
#28636=CARTESIAN_POINT('',(-11.5,-7.,-0.8));
#28637=CARTESIAN_POINT('',(-11.5,-7.,0.));
#28638=CARTESIAN_POINT('',(-11.5,-7.,0.));
#28639=CARTESIAN_POINT('',(-11.5,-7.,-0.8));
#28640=CARTESIAN_POINT('Origin',(-13.5,-7.,-0.8));
#28641=CARTESIAN_POINT('',(-13.5,-7.,-0.8));
#28642=CARTESIAN_POINT('',(-13.5,-7.,-0.8));
#28643=CARTESIAN_POINT('',(-13.5,-7.,0.));
#28644=CARTESIAN_POINT('',(-13.5,-7.,0.));
#28645=CARTESIAN_POINT('',(-13.5,-7.,-0.8));
#28646=CARTESIAN_POINT('Origin',(-13.5,7.,-0.8));
#28647=CARTESIAN_POINT('',(-13.5,7.,-0.8));
#28648=CARTESIAN_POINT('',(-13.5,7.,0.));
#28649=CARTESIAN_POINT('Origin',(-12.5,0.,0.));
#28650=CARTESIAN_POINT('Origin',(-12.5,0.,-0.8));
#28651=CARTESIAN_POINT('',(0.,0.,0.));
#28652=CARTESIAN_POINT('Origin',(6.5,7.,-0.8));
#28653=CARTESIAN_POINT('',(6.5,7.,-0.8));
#28654=CARTESIAN_POINT('',(4.5,7.,-0.8));
#28655=CARTESIAN_POINT('',(6.5,7.,-0.8));
#28656=CARTESIAN_POINT('',(4.5,7.,0.));
#28657=CARTESIAN_POINT('',(4.5,7.,-0.8));
#28658=CARTESIAN_POINT('',(6.5,7.,0.));
#28659=CARTESIAN_POINT('',(6.5,7.,0.));
#28660=CARTESIAN_POINT('',(6.5,7.,-0.8));
#28661=CARTESIAN_POINT('Origin',(6.5,-7.,-0.8));
#28662=CARTESIAN_POINT('',(6.5,-7.,-0.8));
#28663=CARTESIAN_POINT('',(6.5,-7.,-0.8));
#28664=CARTESIAN_POINT('',(6.5,-7.,0.));
#28665=CARTESIAN_POINT('',(6.5,-7.,0.));
#28666=CARTESIAN_POINT('',(6.5,-7.,-0.8));
#28667=CARTESIAN_POINT('Origin',(4.5,-7.,-0.8));
#28668=CARTESIAN_POINT('',(4.5,-7.,-0.8));
#28669=CARTESIAN_POINT('',(4.5,-7.,-0.8));
#28670=CARTESIAN_POINT('',(4.5,-7.,0.));
#28671=CARTESIAN_POINT('',(4.5,-7.,0.));
#28672=CARTESIAN_POINT('',(4.5,-7.,-0.8));
#28673=CARTESIAN_POINT('Origin',(4.5,7.,-0.8));
#28674=CARTESIAN_POINT('',(4.5,7.,-0.8));
#28675=CARTESIAN_POINT('',(4.5,7.,0.));
#28676=CARTESIAN_POINT('Origin',(5.5,0.,0.));
#28677=CARTESIAN_POINT('Origin',(5.5,0.,-0.8));
#28678=CARTESIAN_POINT('',(0.,0.,0.));
#28679=CARTESIAN_POINT('Origin',(0.144337567297406,-0.6,-0.25));
#28680=CARTESIAN_POINT('',(0.288675134594813,-0.6,0.));
#28681=CARTESIAN_POINT('',(0.144337567297406,-0.6,-0.25));
#28682=CARTESIAN_POINT('',(0.288675134594813,-0.6,0.));
#28683=CARTESIAN_POINT('',(0.144337567297406,-0.96,-0.25));
#28684=CARTESIAN_POINT('',(0.144337567297406,-0.6,-0.25));
#28685=CARTESIAN_POINT('',(0.288675134594813,-0.96,0.));
#28686=CARTESIAN_POINT('',(0.288675134594813,-0.96,0.));
#28687=CARTESIAN_POINT('',(0.288675134594813,-0.6,0.));
#28688=CARTESIAN_POINT('Origin',(-0.144337567297406,-0.6,-0.25));
#28689=CARTESIAN_POINT('',(-0.144337567297406,-0.6,-0.25));
#28690=CARTESIAN_POINT('',(0.144337567297406,-0.6,-0.25));
#28691=CARTESIAN_POINT('',(-0.144337567297406,-0.96,-0.25));
#28692=CARTESIAN_POINT('',(-0.144337567297406,-0.6,-0.25));
#28693=CARTESIAN_POINT('',(0.144337567297406,-0.96,-0.25));
#28694=CARTESIAN_POINT('Origin',(-0.288675134594813,-0.6,-8.32667268468867E-17));
#28695=CARTESIAN_POINT('',(-0.288675134594813,-0.6,-3.53525079574969E-17));
#28696=CARTESIAN_POINT('',(-0.144337567297406,-0.6,-0.25));
#28697=CARTESIAN_POINT('',(-0.288675134594813,-0.96,-5.55111512312578E-17));
#28698=CARTESIAN_POINT('',(-0.288675134594813,-0.6,-3.53525079574969E-17));
#28699=CARTESIAN_POINT('',(-0.144337567297406,-0.96,-0.25));
#28700=CARTESIAN_POINT('Origin',(-0.144337567297407,-0.6,0.25));
#28701=CARTESIAN_POINT('',(-0.144337567297407,-0.6,0.25));
#28702=CARTESIAN_POINT('',(-0.288675134594813,-0.6,-3.53525079574969E-17));
#28703=CARTESIAN_POINT('',(-0.144337567297407,-0.96,0.25));
#28704=CARTESIAN_POINT('',(-0.144337567297407,-0.6,0.25));
#28705=CARTESIAN_POINT('',(-0.288675134594813,-0.96,-3.53525079574969E-17));
#28706=CARTESIAN_POINT('Origin',(0.144337567297406,-0.6,0.25));
#28707=CARTESIAN_POINT('',(0.144337567297406,-0.6,0.25));
#28708=CARTESIAN_POINT('',(-0.144337567297407,-0.6,0.25));
#28709=CARTESIAN_POINT('',(0.144337567297406,-0.96,0.25));
#28710=CARTESIAN_POINT('',(0.144337567297406,-0.6,0.25));
#28711=CARTESIAN_POINT('',(-0.144337567297407,-0.96,0.25));
#28712=CARTESIAN_POINT('Origin',(0.288675134594813,-0.6,0.));
#28713=CARTESIAN_POINT('',(0.144337567297406,-0.6,0.25));
#28714=CARTESIAN_POINT('',(0.144337567297406,-0.96,0.25));
#28715=CARTESIAN_POINT('Origin',(0.,-0.6,0.));
#28716=CARTESIAN_POINT('Origin',(0.,-0.96,0.));
#28717=CARTESIAN_POINT('Origin',(0.,-1.8,0.));
#28718=CARTESIAN_POINT('',(-0.2942,-1.8,3.60291088309151E-17));
#28719=CARTESIAN_POINT('Origin',(0.,-1.8,0.));
#28720=CARTESIAN_POINT('Origin',(0.45,0.6,0.));
#28721=CARTESIAN_POINT('',(-0.45,0.6,-5.51091059616309E-17));
#28722=CARTESIAN_POINT('Origin',(0.,0.6,0.));
#28723=CARTESIAN_POINT('Origin',(0.,0.575,0.));
#28724=CARTESIAN_POINT('',(-0.5,0.55,-6.12323399573677E-17));
#28725=CARTESIAN_POINT('Origin',(0.,0.55,0.));
#28726=CARTESIAN_POINT('',(-0.475,0.575,-5.81707229594993E-17));
#28727=CARTESIAN_POINT('Origin',(0.,0.29,0.));
#28728=CARTESIAN_POINT('',(-0.5,0.0299999999999998,-6.12323399573677E-17));
#28729=CARTESIAN_POINT('Origin',(0.,0.0299999999999998,0.));
#28730=CARTESIAN_POINT('',(-0.5,0.29,-6.12323399573677E-17));
#28731=CARTESIAN_POINT('Origin',(0.,0.0150000000000001,0.));
#28732=CARTESIAN_POINT('',(-0.47,7.11236625150491E-17,-5.75583995599256E-17));
#28733=CARTESIAN_POINT('Origin',(0.,0.,0.));
#28734=CARTESIAN_POINT('',(-0.485,0.0150000000000001,-5.93953697586466E-17));
#28735=CARTESIAN_POINT('Origin',(0.32,0.,0.));
#28736=CARTESIAN_POINT('',(-0.32,-6.93889390390723E-18,-3.91886975727153E-17));
#28737=CARTESIAN_POINT('Origin',(0.,0.,0.));
#28738=CARTESIAN_POINT('Origin',(0.,-0.02,0.));
#28739=CARTESIAN_POINT('',(-0.2942,-0.0515999999999999,3.60291088309151E-17));
#28740=CARTESIAN_POINT('Origin',(0.,-0.0515999999999999,0.));
#28741=CARTESIAN_POINT('',(-0.31,-0.02,-3.7964050773568E-17));
#28742=CARTESIAN_POINT('Origin',(0.,-1.24,0.));
#28743=CARTESIAN_POINT('',(-0.2942,-1.24,-3.60291088309151E-17));
#28744=CARTESIAN_POINT('',(0.,0.,0.));
#28745=CARTESIAN_POINT('Origin',(0.173205080756888,-0.8,-0.3));
#28746=CARTESIAN_POINT('',(0.346410161513775,-0.8,0.));
#28747=CARTESIAN_POINT('',(0.173205080756888,-0.8,-0.3));
#28748=CARTESIAN_POINT('',(0.346410161513775,-0.8,0.));
#28749=CARTESIAN_POINT('',(0.173205080756888,-1.28,-0.3));
#28750=CARTESIAN_POINT('',(0.173205080756888,-0.8,-0.3));
#28751=CARTESIAN_POINT('',(0.346410161513775,-1.28,0.));
#28752=CARTESIAN_POINT('',(0.346410161513775,-1.28,0.));
#28753=CARTESIAN_POINT('',(0.346410161513775,-0.8,0.));
#28754=CARTESIAN_POINT('Origin',(-0.173205080756888,-0.8,-0.3));
#28755=CARTESIAN_POINT('',(-0.173205080756888,-0.8,-0.3));
#28756=CARTESIAN_POINT('',(0.173205080756888,-0.8,-0.3));
#28757=CARTESIAN_POINT('',(-0.173205080756888,-1.28,-0.3));
#28758=CARTESIAN_POINT('',(-0.173205080756888,-0.8,-0.3));
#28759=CARTESIAN_POINT('',(0.173205080756888,-1.28,-0.3));
#28760=CARTESIAN_POINT('Origin',(-0.346410161513775,-0.8,-5.55111512312578E-17));
#28761=CARTESIAN_POINT('',(-0.346410161513775,-0.8,-4.24230095489963E-17));
#28762=CARTESIAN_POINT('',(-0.173205080756888,-0.8,-0.3));
#28763=CARTESIAN_POINT('',(-0.346410161513775,-1.28,-5.55111512312578E-17));
#28764=CARTESIAN_POINT('',(-0.346410161513775,-0.8,-4.24230095489963E-17));
#28765=CARTESIAN_POINT('',(-0.173205080756888,-1.28,-0.3));
#28766=CARTESIAN_POINT('Origin',(-0.173205080756888,-0.8,0.3));
#28767=CARTESIAN_POINT('',(-0.173205080756888,-0.8,0.3));
#28768=CARTESIAN_POINT('',(-0.346410161513775,-0.8,-4.24230095489963E-17));
#28769=CARTESIAN_POINT('',(-0.173205080756888,-1.28,0.3));
#28770=CARTESIAN_POINT('',(-0.173205080756888,-0.8,0.3));
#28771=CARTESIAN_POINT('',(-0.346410161513775,-1.28,-4.24230095489963E-17));
#28772=CARTESIAN_POINT('Origin',(0.173205080756888,-0.8,0.3));
#28773=CARTESIAN_POINT('',(0.173205080756888,-0.8,0.3));
#28774=CARTESIAN_POINT('',(-0.173205080756888,-0.8,0.3));
#28775=CARTESIAN_POINT('',(0.173205080756888,-1.28,0.3));
#28776=CARTESIAN_POINT('',(0.173205080756888,-0.8,0.3));
#28777=CARTESIAN_POINT('',(-0.173205080756888,-1.28,0.3));
#28778=CARTESIAN_POINT('Origin',(0.346410161513775,-0.8,0.));
#28779=CARTESIAN_POINT('',(0.173205080756888,-0.8,0.3));
#28780=CARTESIAN_POINT('',(0.173205080756888,-1.28,0.3));
#28781=CARTESIAN_POINT('Origin',(0.,-0.8,-5.55111512312578E-17));
#28782=CARTESIAN_POINT('Origin',(0.,-1.28,-5.55111512312578E-17));
#28783=CARTESIAN_POINT('Origin',(0.,-2.9,0.));
#28784=CARTESIAN_POINT('',(-0.4,-2.9,4.89858719658941E-17));
#28785=CARTESIAN_POINT('Origin',(0.,-2.9,0.));
#28786=CARTESIAN_POINT('',(-0.3933,-2.9,4.81653586104654E-17));
#28787=CARTESIAN_POINT('Origin',(0.,-2.9,0.));
#28788=CARTESIAN_POINT('Origin',(0.,-4.,0.));
#28789=CARTESIAN_POINT('',(-0.4,-4.,4.89858719658941E-17));
#28790=CARTESIAN_POINT('',(-0.4,-4.,4.89858719658941E-17));
#28791=CARTESIAN_POINT('Origin',(0.,-4.,0.));
#28792=CARTESIAN_POINT('Origin',(0.,-4.,0.));
#28793=CARTESIAN_POINT('Origin',(0.6,0.8,0.));
#28794=CARTESIAN_POINT('',(-0.6,0.8,-7.34788079488412E-17));
#28795=CARTESIAN_POINT('Origin',(0.,0.8,0.));
#28796=CARTESIAN_POINT('Origin',(0.,0.775,0.));
#28797=CARTESIAN_POINT('',(-0.65,0.75,-7.9602041944578E-17));
#28798=CARTESIAN_POINT('Origin',(0.,0.75,0.));
#28799=CARTESIAN_POINT('',(-0.625,0.775,-7.65404249467096E-17));
#28800=CARTESIAN_POINT('Origin',(0.,0.39,0.));
#28801=CARTESIAN_POINT('',(-0.65,0.0299999999999998,-7.9602041944578E-17));
#28802=CARTESIAN_POINT('Origin',(0.,0.0299999999999998,0.));
#28803=CARTESIAN_POINT('',(-0.65,0.39,-7.9602041944578E-17));
#28804=CARTESIAN_POINT('Origin',(0.,0.0150000000000001,0.));
#28805=CARTESIAN_POINT('',(-0.62,5.89805981832114E-17,-7.59281015471359E-17));
#28806=CARTESIAN_POINT('Origin',(0.,0.,0.));
#28807=CARTESIAN_POINT('',(-0.635,0.0150000000000001,-7.77650717458569E-17));
#28808=CARTESIAN_POINT('Origin',(0.42,0.,0.));
#28809=CARTESIAN_POINT('',(-0.42,-3.46944695195361E-18,-5.14351655641888E-17));
#28810=CARTESIAN_POINT('Origin',(0.,0.,0.));
#28811=CARTESIAN_POINT('Origin',(0.,-0.02,0.));
#28812=CARTESIAN_POINT('',(-0.3933,-0.0534000000000001,4.81653586104654E-17));
#28813=CARTESIAN_POINT('Origin',(0.,-0.0534000000000001,0.));
#28814=CARTESIAN_POINT('',(-0.41,-0.02,-5.02105187650415E-17));
#28815=CARTESIAN_POINT('Origin',(0.,-1.48,0.));
#28816=CARTESIAN_POINT('',(-0.3933,-1.48,-4.81653586104654E-17));
#28817=CARTESIAN_POINT('',(0.,0.,0.));
#28818=CARTESIAN_POINT('Origin',(0.,0.,0.));
#28819=CARTESIAN_POINT('',(-0.42,0.16,5.14351655641888E-17));
#28820=CARTESIAN_POINT('Origin',(0.,0.16,0.));
#28821=CARTESIAN_POINT('',(-0.42,0.,5.14351655641888E-17));
#28822=CARTESIAN_POINT('',(-0.42,0.,5.14351655641888E-17));
#28823=CARTESIAN_POINT('Origin',(0.,0.,0.));
#28824=CARTESIAN_POINT('Origin',(0.,0.,0.));
#28825=CARTESIAN_POINT('',(-0.8,0.16,9.79717439317883E-17));
#28826=CARTESIAN_POINT('Origin',(0.,0.16,0.));
#28827=CARTESIAN_POINT('',(-0.8,0.,9.79717439317883E-17));
#28828=CARTESIAN_POINT('',(-0.8,0.,9.79717439317883E-17));
#28829=CARTESIAN_POINT('Origin',(0.,0.,0.));
#28830=CARTESIAN_POINT('Origin',(0.,0.16,0.));
#28831=CARTESIAN_POINT('Origin',(0.,0.,0.));
#28832=CARTESIAN_POINT('',(0.,0.,0.));
#28833=CARTESIAN_POINT('Origin',(0.,0.067277284513851,0.));
#28834=CARTESIAN_POINT('',(-0.375277674973257,0.0768195421087395,0.65));
#28835=CARTESIAN_POINT('',(0.375277674973257,0.0768195421087395,0.65));
#28836=CARTESIAN_POINT('Ctrl Pts',(-0.375277674973257,0.0768195421087395,
0.65));
#28837=CARTESIAN_POINT('Ctrl Pts',(1.66533453693773E-13,-0.0315137912242439,
0.65));
#28838=CARTESIAN_POINT('Ctrl Pts',(0.375277674973257,0.0768195421087394,
0.65));
#28839=CARTESIAN_POINT('',(-0.750555349946514,0.0768195421087394,-9.19165206894919E-17));
#28840=CARTESIAN_POINT('Ctrl Pts',(-0.750555349946514,0.0768195421087394,
-9.19165206894919E-17));
#28841=CARTESIAN_POINT('Ctrl Pts',(-0.562916512459802,-0.0315137912242434,
0.325000000000144));
#28842=CARTESIAN_POINT('Ctrl Pts',(-0.375277674973257,0.0768195421087395,
0.65));
#28843=CARTESIAN_POINT('',(-0.6175,-2.77555756156289E-17,-7.5621939847349E-17));
#28844=CARTESIAN_POINT('',(-0.734027674973257,0.067277284513851,-8.98924642641573E-17));
#28845=CARTESIAN_POINT('Origin',(0.,0.,0.));
#28846=CARTESIAN_POINT('',(-0.375277674973257,0.0768195421087395,-0.65));
#28847=CARTESIAN_POINT('Ctrl Pts',(-0.375277674973257,0.0768195421087395,
-0.65));
#28848=CARTESIAN_POINT('Ctrl Pts',(-0.562916512459968,-0.0315137912242437,
-0.324999999999856));
#28849=CARTESIAN_POINT('Ctrl Pts',(-0.750555349946514,0.0768195421087395,
-9.19165206894919E-17));
#28850=CARTESIAN_POINT('',(0.375277674973257,0.0768195421087395,-0.65));
#28851=CARTESIAN_POINT('Ctrl Pts',(0.375277674973257,0.0768195421087395,
-0.65));
#28852=CARTESIAN_POINT('Ctrl Pts',(-1.66144875635155E-13,-0.0315137912242437,
-0.65));
#28853=CARTESIAN_POINT('Ctrl Pts',(-0.375277674973257,0.0768195421087395,
-0.65));
#28854=CARTESIAN_POINT('',(0.750555349946514,0.0768195421087394,0.));
#28855=CARTESIAN_POINT('Ctrl Pts',(0.750555349946514,0.0768195421087394,
0.));
#28856=CARTESIAN_POINT('Ctrl Pts',(0.562916512459802,-0.0315137912242436,
-0.325000000000144));
#28857=CARTESIAN_POINT('Ctrl Pts',(0.375277674973257,0.0768195421087395,
-0.65));
#28858=CARTESIAN_POINT('Ctrl Pts',(0.375277674973257,0.0768195421087394,
0.65));
#28859=CARTESIAN_POINT('Ctrl Pts',(0.562916512459968,-0.0315137912242439,
0.324999999999856));
#28860=CARTESIAN_POINT('Ctrl Pts',(0.750555349946514,0.0768195421087394,
0.));
#28861=CARTESIAN_POINT('Origin',(0.,0.612722715486149,0.));
#28862=CARTESIAN_POINT('',(-0.6175,0.68,-7.5621939847349E-17));
#28863=CARTESIAN_POINT('Origin',(0.,0.68,0.));
#28864=CARTESIAN_POINT('',(-0.750555349946514,0.603180457891261,-9.19165206894919E-17));
#28865=CARTESIAN_POINT('',(-0.734027674973257,0.612722715486149,-8.98924642641573E-17));
#28866=CARTESIAN_POINT('',(-0.375277674973257,0.603180457891261,0.65));
#28867=CARTESIAN_POINT('Ctrl Pts',(-0.375277674973257,0.603180457891261,
0.65));
#28868=CARTESIAN_POINT('Ctrl Pts',(-0.562916512459968,0.711513791224243,
0.324999999999856));
#28869=CARTESIAN_POINT('Ctrl Pts',(-0.750555349946514,0.603180457891261,
-9.19165206894919E-17));
#28870=CARTESIAN_POINT('',(0.375277674973257,0.603180457891261,0.65));
#28871=CARTESIAN_POINT('Ctrl Pts',(0.375277674973257,0.603180457891261,
0.65));
#28872=CARTESIAN_POINT('Ctrl Pts',(-1.66755498298699E-13,0.711513791224244,
0.65));
#28873=CARTESIAN_POINT('Ctrl Pts',(-0.375277674973257,0.603180457891261,
0.65));
#28874=CARTESIAN_POINT('',(0.750555349946514,0.603180457891261,0.));
#28875=CARTESIAN_POINT('Ctrl Pts',(0.750555349946514,0.603180457891261,
0.));
#28876=CARTESIAN_POINT('Ctrl Pts',(0.562916512459802,0.711513791224244,
0.325000000000144));
#28877=CARTESIAN_POINT('Ctrl Pts',(0.375277674973257,0.603180457891261,
0.65));
#28878=CARTESIAN_POINT('',(0.375277674973257,0.603180457891261,-0.65));
#28879=CARTESIAN_POINT('Ctrl Pts',(0.375277674973257,0.603180457891261,
-0.65));
#28880=CARTESIAN_POINT('Ctrl Pts',(0.562916512459969,0.711513791224244,
-0.324999999999856));
#28881=CARTESIAN_POINT('Ctrl Pts',(0.750555349946514,0.603180457891261,
0.));
#28882=CARTESIAN_POINT('',(-0.375277674973257,0.603180457891261,-0.65));
#28883=CARTESIAN_POINT('Ctrl Pts',(-0.375277674973257,0.603180457891261,
-0.65));
#28884=CARTESIAN_POINT('Ctrl Pts',(1.66422431391311E-13,0.711513791224244,
-0.65));
#28885=CARTESIAN_POINT('Ctrl Pts',(0.375277674973257,0.603180457891261,
-0.65));
#28886=CARTESIAN_POINT('Ctrl Pts',(-0.750555349946514,0.603180457891261,
-9.19165206894919E-17));
#28887=CARTESIAN_POINT('Ctrl Pts',(-0.562916512459802,0.711513791224244,
-0.325000000000144));
#28888=CARTESIAN_POINT('Ctrl Pts',(-0.375277674973257,0.603180457891261,
-0.65));
#28889=CARTESIAN_POINT('Origin',(0.375277674973257,0.,-0.65));
#28890=CARTESIAN_POINT('',(-0.375277674973257,0.,-0.65));
#28891=CARTESIAN_POINT('',(0.375277674973257,0.,-0.65));
#28892=CARTESIAN_POINT('Origin',(-0.375277674973257,0.,-0.65));
#28893=CARTESIAN_POINT('',(-0.750555349946514,0.,-9.19165206894919E-17));
#28894=CARTESIAN_POINT('Origin',(-0.750555349946514,0.,-9.19165206894919E-17));
#28895=CARTESIAN_POINT('',(-0.375277674973257,0.,0.65));
#28896=CARTESIAN_POINT('Origin',(0.,0.,0.));
#28897=CARTESIAN_POINT('',(-0.338975,0.68,4.15124648740974E-17));
#28898=CARTESIAN_POINT('Origin',(0.,0.68,0.));
#28899=CARTESIAN_POINT('',(-0.338975,0.,4.15124648740974E-17));
#28900=CARTESIAN_POINT('',(-0.338975,0.,4.15124648740974E-17));
#28901=CARTESIAN_POINT('Origin',(0.,0.,0.));
#28902=CARTESIAN_POINT('Origin',(-0.375277674973257,0.,0.65));
#28903=CARTESIAN_POINT('',(0.375277674973257,0.,0.65));
#28904=CARTESIAN_POINT('Origin',(0.750555349946514,0.,0.));
#28905=CARTESIAN_POINT('',(0.750555349946514,0.,0.));
#28906=CARTESIAN_POINT('Origin',(0.375277674973257,0.,0.65));
#28907=CARTESIAN_POINT('Origin',(0.,0.68,-1.11022302462516E-16));
#28908=CARTESIAN_POINT('Origin',(0.,0.,-1.11022302462516E-16));
#28909=CARTESIAN_POINT('',(0.,0.,0.));
#28910=CARTESIAN_POINT('',(0.,0.,0.));
#28911=CARTESIAN_POINT('',(0.,0.,0.));
#28912=CARTESIAN_POINT('',(0.,0.,0.));
#28913=CARTESIAN_POINT('',(0.,0.,0.));
#28914=CARTESIAN_POINT('',(0.,0.,0.));
#28915=CARTESIAN_POINT('',(0.,0.,0.));
#28916=CARTESIAN_POINT('',(0.,0.,0.));
#28917=CARTESIAN_POINT('',(0.,0.,0.));
#28918=CARTESIAN_POINT('',(0.,0.,0.));
#28919=CARTESIAN_POINT('',(0.,0.,0.));
#28920=CARTESIAN_POINT('',(0.,0.,0.));
#28921=CARTESIAN_POINT('',(0.,0.,0.));
#28922=CARTESIAN_POINT('',(0.,0.,0.));
#28923=CARTESIAN_POINT('',(-5.5,0.,1.8));
#28924=CARTESIAN_POINT('',(-8.5,3.,1.8));
#28925=CARTESIAN_POINT('',(-11.5,3.67394039744206E-16,1.8));
#28926=CARTESIAN_POINT('',(-8.5,-3.,1.8));
#28927=CARTESIAN_POINT('',(-3.,0.,19.2));
#28928=CARTESIAN_POINT('',(-3.,0.,19.36));
#28929=CARTESIAN_POINT('',(-3.,0.,16.8));
#28930=CARTESIAN_POINT('',(-3.,0.,16.64));
#28931=CARTESIAN_POINT('',(3.,0.,19.2));
#28932=CARTESIAN_POINT('',(3.,0.,19.36));
#28933=CARTESIAN_POINT('',(3.,0.,16.8));
#28934=CARTESIAN_POINT('',(3.,0.,16.64));
#28935=CARTESIAN_POINT('',(-5.2,0.,29.2));
#28936=CARTESIAN_POINT('',(-5.2,0.,29.36));
#28937=CARTESIAN_POINT('',(-5.2,0.,26.8));
#28938=CARTESIAN_POINT('',(-5.2,0.,26.64));
#28939=CARTESIAN_POINT('',(5.2,0.,29.2));
#28940=CARTESIAN_POINT('',(5.2,0.,29.36));
#28941=CARTESIAN_POINT('',(5.2,0.,26.8));
#28942=CARTESIAN_POINT('',(5.2,0.,26.64));
#28943=CARTESIAN_POINT('',(0.,0.,0.));
#28944=CARTESIAN_POINT('',(0.,0.,0.));
#28945=CARTESIAN_POINT('Origin',(-8.5,0.,13.7));
#28946=CARTESIAN_POINT('',(-9.55012781659967,-2.18430157070126E-5,14.8841069671524));
#28947=CARTESIAN_POINT('',(-9.55001141291652,-2.01662567329067E-6,14.9658930328476));
#28948=CARTESIAN_POINT('',(-9.5501,-1.28600160378464E-16,13.7));
#28949=CARTESIAN_POINT('',(-9.29338130674009,-0.687936125025709,15.));
#28950=CARTESIAN_POINT('Ctrl Pts',(-9.55001141291652,-2.01662567329067E-6,
14.9658930328476));
#28951=CARTESIAN_POINT('Ctrl Pts',(-9.55001922277969,-0.0803165835301839,
14.9695440482821));
#28952=CARTESIAN_POINT('Ctrl Pts',(-9.54090778743713,-0.160626033963762,
14.9731950637165));
#28953=CARTESIAN_POINT('Ctrl Pts',(-9.52264958339625,-0.238792272757937,
14.9768460791509));
#28954=CARTESIAN_POINT('Ctrl Pts',(-9.48405310534775,-0.404029856531109,
14.9845640527673));
#28955=CARTESIAN_POINT('Ctrl Pts',(-9.40458264633919,-0.559690113640443,
14.9922820263836));
#28956=CARTESIAN_POINT('Ctrl Pts',(-9.2933813067401,-0.687936125025703,
15.));
#28957=CARTESIAN_POINT('',(-7.70661869325995,-0.687936125025756,15.));
#28958=CARTESIAN_POINT('Origin',(-8.5,0.,15.));
#28959=CARTESIAN_POINT('Ctrl Pts',(-7.70658096099556,-0.687940818620804,
15.));
#28960=CARTESIAN_POINT('Ctrl Pts',(-7.79864161971976,-0.793915406016005,
14.9936166544345));
#28961=CARTESIAN_POINT('Ctrl Pts',(-7.91206836837192,-0.881430565297469,
14.987233308869));
#28962=CARTESIAN_POINT('Ctrl Pts',(-8.03812224866575,-0.943160376009438,
14.9808499633034));
#28963=CARTESIAN_POINT('Ctrl Pts',(-8.1905314379165,-1.01779663775151,14.9731319896871));
#28964=CARTESIAN_POINT('Ctrl Pts',(-8.36139989944402,-1.05473797530154,
14.9654140160707));
#28965=CARTESIAN_POINT('Ctrl Pts',(-8.53102861693969,-1.04972405688955,
14.9576960424544));
#28966=CARTESIAN_POINT('Ctrl Pts',(-8.70065733443535,-1.04471013847756,
14.949978068838));
#28967=CARTESIAN_POINT('Ctrl Pts',(-8.86904630789917,-0.997740964103553,
14.9422600952216));
#28968=CARTESIAN_POINT('Ctrl Pts',(-9.01678065422342,-0.914232359021707,
14.9345421216053));
#28969=CARTESIAN_POINT('Ctrl Pts',(-9.16451500054767,-0.830723753939859,
14.9268241479889));
#28970=CARTESIAN_POINT('Ctrl Pts',(-9.29159471973234,-0.710675718150169,
14.9191061743726));
#28971=CARTESIAN_POINT('Ctrl Pts',(-9.38336846546382,-0.567928885365873,
14.9113882007562));
#28972=CARTESIAN_POINT('Ctrl Pts',(-9.4751422111953,-0.425182052581577,
14.9036702271398));
#28973=CARTESIAN_POINT('Ctrl Pts',(-9.53160998347358,-0.259736422802674,
14.8959522535235));
#28974=CARTESIAN_POINT('Ctrl Pts',(-9.54626123844843,-0.0906670911680779,
14.8882342799071));
#28975=CARTESIAN_POINT('Ctrl Pts',(-9.54887290460746,-0.0605295601021361,
14.8868585089889));
#28976=CARTESIAN_POINT('Ctrl Pts',(-9.55015585058872,-0.0302768858802269,
14.8854827380706));
#28977=CARTESIAN_POINT('Ctrl Pts',(-9.55012781659967,-2.18430157070126E-5,
14.8841069671524));
#28978=CARTESIAN_POINT('Origin',(-8.5,0.,13.7));
#28979=CARTESIAN_POINT('',(-9.55014776911894,-1.85392180561128E-5,14.5841069671524));
#28980=CARTESIAN_POINT('',(-9.55002842899351,-9.63116671427123E-6,14.6658930328476));
#28981=CARTESIAN_POINT('',(-9.5501,-1.28600160378464E-16,13.7));
#28982=CARTESIAN_POINT('Ctrl Pts',(-9.55002842899351,-9.63116671427123E-6,
14.6658930328476));
#28983=CARTESIAN_POINT('Ctrl Pts',(-9.55005326673695,-0.0729826631512053,
14.6692103912693));
#28984=CARTESIAN_POINT('Ctrl Pts',(-9.54254596316782,-0.145950655912037,
14.6725277496911));
#28985=CARTESIAN_POINT('Ctrl Pts',(-9.52745206094249,-0.217314024833131,
14.6758451081128));
#28986=CARTESIAN_POINT('Ctrl Pts',(-9.49233546383911,-0.383343898150939,
14.6835630817291));
#28987=CARTESIAN_POINT('Ctrl Pts',(-9.41615414400742,-0.540688267457234,
14.6912810553455));
#28988=CARTESIAN_POINT('Ctrl Pts',(-9.30769139353042,-0.671206180295421,
14.6989990289619));
#28989=CARTESIAN_POINT('Ctrl Pts',(-9.19922864305341,-0.801724093133606,
14.7067170025782));
#28990=CARTESIAN_POINT('Ctrl Pts',(-9.05848446193109,-0.905415549503684,
14.7144349761946));
#28991=CARTESIAN_POINT('Ctrl Pts',(-8.90168588647599,-0.970325496300035,
14.722152949811));
#28992=CARTESIAN_POINT('Ctrl Pts',(-8.74488731102089,-1.03523544309639,
14.7298709234273));
#28993=CARTESIAN_POINT('Ctrl Pts',(-8.57203434123302,-1.06136388031901,
14.7375888970437));
#28994=CARTESIAN_POINT('Ctrl Pts',(-8.40305598661677,-1.04569832567051,
14.74530687066));
#28995=CARTESIAN_POINT('Ctrl Pts',(-8.23407763200053,-1.03003277102201,
14.7530248442764));
#28996=CARTESIAN_POINT('Ctrl Pts',(-8.06897389255591,-0.972573224502382,
14.7607428178928));
#28997=CARTESIAN_POINT('Ctrl Pts',(-7.92678032355634,-0.879944493087918,
14.7684607915091));
#28998=CARTESIAN_POINT('Ctrl Pts',(-7.78458675455677,-0.787315761673454,
14.7761787651255));
#28999=CARTESIAN_POINT('Ctrl Pts',(-7.66530335600225,-0.659517845364154,
14.7838967387419));
#29000=CARTESIAN_POINT('Ctrl Pts',(-7.5826828692813,-0.511285074047506,
14.7916147123582));
#29001=CARTESIAN_POINT('Ctrl Pts',(-7.50006238256035,-0.363052302730855,
14.7993326859746));
#29002=CARTESIAN_POINT('Ctrl Pts',(-7.45410480767297,-0.194384676406854,
14.8070506595909));
#29003=CARTESIAN_POINT('Ctrl Pts',(-7.45010876983605,-0.0247288141878713,
14.8147686332073));
#29004=CARTESIAN_POINT('Ctrl Pts',(-7.44611273199913,0.144927048031107,
14.8224866068237));
#29005=CARTESIAN_POINT('Ctrl Pts',(-7.48407823121267,0.315571146145067,
14.83020458044));
#29006=CARTESIAN_POINT('Ctrl Pts',(-7.5596281217401,0.467529493626993,14.8379225540564));
#29007=CARTESIAN_POINT('Ctrl Pts',(-7.63517801226754,0.619487841108922,
14.8456405276727));
#29008=CARTESIAN_POINT('Ctrl Pts',(-7.74831229410887,0.752760437958817,
14.8533585012891));
#29009=CARTESIAN_POINT('Ctrl Pts',(-7.88598704248203,0.851980929732758,
14.8610764749055));
#29010=CARTESIAN_POINT('Ctrl Pts',(-8.02366179085519,0.951201421506699,
14.8687944485218));
#29011=CARTESIAN_POINT('Ctrl Pts',(-8.18587700576016,1.01636980820469,14.8765124221382));
#29012=CARTESIAN_POINT('Ctrl Pts',(-8.35393047093769,1.03997418164186,14.8842303957546));
#29013=CARTESIAN_POINT('Ctrl Pts',(-8.52198393611523,1.06357855507904,14.8919483693709));
#29014=CARTESIAN_POINT('Ctrl Pts',(-8.69587565156532,1.0456189152554,14.8996663429873));
#29015=CARTESIAN_POINT('Ctrl Pts',(-8.85555605774434,0.988162433411327,
14.9073843166036));
#29016=CARTESIAN_POINT('Ctrl Pts',(-9.01523646392337,0.930705951567249,
14.91510229022));
#29017=CARTESIAN_POINT('Ctrl Pts',(-9.16070556083133,0.833752627702728,
14.9228202638364));
#29018=CARTESIAN_POINT('Ctrl Pts',(-9.27519284226569,0.708488603778973,
14.9305382374527));
#29019=CARTESIAN_POINT('Ctrl Pts',(-9.38968012370006,0.583224579855222,
14.9382562110691));
#29020=CARTESIAN_POINT('Ctrl Pts',(-9.47318558966083,0.429649855872239,
14.9459741846855));
#29021=CARTESIAN_POINT('Ctrl Pts',(-9.516077074097,0.265455038662242,14.9536921583018));
#29022=CARTESIAN_POINT('Ctrl Pts',(-9.53867858613031,0.178933175738607,
14.9577591164838));
#29023=CARTESIAN_POINT('Ctrl Pts',(-9.55000271331294,0.0894624052226828,
14.9618260746657));
#29024=CARTESIAN_POINT('Ctrl Pts',(-9.55001141291652,-2.01662567329067E-6,
14.9658930328476));
#29025=CARTESIAN_POINT('Ctrl Pts',(-9.55012781659967,-2.18430157070126E-5,
14.8841069671524));
#29026=CARTESIAN_POINT('Ctrl Pts',(-9.54999858197299,0.139451678297384,
14.8777647644543));
#29027=CARTESIAN_POINT('Ctrl Pts',(-9.52200915934138,0.278975536633117,
14.8714225617561));
#29028=CARTESIAN_POINT('Ctrl Pts',(-9.46789751229482,0.407501496024797,
14.865080359058));
#29029=CARTESIAN_POINT('Ctrl Pts',(-9.40204779349493,0.563907718092787,
14.8573623854417));
#29030=CARTESIAN_POINT('Ctrl Pts',(-9.29751361822373,0.704027128738476,
14.8496444118253));
#29031=CARTESIAN_POINT('Ctrl Pts',(-9.16634718282251,0.811704698310384,
14.8419264382089));
#29032=CARTESIAN_POINT('Ctrl Pts',(-9.0351807474213,0.919382267882293,14.8342084645926));
#29033=CARTESIAN_POINT('Ctrl Pts',(-8.87738205189007,0.994617996380422,
14.8264904909762));
#29034=CARTESIAN_POINT('Ctrl Pts',(-8.71114443817192,1.02873762525396,14.8187725173598));
#29035=CARTESIAN_POINT('Ctrl Pts',(-8.54490682445378,1.0628572541275,14.8110545437435));
#29036=CARTESIAN_POINT('Ctrl Pts',(-8.37023029254873,1.05586078337645,14.8033365701271));
#29037=CARTESIAN_POINT('Ctrl Pts',(-8.20725409024193,1.00855486276817,14.7956185965108));
#29038=CARTESIAN_POINT('Ctrl Pts',(-8.04427788793513,0.961248942159876,
14.7879006228944));
#29039=CARTESIAN_POINT('Ctrl Pts',(-7.89300201522659,0.873633571694345,
14.780182649278));
#29040=CARTESIAN_POINT('Ctrl Pts',(-7.77086775905398,0.755810328966214,
14.7724646756617));
#29041=CARTESIAN_POINT('Ctrl Pts',(-7.64873350288136,0.637987086238083,
14.7647467020453));
#29042=CARTESIAN_POINT('Ctrl Pts',(-7.55574086324466,0.489955971247353,
14.7570287284289));
#29043=CARTESIAN_POINT('Ctrl Pts',(-7.50261138405976,0.328784164475392,
14.7493107548126));
#29044=CARTESIAN_POINT('Ctrl Pts',(-7.44948190487485,0.167612357703432,
14.7415927811962));
#29045=CARTESIAN_POINT('Ctrl Pts',(-7.43621558614173,-0.00670014084975726,
14.7338748075799));
#29046=CARTESIAN_POINT('Ctrl Pts',(-7.46434196270175,-0.174056048645625,
14.7261568339635));
#29047=CARTESIAN_POINT('Ctrl Pts',(-7.49246833926176,-0.341411956441492,
14.7184388603471));
#29048=CARTESIAN_POINT('Ctrl Pts',(-7.56198741111491,-0.501811273480041,
14.7107208867308));
#29049=CARTESIAN_POINT('Ctrl Pts',(-7.6648840075379,-0.636760832049021,
14.7030029131144));
#29050=CARTESIAN_POINT('Ctrl Pts',(-7.76778060396089,-0.771710390618001,
14.695284939498));
#29051=CARTESIAN_POINT('Ctrl Pts',(-7.90405472495371,-0.881210190717416,
14.6875669658817));
#29052=CARTESIAN_POINT('Ctrl Pts',(-8.05799470643122,-0.952635501466403,
14.6798489922653));
#29053=CARTESIAN_POINT('Ctrl Pts',(-8.21193468790874,-1.02406081221539,
14.672131018649));
#29054=CARTESIAN_POINT('Ctrl Pts',(-8.38354052987094,-1.05741163361395,
14.6644130450326));
#29055=CARTESIAN_POINT('Ctrl Pts',(-8.55302701300903,-1.04884279758615,
14.6566950714162));
#29056=CARTESIAN_POINT('Ctrl Pts',(-8.72251349614711,-1.04027396155835,
14.6489770977999));
#29057=CARTESIAN_POINT('Ctrl Pts',(-8.88988062046108,-0.989785468104193,
14.6412591241835));
#29058=CARTESIAN_POINT('Ctrl Pts',(-9.03583186778373,-0.903198365607414,
14.6335411505671));
#29059=CARTESIAN_POINT('Ctrl Pts',(-9.18178311510637,-0.816611263110635,
14.6258231769508));
#29060=CARTESIAN_POINT('Ctrl Pts',(-9.30631848543768,-0.693925551571234,
14.6181052033344));
#29061=CARTESIAN_POINT('Ctrl Pts',(-9.39507972860953,-0.549286225569062,
14.6103872297181));
#29062=CARTESIAN_POINT('Ctrl Pts',(-9.48384097178138,-0.404646899566892,
14.6026692561017));
#29063=CARTESIAN_POINT('Ctrl Pts',(-9.53682808779378,-0.238053959101951,
14.5949512824853));
#29064=CARTESIAN_POINT('Ctrl Pts',(-9.54793195066775,-0.0687146631774201,
14.587233308869));
#29065=CARTESIAN_POINT('Ctrl Pts',(-9.54943124186531,-0.0458497450256745,
14.5861911949634));
#29066=CARTESIAN_POINT('Ctrl Pts',(-9.55016693607009,-0.0229347565328515,
14.5851490810579));
#29067=CARTESIAN_POINT('Ctrl Pts',(-9.55014776911894,-1.85392180561128E-5,
14.5841069671524));
#29068=CARTESIAN_POINT('Origin',(-8.5,0.,13.7));
#29069=CARTESIAN_POINT('',(-9.55016480120948,-1.36965928395627E-5,14.2841069671524));
#29070=CARTESIAN_POINT('',(-9.55003832846065,-1.48519270705213E-5,14.3658930328476));
#29071=CARTESIAN_POINT('',(-9.5501,-1.28600160378464E-16,13.7));
#29072=CARTESIAN_POINT('Ctrl Pts',(-9.55003832846065,-1.48519270705213E-5,
14.3658930328476));
#29073=CARTESIAN_POINT('Ctrl Pts',(-9.550073241473,-0.0656465445328537,
14.3688767342566));
#29074=CARTESIAN_POINT('Ctrl Pts',(-9.54400906450974,-0.131271863811158,
14.3718604356656));
#29075=CARTESIAN_POINT('Ctrl Pts',(-9.5317817860297,-0.19572804844434,14.3748441370746));
#29076=CARTESIAN_POINT('Ctrl Pts',(-9.50015334880606,-0.36245757805093,
14.382562110691));
#29077=CARTESIAN_POINT('Ctrl Pts',(-9.42728714065459,-0.521364340736037,
14.3902800843074));
#29078=CARTESIAN_POINT('Ctrl Pts',(-9.3215842386497,-0.654127251941727,
14.3979980579237));
#29079=CARTESIAN_POINT('Ctrl Pts',(-9.21588133664482,-0.786890163147415,
14.4057160315401));
#29080=CARTESIAN_POINT('Ctrl Pts',(-9.07734174078653,-0.893509222873686,
14.4134340051565));
#29081=CARTESIAN_POINT('Ctrl Pts',(-8.92193831218837,-0.961691834029087,
14.4211519787728));
#29082=CARTESIAN_POINT('Ctrl Pts',(-8.7665348835902,-1.02987444518449,14.4288699523892));
#29083=CARTESIAN_POINT('Ctrl Pts',(-8.59426762225216,-1.05962060776902,
14.4365879260055));
#29084=CARTESIAN_POINT('Ctrl Pts',(-8.42499800548463,-1.04750075119252,
14.4443058996219));
#29085=CARTESIAN_POINT('Ctrl Pts',(-8.25572838871711,-1.03538089461602,
14.4520238732383));
#29086=CARTESIAN_POINT('Ctrl Pts',(-8.08945641652011,-0.981395018878487,
14.4597418468546));
#29087=CARTESIAN_POINT('Ctrl Pts',(-7.94535234200829,-0.891767401520943,
14.467459820471));
#29088=CARTESIAN_POINT('Ctrl Pts',(-7.80124826749647,-0.802139784163398,
14.4751777940874));
#29089=CARTESIAN_POINT('Ctrl Pts',(-7.67931209066984,-0.676870425185841,
14.4828957677037));
#29090=CARTESIAN_POINT('Ctrl Pts',(-7.59360238882539,-0.530402199643331,
14.4906137413201));
#29091=CARTESIAN_POINT('Ctrl Pts',(-7.50789268698095,-0.383933974100822,
14.4983317149364));
#29092=CARTESIAN_POINT('Ctrl Pts',(-7.4584094601187,-0.216266881993361,
14.5060496885528));
#29093=CARTESIAN_POINT('Ctrl Pts',(-7.4508578548822,-0.0467320261582989,
14.5137676621692));
#29094=CARTESIAN_POINT('Ctrl Pts',(-7.44330624964569,0.122802829676763,
14.5214856357855));
#29095=CARTESIAN_POINT('Ctrl Pts',(-7.47768626603494,0.294205449239426,
14.5292036094019));
#29096=CARTESIAN_POINT('Ctrl Pts',(-7.55003407534174,0.447714043693381,
14.5369215830183));
#29097=CARTESIAN_POINT('Ctrl Pts',(-7.62238188464855,0.601222638147337,
14.5446395566346));
#29098=CARTESIAN_POINT('Ctrl Pts',(-7.73269748687292,0.736837207492585,
14.552357530251));
#29099=CARTESIAN_POINT('Ctrl Pts',(-7.86826209370633,0.838922130279325,
14.5600755038673));
#29100=CARTESIAN_POINT('Ctrl Pts',(-8.00382670053974,0.941007053066066,
14.5677934774837));
#29101=CARTESIAN_POINT('Ctrl Pts',(-8.16464031198218,1.0095623292943,14.5755114511001));
#29102=CARTESIAN_POINT('Ctrl Pts',(-8.33216199418164,1.03668390879925,14.5832294247164));
#29103=CARTESIAN_POINT('Ctrl Pts',(-8.4996836763811,1.06380548830419,14.5909473983328));
#29104=CARTESIAN_POINT('Ctrl Pts',(-8.67391342933756,1.04949337108586,14.5986653719492));
#29105=CARTESIAN_POINT('Ctrl Pts',(-8.83476351117266,0.995397666487676,
14.6063833455655));
#29106=CARTESIAN_POINT('Ctrl Pts',(-8.99561359300775,0.941301961889491,
14.6141013191819));
#29107=CARTESIAN_POINT('Ctrl Pts',(-9.14308400372149,0.847422669911453,
14.6218192927982));
#29108=CARTESIAN_POINT('Ctrl Pts',(-9.26017220780516,0.724583561457418,
14.6295372664146));
#29109=CARTESIAN_POINT('Ctrl Pts',(-9.37726041188882,0.601744453003383,
14.637255240031));
#29110=CARTESIAN_POINT('Ctrl Pts',(-9.46396640934243,0.44994552807335,14.6449732136473));
#29111=CARTESIAN_POINT('Ctrl Pts',(-9.51029347088169,0.286688376943674,
14.6526911872637));
#29112=CARTESIAN_POINT('Ctrl Pts',(-9.53670812077122,0.193602816457645,
14.6570918024583));
#29113=CARTESIAN_POINT('Ctrl Pts',(-9.54999548068424,0.0967921588502287,
14.661492417653));
#29114=CARTESIAN_POINT('Ctrl Pts',(-9.55002842899351,-9.63116671427123E-6,
14.6658930328476));
#29115=CARTESIAN_POINT('Ctrl Pts',(-9.55014776911894,-1.85392180561128E-5,
14.5841069671524));
#29116=CARTESIAN_POINT('Ctrl Pts',(-9.55002498419467,0.146784464834437,
14.5774311074415));
#29117=CARTESIAN_POINT('Ctrl Pts',(-9.51892436163577,0.293637897031557,
14.5707552477307));
#29118=CARTESIAN_POINT('Ctrl Pts',(-9.4591424759889,0.427701752301033,14.5640793880199));
#29119=CARTESIAN_POINT('Ctrl Pts',(-9.39002852870054,0.582693220470828,
14.5563614144035));
#29120=CARTESIAN_POINT('Ctrl Pts',(-9.28258002438829,0.720590505426293,
14.5486434407872));
#29121=CARTESIAN_POINT('Ctrl Pts',(-9.14918519058914,0.825494801005002,
14.5409254671708));
#29122=CARTESIAN_POINT('Ctrl Pts',(-9.01579035679,0.930399096583712,14.5332074935544));
#29123=CARTESIAN_POINT('Ctrl Pts',(-8.85644919350396,1.00231040278566,14.5254895199381));
#29124=CARTESIAN_POINT('Ctrl Pts',(-8.68953286931277,1.03293773753167,14.5177715463217));
#29125=CARTESIAN_POINT('Ctrl Pts',(-8.52261654512158,1.06356507227767,14.5100535727053));
#29126=CARTESIAN_POINT('Ctrl Pts',(-8.34812506002524,1.05290843556774,14.502335599089));
#29127=CARTESIAN_POINT('Ctrl Pts',(-8.18617633222389,1.00219647959389,14.4946176254726));
#29128=CARTESIAN_POINT('Ctrl Pts',(-8.02422760442253,0.951484523620035,
14.4868996518563));
#29129=CARTESIAN_POINT('Ctrl Pts',(-7.87482163391617,0.860717248382274,
14.4791816782399));
#29130=CARTESIAN_POINT('Ctrl Pts',(-7.75518411565231,0.740359626526339,
14.4714637046235));
#29131=CARTESIAN_POINT('Ctrl Pts',(-7.63554659738845,0.620002004670402,
14.4637457310072));
#29132=CARTESIAN_POINT('Ctrl Pts',(-7.54567753136709,0.470054036196291,
14.4560277573908));
#29133=CARTESIAN_POINT('Ctrl Pts',(-7.49593833160183,0.307803905466374,
14.4483097837744));
#29134=CARTESIAN_POINT('Ctrl Pts',(-7.44619913183657,0.145553774736457,
14.4405918101581));
#29135=CARTESIAN_POINT('Ctrl Pts',(-7.4365897983274,-0.0289985182492672,
14.4328738365417));
#29136=CARTESIAN_POINT('Ctrl Pts',(-7.46821823490919,-0.195728044472262,
14.4251558629254));
#29137=CARTESIAN_POINT('Ctrl Pts',(-7.49984667149097,-0.362457570695256,
14.417437889309));
#29138=CARTESIAN_POINT('Ctrl Pts',(-7.5727128781637,-0.521364330155521,
14.4097199156926));
#29139=CARTESIAN_POINT('Ctrl Pts',(-7.67841577802345,-0.654127238666931,
14.4020019420763));
#29140=CARTESIAN_POINT('Ctrl Pts',(-7.78411867788321,-0.786890147178342,
14.3942839684599));
#29141=CARTESIAN_POINT('Ctrl Pts',(-7.92265827092999,-0.893509204740896,
14.3865659948435));
#29142=CARTESIAN_POINT('Ctrl Pts',(-8.07806169637442,-0.961691814512604,
14.3788480212272));
#29143=CARTESIAN_POINT('Ctrl Pts',(-8.23346512181885,-1.02987442428431,
14.3711300476108));
#29144=CARTESIAN_POINT('Ctrl Pts',(-8.40573237966092,-1.05962058626517,
14.3634120739945));
#29145=CARTESIAN_POINT('Ctrl Pts',(-8.5750019929933,-1.04750072993463,14.3556941003781));
#29146=CARTESIAN_POINT('Ctrl Pts',(-8.74427160632568,-1.03538087360409,
14.3479761267617));
#29147=CARTESIAN_POINT('Ctrl Pts',(-8.91054357514837,-0.981394998962145,
14.3402581531454));
#29148=CARTESIAN_POINT('Ctrl Pts',(-9.05464764673576,-0.89176738342349,
14.332540179529));
#29149=CARTESIAN_POINT('Ctrl Pts',(-9.19875171832314,-0.802139767884835,
14.3248222059126));
#29150=CARTESIAN_POINT('Ctrl Pts',(-9.32068789267521,-0.676870411449469,
14.3171042322963));
#29151=CARTESIAN_POINT('Ctrl Pts',(-9.40639759278026,-0.530402188879377,
14.3093862586799));
#29152=CARTESIAN_POINT('Ctrl Pts',(-9.49210729288531,-0.383933966309286,
14.3016682850636));
#29153=CARTESIAN_POINT('Ctrl Pts',(-9.54159051874335,-0.216266877604468,
14.2939503114472));
#29154=CARTESIAN_POINT('Ctrl Pts',(-9.5491421238266,-0.0467320252099184,
14.2862323378308));
#29155=CARTESIAN_POINT('Ctrl Pts',(-9.54983530923238,-0.0311698918414938,
14.285523880938));
#29156=CARTESIAN_POINT('Ctrl Pts',(-9.55017517975655,-0.0155920207387595,
14.2848154240452));
#29157=CARTESIAN_POINT('Ctrl Pts',(-9.55016480120948,-1.36965928395627E-5,
14.2841069671524));
#29158=CARTESIAN_POINT('Origin',(-8.5,0.,13.7));
#29159=CARTESIAN_POINT('',(-9.55017700723911,-7.61513114500012E-6,13.9841069671524));
#29160=CARTESIAN_POINT('',(-9.5500522825869,-1.91003407042144E-5,14.0658930328476));
#29161=CARTESIAN_POINT('',(-9.5501,-1.28600160378464E-16,13.7));
#29162=CARTESIAN_POINT('',(-7.70661869325991,-0.687936125025711,13.8));
#29163=CARTESIAN_POINT('Ctrl Pts',(-9.55017700723911,-7.61513114500012E-6,
13.9841069671524));
#29164=CARTESIAN_POINT('Ctrl Pts',(-9.55011125498444,0.161456600375193,
13.9767637934161));
#29165=CARTESIAN_POINT('Ctrl Pts',(-9.51225289750323,0.322950533171347,
13.9694206196799));
#29166=CARTESIAN_POINT('Ctrl Pts',(-9.44037185879917,0.467529483605666,
13.9620774459436));
#29167=CARTESIAN_POINT('Ctrl Pts',(-9.36482196986006,0.61948782818686,13.9543594723273));
#29168=CARTESIAN_POINT('Ctrl Pts',(-9.25168769073042,0.752760423312007,
13.9466414987109));
#29169=CARTESIAN_POINT('Ctrl Pts',(-9.11401294444701,0.851980912188383,
13.9389235250945));
#29170=CARTESIAN_POINT('Ctrl Pts',(-8.97633819816361,0.95120140106476,13.9312055514782));
#29171=CARTESIAN_POINT('Ctrl Pts',(-8.81412298472643,1.01636978369236,13.9234875778618));
#29172=CARTESIAN_POINT('Ctrl Pts',(-8.64606952266772,1.03997415669788,13.9157696042454));
#29173=CARTESIAN_POINT('Ctrl Pts',(-8.478016060609,1.0635785297034,13.9080516306291));
#29174=CARTESIAN_POINT('Ctrl Pts',(-8.30412434992875,1.04561889308684,13.9003336570127));
#29175=CARTESIAN_POINT('Ctrl Pts',(-8.14444394193064,0.988162407251559,
13.8926156833964));
#29176=CARTESIAN_POINT('Ctrl Pts',(-7.98476353393253,0.930705921416282,
13.88489770978));
#29177=CARTESIAN_POINT('Ctrl Pts',(-7.83929442861656,0.833752586362294,
13.8771797361636));
#29178=CARTESIAN_POINT('Ctrl Pts',(-7.72480714475875,0.708488560736079,
13.8694617625473));
#29179=CARTESIAN_POINT('Ctrl Pts',(-7.61031986090093,0.583224535109864,
13.8617437889309));
#29180=CARTESIAN_POINT('Ctrl Pts',(-7.52681439850127,0.429649818911422,
13.8540258153145));
#29181=CARTESIAN_POINT('Ctrl Pts',(-7.48392288713058,0.265454980301966,
13.8463078416982));
#29182=CARTESIAN_POINT('Ctrl Pts',(-7.44103137575989,0.101260141692509,
13.8385898680818));
#29183=CARTESIAN_POINT('Ctrl Pts',(-7.43875381541816,-0.0735548193279625,
13.8308718944655));
#29184=CARTESIAN_POINT('Ctrl Pts',(-7.47735030989339,-0.238792383161204,
13.8231539208491));
#29185=CARTESIAN_POINT('Ctrl Pts',(-7.51594680436863,-0.404029946994446,
13.8154359472327));
#29186=CARTESIAN_POINT('Ctrl Pts',(-7.59541735366082,-0.559690113640457,
13.8077179736164));
#29187=CARTESIAN_POINT('Ctrl Pts',(-7.70661869325992,-0.687936125025717,
13.8));
#29188=CARTESIAN_POINT('',(-9.29341905289386,-0.68794083902029,13.8));
#29189=CARTESIAN_POINT('Origin',(-8.5,0.,13.8));
#29190=CARTESIAN_POINT('Ctrl Pts',(-9.29341905289386,-0.68794083902029,
13.8));
#29191=CARTESIAN_POINT('Ctrl Pts',(-9.20135839317727,-0.793915425263775,
13.8063833455655));
#29192=CARTESIAN_POINT('Ctrl Pts',(-9.08793164264836,-0.881430588389637,
13.812766691131));
#29193=CARTESIAN_POINT('Ctrl Pts',(-8.96187776001814,-0.943160400251609,
13.8191500366965));
#29194=CARTESIAN_POINT('Ctrl Pts',(-8.80946856794249,-1.01779666338413,
13.8268680103129));
#29195=CARTESIAN_POINT('Ctrl Pts',(-8.63860010291811,-1.05473799838573,
13.8345859839293));
#29196=CARTESIAN_POINT('Ctrl Pts',(-8.4689713820678,-1.04972407874521,13.8423039575456));
#29197=CARTESIAN_POINT('Ctrl Pts',(-8.29934266121749,-1.04471015910468,
13.850021931162));
#29198=CARTESIAN_POINT('Ctrl Pts',(-8.13095368454124,-0.997740984822029,
13.8577399047784));
#29199=CARTESIAN_POINT('Ctrl Pts',(-7.98321933527585,-0.914232378227999,
13.8654578783947));
#29200=CARTESIAN_POINT('Ctrl Pts',(-7.83548498601045,-0.830723771633969,
13.8731758520111));
#29201=CARTESIAN_POINT('Ctrl Pts',(-7.70840526415591,-0.710675732728563,
13.8808938256275));
#29202=CARTESIAN_POINT('Ctrl Pts',(-7.61663151655039,-0.567928896847351,
13.8886117992438));
#29203=CARTESIAN_POINT('Ctrl Pts',(-7.52485776894487,-0.425182060966139,
13.8963297728602));
#29204=CARTESIAN_POINT('Ctrl Pts',(-7.46838999558837,-0.259736428109122,
13.9040477464765));
#29205=CARTESIAN_POINT('Ctrl Pts',(-7.45373874033249,-0.0906670931082204,
13.9117657200929));
#29206=CARTESIAN_POINT('Ctrl Pts',(-7.43908748507661,0.0784022418926819,
13.9194836937093));
#29207=CARTESIAN_POINT('Ctrl Pts',(-7.46625274792135,0.251095279037468,
13.9272016673256));
#29208=CARTESIAN_POINT('Ctrl Pts',(-7.53210246805017,0.407501504320363,
13.934919640942));
#29209=CARTESIAN_POINT('Ctrl Pts',(-7.59795218817899,0.563907729603256,
13.9426376145584));
#29210=CARTESIAN_POINT('Ctrl Pts',(-7.7024863655919,0.704027143024259,13.9503555881747));
#29211=CARTESIAN_POINT('Ctrl Pts',(-7.83365280365984,0.811704714764279,
13.9580735617911));
#29212=CARTESIAN_POINT('Ctrl Pts',(-7.96481924172778,0.919382286504301,
13.9657915354074));
#29213=CARTESIAN_POINT('Ctrl Pts',(-8.12261794045076,0.99461801656334,13.9735095090238));
#29214=CARTESIAN_POINT('Ctrl Pts',(-8.28885555754004,1.02873764613831,13.9812274826402));
#29215=CARTESIAN_POINT('Ctrl Pts',(-8.45509317462931,1.06285727571327,13.9889454562565));
#29216=CARTESIAN_POINT('Ctrl Pts',(-8.62976971008488,1.05586080480417,13.9966634298729));
#29217=CARTESIAN_POINT('Ctrl Pts',(-8.79274591570048,1.00855488323173,14.0043814034893));
#29218=CARTESIAN_POINT('Ctrl Pts',(-8.95572212131607,0.961248961659288,
14.0120993771056));
#29219=CARTESIAN_POINT('Ctrl Pts',(-9.10699799709169,0.873633589423514,
14.019817350722));
#29220=CARTESIAN_POINT('Ctrl Pts',(-9.22913225574218,0.755810344306336,
14.0275353243383));
#29221=CARTESIAN_POINT('Ctrl Pts',(-9.35126651439268,0.637987099189158,
14.0352532979547));
#29222=CARTESIAN_POINT('Ctrl Pts',(-9.44425915591805,0.489955981190576,
14.0429712715711));
#29223=CARTESIAN_POINT('Ctrl Pts',(-9.49738863618153,0.328784171146844,
14.0506892451874));
#29224=CARTESIAN_POINT('Ctrl Pts',(-9.53227557138735,0.222952334168298,
14.0557571744075));
#29225=CARTESIAN_POINT('Ctrl Pts',(-9.54997447121724,0.111454547160044,
14.0608251036276));
#29226=CARTESIAN_POINT('Ctrl Pts',(-9.5500522825869,-1.91003407042144E-5,
14.0658930328476));
#29227=CARTESIAN_POINT('Origin',(-8.5,0.,13.1374873996035));
#29228=CARTESIAN_POINT('',(-9.71736702302461,-1.11660450847761E-5,14.7625126003965));
#29229=CARTESIAN_POINT('',(-9.71748224961362,-2.53240448353063E-5,14.7874873996035));
#29230=CARTESIAN_POINT('',(-9.71745,1.55202226700376E-15,13.1374873996035));
#29231=CARTESIAN_POINT('',(-8.18521110449559,1.17604951161383,15.));
#29232=CARTESIAN_POINT('Ctrl Pts',(-9.71748224961362,-2.53240448353162E-5,
14.7874873996035));
#29233=CARTESIAN_POINT('Ctrl Pts',(-9.71751475126106,-0.035101985253679,
14.7888631705217));
#29234=CARTESIAN_POINT('Ctrl Pts',(-9.70768312250827,-0.266937983084884,
14.7979569150563));
#29235=CARTESIAN_POINT('Ctrl Pts',(-9.56507970256121,-0.68475352051211,
14.8147686332073));
#29236=CARTESIAN_POINT('Ctrl Pts',(-9.12308407132213,-1.10229227255141,
14.8379225540564));
#29237=CARTESIAN_POINT('Ctrl Pts',(-8.53741083331568,-1.26565563225515,
14.8610764749055));
#29238=CARTESIAN_POINT('Ctrl Pts',(-7.94311369450983,-1.13717006497505,
14.8842303957546));
#29239=CARTESIAN_POINT('Ctrl Pts',(-7.47722284672394,-0.74647126776861,
14.9073843166036));
#29240=CARTESIAN_POINT('Ctrl Pts',(-7.24718575990748,-0.183633090657203,
14.9305382374527));
#29241=CARTESIAN_POINT('Ctrl Pts',(-7.3060080642777,0.421519192034503,14.9536921583018));
#29242=CARTESIAN_POINT('Ctrl Pts',(-7.64021279447249,0.92951767940246,14.9768460791509));
#29243=CARTESIAN_POINT('Ctrl Pts',(-7.99510874416173,1.12516550422186,14.9922820263836));
#29244=CARTESIAN_POINT('Ctrl Pts',(-8.18521110449559,1.17604951161383,15.));
#29245=CARTESIAN_POINT('',(-8.81478889550434,1.17604951161384,15.));
#29246=CARTESIAN_POINT('Origin',(-8.5,0.,15.));
#29247=CARTESIAN_POINT('Ctrl Pts',(-9.71736702302461,-1.11660450847831E-5,
14.7625126003965));
#29248=CARTESIAN_POINT('Ctrl Pts',(-9.71739581905428,-0.0846136018031169,
14.7658299588182));
#29249=CARTESIAN_POINT('Ctrl Pts',(-9.68844255967355,-0.366027720925746,
14.7768652908563));
#29250=CARTESIAN_POINT('Ctrl Pts',(-9.47383574401748,-0.809275148678942,
14.7956185965108));
#29251=CARTESIAN_POINT('Ctrl Pts',(-8.98431378427829,-1.16992412560805,
14.8187725173598));
#29252=CARTESIAN_POINT('Ctrl Pts',(-8.38311433260251,-1.26080137319404,
14.8419264382089));
#29253=CARTESIAN_POINT('Ctrl Pts',(-7.80886745824715,-1.06095147820218,
14.865080359058));
#29254=CARTESIAN_POINT('Ctrl Pts',(-7.39398818892938,-0.616457887465797,
14.8882342799071));
#29255=CARTESIAN_POINT('Ctrl Pts',(-7.23414327069309,-0.0298154676920097,
14.9113882007562));
#29256=CARTESIAN_POINT('Ctrl Pts',(-7.36619097191447,0.563701313325544,
14.9345421216053));
#29257=CARTESIAN_POINT('Ctrl Pts',(-7.75968301484676,1.02723637580027,14.9576960424544));
#29258=CARTESIAN_POINT('Ctrl Pts',(-8.29136193563724,1.24083321706785,14.9795153352526));
#29259=CARTESIAN_POINT('Ctrl Pts',(-8.6575692829609,1.2180150268885,14.9936166544345));
#29260=CARTESIAN_POINT('Ctrl Pts',(-8.81482207543406,1.17607856395779,15.));
#29261=CARTESIAN_POINT('Origin',(-8.5,0.,13.1374873996035));
#29262=CARTESIAN_POINT('',(-9.717378500128,-1.72188158990005E-5,14.4625126003965));
#29263=CARTESIAN_POINT('',(-9.71750538188158,-2.1493734860395E-5,14.4874873996035));
#29264=CARTESIAN_POINT('',(-9.71745,1.55202226700376E-15,13.1374873996035));
#29265=CARTESIAN_POINT('Ctrl Pts',(-9.71750538188158,-2.14937348604928E-5,
14.4874873996035));
#29266=CARTESIAN_POINT('Ctrl Pts',(-9.71752760338875,-0.0265897717749626,
14.488529513509));
#29267=CARTESIAN_POINT('Ctrl Pts',(-9.71035773696392,-0.249912730625655,
14.4972896010309));
#29268=CARTESIAN_POINT('Ctrl Pts',(-9.57920010161505,-0.662275919671228,
14.5137676621692));
#29269=CARTESIAN_POINT('Ctrl Pts',(-9.14605396331434,-1.08898876467735,
14.5369215830183));
#29270=CARTESIAN_POINT('Ctrl Pts',(-8.56393481610157,-1.2645926586563,14.5600755038673));
#29271=CARTESIAN_POINT('Ctrl Pts',(-7.96707299637902,-1.14859525599462,
14.5832294247164));
#29272=CARTESIAN_POINT('Ctrl Pts',(-7.49309834081465,-0.767744294283258,
14.6063833455655));
#29273=CARTESIAN_POINT('Ctrl Pts',(-7.25130424303077,-0.209859858909738,
14.6295372664146));
#29274=CARTESIAN_POINT('Ctrl Pts',(-7.29744579071662,0.396415975859085,
14.6526911872637));
#29275=CARTESIAN_POINT('Ctrl Pts',(-7.62088324179469,0.911282600786611,
14.6758451081128));
#29276=CARTESIAN_POINT('Ctrl Pts',(-8.14703544985776,1.21601738634968,14.6989990289619));
#29277=CARTESIAN_POINT('Ctrl Pts',(-8.75457742805358,1.2403517925468,14.722152949811));
#29278=CARTESIAN_POINT('Ctrl Pts',(-9.3034166487216,0.978674606583422,14.74530687066));
#29279=CARTESIAN_POINT('Ctrl Pts',(-9.6453933088254,0.520283195889185,14.7670850205909));
#29280=CARTESIAN_POINT('Ctrl Pts',(-9.71733241941055,0.1616755030408,14.7811451969054));
#29281=CARTESIAN_POINT('Ctrl Pts',(-9.71748224961362,-2.53240448353162E-5,
14.7874873996035));
#29282=CARTESIAN_POINT('Ctrl Pts',(-9.717378500128,-1.72188158990352E-5,
14.4625126003965));
#29283=CARTESIAN_POINT('Ctrl Pts',(-9.71741897707961,-0.0761083569579073,
14.4654963018055));
#29284=CARTESIAN_POINT('Ctrl Pts',(-9.69220224865988,-0.348998786067701,
14.4761979768309));
#29285=CARTESIAN_POINT('Ctrl Pts',(-9.49058638632123,-0.788683034815797,
14.4946176254726));
#29286=CARTESIAN_POINT('Ctrl Pts',(-9.00873218868954,-1.159514501144,14.5177715463217));
#29287=CARTESIAN_POINT('Ctrl Pts',(-8.40956988800579,-1.26297454963044,
14.5409254671708));
#29288=CARTESIAN_POINT('Ctrl Pts',(-7.8312597864405,-1.07520641969046,14.5640793880199));
#29289=CARTESIAN_POINT('Ctrl Pts',(-7.40715389611314,-0.639507397443362,
14.587233308869));
#29290=CARTESIAN_POINT('Ctrl Pts',(-7.23504641717748,-0.0563449330507459,
14.6103872297181));
#29291=CARTESIAN_POINT('Ctrl Pts',(-7.35462346018219,0.539810059387775,
14.6335411505671));
#29292=CARTESIAN_POINT('Ctrl Pts',(-7.73831186108132,1.01149073013163,14.6566950714162));
#29293=CARTESIAN_POINT('Ctrl Pts',(-8.29763725271243,1.24993265293153,14.6798489922653));
#29294=CARTESIAN_POINT('Ctrl Pts',(-8.9036252902427,1.20015371633275,14.7030029131144));
#29295=CARTESIAN_POINT('Ctrl Pts',(-9.4165417311248,0.873632402118881,14.7261568339635));
#29296=CARTESIAN_POINT('Ctrl Pts',(-9.6749061703283,0.421305628158093,14.7459933963909));
#29297=CARTESIAN_POINT('Ctrl Pts',(-9.71732882388252,0.112217516229114,
14.7581119852019));
#29298=CARTESIAN_POINT('Ctrl Pts',(-9.71736702302461,-1.11660450847831E-5,
14.7625126003965));
#29299=CARTESIAN_POINT('Origin',(-8.5,0.,13.1374873996035));
#29300=CARTESIAN_POINT('',(-9.7173946780644,-2.21442813102546E-5,14.1625126003965));
#29301=CARTESIAN_POINT('',(-9.71752512830443,-1.58793609722743E-5,14.1874873996035));
#29302=CARTESIAN_POINT('',(-9.71745,1.55202226700376E-15,13.1374873996035));
#29303=CARTESIAN_POINT('Ctrl Pts',(-9.71752512830443,-1.58793609723457E-5,
14.1874873996035));
#29304=CARTESIAN_POINT('Ctrl Pts',(-9.71753716083669,-0.0180768552027482,
14.1881958564963));
#29305=CARTESIAN_POINT('Ctrl Pts',(-9.71285049282718,-0.232888982065844,
14.1966222870055));
#29306=CARTESIAN_POINT('Ctrl Pts',(-9.59284608170875,-0.639507384465213,
14.212766691131));
#29307=CARTESIAN_POINT('Ctrl Pts',(-9.16874019998817,-1.07520639787033,
14.2359206119801));
#29308=CARTESIAN_POINT('Ctrl Pts',(-8.59043011015904,-1.26297452399975,
14.2590745328292));
#29309=CARTESIAN_POINT('Ctrl Pts',(-7.99126782163464,-1.15951447761293,
14.2822284536783));
#29310=CARTESIAN_POINT('Ctrl Pts',(-7.50941363378165,-0.788683018810342,
14.3053823745274));
#29311=CARTESIAN_POINT('Ctrl Pts',(-7.25597787533851,-0.235989843955851,
14.3285362953765));
#29312=CARTESIAN_POINT('Ctrl Pts',(-7.28940007250277,0.371120019187095,
14.3516902162256));
#29313=CARTESIAN_POINT('Ctrl Pts',(-7.60197343054782,0.892653647085789,
14.3748441370747));
#29314=CARTESIAN_POINT('Ctrl Pts',(-8.12162193676524,1.20835106420286,14.3979980579237));
#29315=CARTESIAN_POINT('Ctrl Pts',(-8.72852030415086,1.24541588382723,14.4211519787728));
#29316=CARTESIAN_POINT('Ctrl Pts',(-9.28272437778932,0.995301362156251,
14.4443058996219));
#29317=CARTESIAN_POINT('Ctrl Pts',(-9.63962047130265,0.537267975635789,
14.4664177065655));
#29318=CARTESIAN_POINT('Ctrl Pts',(-9.71736302924274,0.170176884784988,
14.4808115398927));
#29319=CARTESIAN_POINT('Ctrl Pts',(-9.71750538188158,-2.14937348604928E-5,
14.4874873996035));
#29320=CARTESIAN_POINT('Ctrl Pts',(-9.7173946780644,-2.21442813102893E-5,
14.1625126003965));
#29321=CARTESIAN_POINT('Ctrl Pts',(-9.71744185026584,-0.0676016943959369,
14.1651626447928));
#29322=CARTESIAN_POINT('Ctrl Pts',(-9.69577189929841,-0.331969587358445,
14.1755306628055));
#29323=CARTESIAN_POINT('Ctrl Pts',(-9.50690167961977,-0.767744309864743,
14.1936166544345));
#29324=CARTESIAN_POINT('Ctrl Pts',(-9.03292701443594,-1.14859527930365,
14.2167705752836));
#29325=CARTESIAN_POINT('Ctrl Pts',(-8.43606518260107,-1.26459268432005,
14.2399244961327));
#29326=CARTESIAN_POINT('Ctrl Pts',(-7.85394602357466,-1.08898878677709,
14.2630784169817));
#29327=CARTESIAN_POINT('Ctrl Pts',(-7.4207998764838,-0.662275933111461,
14.2862323378308));
#29328=CARTESIAN_POINT('Ctrl Pts',(-7.23650552633111,-0.0828494609134307,
14.3093862586799));
#29329=CARTESIAN_POINT('Ctrl Pts',(-7.3435592434188,0.515681194822054,14.332540179529));
#29330=CARTESIAN_POINT('Ctrl Pts',(-7.71727560632613,0.995301382354801,
14.3556941003781));
#29331=CARTESIAN_POINT('Ctrl Pts',(-8.27147969121155,1.24541590910158,14.3788480212272));
#29332=CARTESIAN_POINT('Ctrl Pts',(-8.87837807091352,1.20835108872504,14.4020019420763));
#29333=CARTESIAN_POINT('Ctrl Pts',(-9.39802658767663,0.892653665201231,
14.4251558629254));
#29334=CARTESIAN_POINT('Ctrl Pts',(-9.67032057157381,0.438326814809805,
14.4453260823654));
#29335=CARTESIAN_POINT('Ctrl Pts',(-9.71731427489874,0.120717436282016,
14.4577783281892));
#29336=CARTESIAN_POINT('Ctrl Pts',(-9.717378500128,-1.72188158990352E-5,
14.4625126003965));
#29337=CARTESIAN_POINT('Origin',(-8.5,0.,13.1374873996035));
#29338=CARTESIAN_POINT('',(-9.7174151537438,-2.95534814070963E-5,13.8625126003965));
#29339=CARTESIAN_POINT('',(-9.71753927955743,-8.82872242793887E-6,13.8874873996035));
#29340=CARTESIAN_POINT('',(-9.71745,1.55202226700376E-15,13.1374873996035));
#29341=CARTESIAN_POINT('',(-8.81478889550441,1.17604951161383,13.8));
#29342=CARTESIAN_POINT('Ctrl Pts',(-8.81478889550439,1.17604951161383,13.8));
#29343=CARTESIAN_POINT('Ctrl Pts',(-9.00489125583826,1.12516550422186,13.8077179736164));
#29344=CARTESIAN_POINT('Ctrl Pts',(-9.35978714971093,0.929517388355175,
13.8231539208491));
#29345=CARTESIAN_POINT('Ctrl Pts',(-9.6605571008421,0.472340818518349,13.8439914543146));
#29346=CARTESIAN_POINT('Ctrl Pts',(-9.71730301126828,0.137708208335554,
13.8571110141637));
#29347=CARTESIAN_POINT('Ctrl Pts',(-9.7174151537438,-2.95534814072282E-5,
13.8625126003965));
#29348=CARTESIAN_POINT('',(-8.18517792464733,1.17607853534586,13.8));
#29349=CARTESIAN_POINT('Origin',(-8.5,0.,13.8));
#29350=CARTESIAN_POINT('Ctrl Pts',(-8.18517792464733,1.17607853534586,13.8));
#29351=CARTESIAN_POINT('Ctrl Pts',(-8.34243071691597,1.21801500002725,13.8063833455655));
#29352=CARTESIAN_POINT('Ctrl Pts',(-8.7086380547407,1.24083318474607,13.8204846647474));
#29353=CARTESIAN_POINT('Ctrl Pts',(-9.24031697072028,1.02723635681965,13.8423039575456));
#29354=CARTESIAN_POINT('Ctrl Pts',(-9.62743942353789,0.571204689714611,
13.8650830785146));
#29355=CARTESIAN_POINT('Ctrl Pts',(-9.71746304864376,0.187187256572491,
13.8801442258672));
#29356=CARTESIAN_POINT('Ctrl Pts',(-9.71753927955742,-8.82872242803645E-6,
13.8874873996035));
#29357=CARTESIAN_POINT('Origin',(-8.5,0.,13.1374873996035));
#29358=CARTESIAN_POINT('Ctrl Pts',(-9.71753927955742,-8.82872242803645E-6,
13.8874873996035));
#29359=CARTESIAN_POINT('Ctrl Pts',(-9.71754317042782,-0.00956342634534076,
13.8878621994836));
#29360=CARTESIAN_POINT('Ctrl Pts',(-9.71516252585584,-0.215866768863219,
13.8959549729801));
#29361=CARTESIAN_POINT('Ctrl Pts',(-9.60601178848326,-0.616457875299982,
13.9117657200929));
#29362=CARTESIAN_POINT('Ctrl Pts',(-9.19113252777601,-1.06095145651566,
13.934919640942));
#29363=CARTESIAN_POINT('Ctrl Pts',(-8.61688566499978,-1.26080134768798,
13.9580735617911));
#29364=CARTESIAN_POINT('Ctrl Pts',(-8.0156862255606,-1.16992410182742,13.9812274826402));
#29365=CARTESIAN_POINT('Ctrl Pts',(-7.52616427574063,-0.809275132274592,
14.0043814034892));
#29366=CARTESIAN_POINT('Ctrl Pts',(-7.26119823647443,-0.262016113511643,
14.0275353243383));
#29367=CARTESIAN_POINT('Ctrl Pts',(-7.28188639587083,0.345660960504597,
14.0506892451874));
#29368=CARTESIAN_POINT('Ctrl Pts',(-7.5834582874758,0.873632384391611,14.0738431660365));
#29369=CARTESIAN_POINT('Ctrl Pts',(-8.09637471794825,1.2001536919759,14.0969970868856));
#29370=CARTESIAN_POINT('Ctrl Pts',(-8.7023627431809,1.24993262756601,14.1201510077347));
#29371=CARTESIAN_POINT('Ctrl Pts',(-9.26168812346101,1.01149070960429,14.1433049285838));
#29372=CARTESIAN_POINT('Ctrl Pts',(-9.63363653142959,0.554242395239179,
14.16575039254));
#29373=CARTESIAN_POINT('Ctrl Pts',(-9.71740607767908,0.178680543088794,
14.1804778828799));
#29374=CARTESIAN_POINT('Ctrl Pts',(-9.71752512830443,-1.58793609723457E-5,
14.1874873996035));
#29375=CARTESIAN_POINT('Ctrl Pts',(-9.7174151537438,-2.95534814072282E-5,
13.8625126003965));
#29376=CARTESIAN_POINT('Ctrl Pts',(-9.71746324432392,-0.05909627943313,
13.8648289877801));
#29377=CARTESIAN_POINT('Ctrl Pts',(-9.69914882474038,-0.314937855799663,
13.87486334878));
#29378=CARTESIAN_POINT('Ctrl Pts',(-9.52277717161101,-0.746471281904888,
13.8926156833963));
#29379=CARTESIAN_POINT('Ctrl Pts',(-9.05688631633702,-1.13717009764717,
13.9157696042454));
#29380=CARTESIAN_POINT('Ctrl Pts',(-8.46258916536876,-1.26565565606363,
13.9389235250945));
#29381=CARTESIAN_POINT('Ctrl Pts',(-7.87691591618916,-1.10229229667761,
13.9620774459436));
#29382=CARTESIAN_POINT('Ctrl Pts',(-7.43492027566404,-0.684753533801549,
13.9852313667927));
#29383=CARTESIAN_POINT('Ctrl Pts',(-7.23851986425691,-0.109317520883414,
14.0083852876418));
#29384=CARTESIAN_POINT('Ctrl Pts',(-7.33300329226471,0.491325669494413,
14.0315392084909));
#29385=CARTESIAN_POINT('Ctrl Pts',(-7.6965833349978,0.978674626363476,14.05469312934));
#29386=CARTESIAN_POINT('Ctrl Pts',(-8.24542256676704,1.24035181775585,14.077847050189));
#29387=CARTESIAN_POINT('Ctrl Pts',(-8.8529645573119,1.21601741100899,14.1010009710381));
#29388=CARTESIAN_POINT('Ctrl Pts',(-9.37911677604257,0.911282619288843,
14.1241548918872));
#29389=CARTESIAN_POINT('Ctrl Pts',(-9.66553572491195,0.455344208231389,
14.14465876834));
#29390=CARTESIAN_POINT('Ctrl Pts',(-9.71730446622554,0.12921658741071,14.1574446711764));
#29391=CARTESIAN_POINT('Ctrl Pts',(-9.7173946780644,-2.21442813102893E-5,
14.1625126003965));
#29392=CARTESIAN_POINT('Ctrl Pts',(-7.70661869325992,-0.687936125025717,
13.8));
#29393=CARTESIAN_POINT('Ctrl Pts',(-7.59541735366082,-0.559690113640457,
13.8077179736164));
#29394=CARTESIAN_POINT('Ctrl Pts',(-7.43647625507643,-0.24836978034843,
13.8231539208491));
#29395=CARTESIAN_POINT('Ctrl Pts',(-7.44330893610161,0.27607510271298,13.8463078416982));
#29396=CARTESIAN_POINT('Ctrl Pts',(-7.69382532330059,0.736799251308305,
13.8694617625473));
#29397=CARTESIAN_POINT('Ctrl Pts',(-8.1302326392485,1.02765925647027,13.8926156833963));
#29398=CARTESIAN_POINT('Ctrl Pts',(-8.65190777128926,1.08153816631997,13.9157696042454));
#29399=CARTESIAN_POINT('Ctrl Pts',(-9.13855341160078,0.886033018437155,
13.9389235250945));
#29400=CARTESIAN_POINT('Ctrl Pts',(-9.47795624898969,0.486215233061711,
13.9620774459436));
#29401=CARTESIAN_POINT('Ctrl Pts',(-9.59185274523544,-0.0257170490500127,
13.9852313667927));
#29402=CARTESIAN_POINT('Ctrl Pts',(-9.45398002306975,-0.531719918561346,
14.0083852876418));
#29403=CARTESIAN_POINT('Ctrl Pts',(-9.09612983483313,-0.915113659277255,
14.0315392084909));
#29404=CARTESIAN_POINT('Ctrl Pts',(-8.60081862648673,-1.08749229554162,
14.05469312934));
#29405=CARTESIAN_POINT('Ctrl Pts',(-8.08225972767768,-1.009106985362,14.077847050189));
#29406=CARTESIAN_POINT('Ctrl Pts',(-7.66002719286643,-0.698032622614111,
14.1010009710381));
#29407=CARTESIAN_POINT('Ctrl Pts',(-7.43148323801536,-0.225999524250339,
14.1241548918872));
#29408=CARTESIAN_POINT('Ctrl Pts',(-7.44932761452541,0.298146597088897,
14.1473088127363));
#29409=CARTESIAN_POINT('Ctrl Pts',(-7.70944560160856,0.753543362642926,
14.1704627335854));
#29410=CARTESIAN_POINT('Ctrl Pts',(-8.151856824771,1.03518123285875,14.1936166544345));
#29411=CARTESIAN_POINT('Ctrl Pts',(-8.67454607303319,1.07811758364374,14.2167705752836));
#29412=CARTESIAN_POINT('Ctrl Pts',(-9.15698689756985,0.872451759132174,
14.2399244961327));
#29413=CARTESIAN_POINT('Ctrl Pts',(-9.48793369752679,0.465608059353192,
14.2630784169817));
#29414=CARTESIAN_POINT('Ctrl Pts',(-9.59107374460138,-0.0485997888996519,
14.2862323378308));
#29415=CARTESIAN_POINT('Ctrl Pts',(-9.44262406702728,-0.551601055014103,
14.3093862586799));
#29416=CARTESIAN_POINT('Ctrl Pts',(-9.07681554397107,-0.927409124320201,
14.332540179529));
#29417=CARTESIAN_POINT('Ctrl Pts',(-8.57799963750299,-1.08936674824603,
14.3556941003781));
#29418=CARTESIAN_POINT('Ctrl Pts',(-8.06119786397678,-1.00012826230345,
14.3788480212272));
#29419=CARTESIAN_POINT('Ctrl Pts',(-7.64557908483643,-0.680271089615787,
14.4020019420763));
#29420=CARTESIAN_POINT('Ctrl Pts',(-7.42698046481824,-0.203550811234991,
14.4251558629254));
#29421=CARTESIAN_POINT('Ctrl Pts',(-7.45580846534574,0.320106067722181,
14.4483097837745));
#29422=CARTESIAN_POINT('Ctrl Pts',(-7.72541566340981,0.769949973144512,
14.4714637046235));
#29423=CARTESIAN_POINT('Ctrl Pts',(-8.1736335749289,1.0422517988578,14.4946176254726));
#29424=CARTESIAN_POINT('Ctrl Pts',(-8.69710803021792,1.07422170898761,14.5177715463217));
#29425=CARTESIAN_POINT('Ctrl Pts',(-9.17513152007603,0.858487790381764,
14.5409254671708));
#29426=CARTESIAN_POINT('Ctrl Pts',(-9.49747703301279,0.444795935515361,
14.5640793880199));
#29427=CARTESIAN_POINT('Ctrl Pts',(-9.58981520380618,-0.0714610186370064,
14.587233308869));
#29428=CARTESIAN_POINT('Ctrl Pts',(-9.43085385576899,-0.571239840031833,
14.6103872297181));
#29429=CARTESIAN_POINT('Ctrl Pts',(-9.05724774477506,-0.939296974650035,
14.6335411505671));
#29430=CARTESIAN_POINT('Ctrl Pts',(-8.55514637183314,-1.09076245501251,
14.6566950714162));
#29431=CARTESIAN_POINT('Ctrl Pts',(-8.04032884594654,-0.990709990816833,
14.6798489922653));
#29432=CARTESIAN_POINT('Ctrl Pts',(-7.63150648296805,-0.662210590518583,
14.7030029131144));
#29433=CARTESIAN_POINT('Ctrl Pts',(-7.42294926740862,-0.181012639402946,
14.7261568339635));
#29434=CARTESIAN_POINT('Ctrl Pts',(-7.46274822360797,0.341924856256622,
14.7493107548126));
#29435=CARTESIAN_POINT('Ctrl Pts',(-7.74172614251806,0.786018201228814,
14.7724646756617));
#29436=CARTESIAN_POINT('Ctrl Pts',(-8.19555376064367,1.04886431262541,14.7956185965108));
#29437=CARTESIAN_POINT('Ctrl Pts',(-8.71958335635884,1.06985372487855,14.8187725173598));
#29438=CARTESIAN_POINT('Ctrl Pts',(-9.19297944295253,0.844146539384165,
14.8419264382089));
#29439=CARTESIAN_POINT('Ctrl Pts',(-9.50658196876613,0.423788307447097,
14.865080359058));
#29440=CARTESIAN_POINT('Ctrl Pts',(-9.58807775575186,-0.0942907930237714,
14.8882342799071));
#29441=CARTESIAN_POINT('Ctrl Pts',(-9.41867443891702,-0.590627682360479,
14.9113882007562));
#29442=CARTESIAN_POINT('Ctrl Pts',(-9.03743528136299,-0.950771789729547,
14.9345421216053));
#29443=CARTESIAN_POINT('Ctrl Pts',(-8.53226836097154,-1.09167931285156,
14.9576960424544));
#29444=CARTESIAN_POINT('Ctrl Pts',(-8.01966297638898,-0.980855300201485,
14.9808499633034));
#29445=CARTESIAN_POINT('Ctrl Pts',(-7.617813225467,-0.643861742399126,15.0040038841525));
#29446=CARTESIAN_POINT('Ctrl Pts',(-7.41939690868525,-0.158390988130214,
15.0271578050016));
#29447=CARTESIAN_POINT('Ctrl Pts',(-7.47013353180666,0.363577398295972,
15.0503117258507));
#29448=CARTESIAN_POINT('Ctrl Pts',(-7.75839866563354,0.801746696078297,
15.0734656466998));
#29449=CARTESIAN_POINT('Ctrl Pts',(-8.06451081542916,0.970500879693927,
15.0889015939325));
#29450=CARTESIAN_POINT('Ctrl Pts',(-8.22848181102371,1.01439039972539,15.0966195675489));
#29451=CARTESIAN_POINT('Ctrl Pts',(-7.66447275106935,-0.724480616192607,
13.7677934774837));
#29452=CARTESIAN_POINT('Ctrl Pts',(-7.54736418225973,-0.589421929822323,
13.7755114511001));
#29453=CARTESIAN_POINT('Ctrl Pts',(-7.37997982657345,-0.261563661166546,
13.7909473983328));
#29454=CARTESIAN_POINT('Ctrl Pts',(-7.38717547276688,0.290740743584966,
13.8141013191819));
#29455=CARTESIAN_POINT('Ctrl Pts',(-7.65099977267187,0.775939445799765,
13.837255240031));
#29456=CARTESIAN_POINT('Ctrl Pts',(-8.11058988528164,1.08225049431121,13.8604091608801));
#29457=CARTESIAN_POINT('Ctrl Pts',(-8.65997740450681,1.13899155556342,13.8835630817291));
#29458=CARTESIAN_POINT('Ctrl Pts',(-9.17247459797395,0.933100797897987,
13.9067170025782));
#29459=CARTESIAN_POINT('Ctrl Pts',(-9.52990716740014,0.512043922155726,
13.9298709234273));
#29460=CARTESIAN_POINT('Ctrl Pts',(-9.64985406476538,-0.027083188198195,
13.9530248442764));
#29461=CARTESIAN_POINT('Ctrl Pts',(-9.50465727820759,-0.559965904140891,
13.9761787651255));
#29462=CARTESIAN_POINT('Ctrl Pts',(-9.12779739914742,-0.963726258356724,
13.9993326859746));
#29463=CARTESIAN_POINT('Ctrl Pts',(-8.60617430599108,-1.14526197959041,
14.0224866068237));
#29464=CARTESIAN_POINT('Ctrl Pts',(-8.06006856030532,-1.06271269085048,
14.0456405276728));
#29465=CARTESIAN_POINT('Ctrl Pts',(-7.61540622049117,-0.735113459167605,
14.0687944485218));
#29466=CARTESIAN_POINT('Ctrl Pts',(-7.37472157083505,-0.238005054004107,
14.0919483693709));
#29467=CARTESIAN_POINT('Ctrl Pts',(-7.39351387497389,0.313984718227464,
14.11510229022));
#29468=CARTESIAN_POINT('Ctrl Pts',(-7.66744983023097,0.793573036559154,
14.1382562110691));
#29469=CARTESIAN_POINT('Ctrl Pts',(-8.13336278916342,1.09017205256447,14.1614101319182));
#29470=CARTESIAN_POINT('Ctrl Pts',(-8.68381829641576,1.13538926495116,14.1845640527673));
#29471=CARTESIAN_POINT('Ctrl Pts',(-9.19188730620024,0.918798075956213,
14.2077179736164));
#29472=CARTESIAN_POINT('Ctrl Pts',(-9.54041463720908,0.490342055713144,
14.2308718944655));
#29473=CARTESIAN_POINT('Ctrl Pts',(-9.64903368211814,-0.0511815032355429,
14.2540258153145));
#29474=CARTESIAN_POINT('Ctrl Pts',(-9.4926980719211,-0.580903164831139,
14.2771797361636));
#29475=CARTESIAN_POINT('Ctrl Pts',(-9.10745709597677,-0.976674882170243,
14.3003336570127));
#29476=CARTESIAN_POINT('Ctrl Pts',(-8.58214312838834,-1.1472360068306,14.3234875778618));
#29477=CARTESIAN_POINT('Ctrl Pts',(-8.03788784986273,-1.05325700073994,
14.3466414987109));
#29478=CARTESIAN_POINT('Ctrl Pts',(-7.6001906011515,-0.716408399347305,
14.36979541956));
#29479=CARTESIAN_POINT('Ctrl Pts',(-7.36997960165833,-0.214363822141945,
14.3929493404091));
#29480=CARTESIAN_POINT('Ctrl Pts',(-7.40033900106474,0.337110718210485,
14.4161032612582));
#29481=CARTESIAN_POINT('Ctrl Pts',(-7.68426825245581,0.810851197791604,
14.4392571821072));
#29482=CARTESIAN_POINT('Ctrl Pts',(-8.15629636220767,1.09761822063948,14.4624111029563));
#29483=CARTESIAN_POINT('Ctrl Pts',(-8.70757878819557,1.13128643393415,14.4855650238054));
#29484=CARTESIAN_POINT('Ctrl Pts',(-9.21099580598046,0.904092314306593,
14.5087189446545));
#29485=CARTESIAN_POINT('Ctrl Pts',(-9.55046493304603,0.468424351795872,
14.5318728655036));
#29486=CARTESIAN_POINT('Ctrl Pts',(-9.64770828521333,-0.0752571655020362,
14.5550267863527));
#29487=CARTESIAN_POINT('Ctrl Pts',(-9.48030260438434,-0.601585199911631,
14.5781807072018));
#29488=CARTESIAN_POINT('Ctrl Pts',(-9.08684981762149,-0.989194237992473,
14.6013346280509));
#29489=CARTESIAN_POINT('Ctrl Pts',(-8.55807585325594,-1.14870585622711,
14.6244885488999));
#29490=CARTESIAN_POINT('Ctrl Pts',(-8.01591022942404,-1.04333841254276,
14.647642469749));
#29491=CARTESIAN_POINT('Ctrl Pts',(-7.58537043558358,-0.697388491773475,
14.6707963905981));
#29492=CARTESIAN_POINT('Ctrl Pts',(-7.36573425928267,-0.190628379238543,
14.6939503114472));
#29493=CARTESIAN_POINT('Ctrl Pts',(-7.40764741264418,0.360088562790776,
14.7171042322963));
#29494=CARTESIAN_POINT('Ctrl Pts',(-7.70144517561027,0.827773001081413,
14.7402581531454));
#29495=CARTESIAN_POINT('Ctrl Pts',(-8.1793809903817,1.10458200386683,14.7634120739945));
#29496=CARTESIAN_POINT('Ctrl Pts',(-8.73124804692375,1.1266864141013,14.7865659948435));
#29497=CARTESIAN_POINT('Ctrl Pts',(-9.22979184487555,0.888989228450584,
14.8097199156926));
#29498=CARTESIAN_POINT('Ctrl Pts',(-9.56005354051264,0.446300758087122,
14.8328738365417));
#29499=CARTESIAN_POINT('Ctrl Pts',(-9.64587854057396,-0.0992997014491682,
14.8560277573908));
#29500=CARTESIAN_POINT('Ctrl Pts',(-9.46747619346509,-0.622002961744356,
14.8791816782399));
#29501=CARTESIAN_POINT('Ctrl Pts',(-9.06598487801604,-1.00127861733684,
14.902335599089));
#29502=CARTESIAN_POINT('Ctrl Pts',(-8.53398251841959,-1.14967141931943,
14.9254895199381));
#29503=CARTESIAN_POINT('Ctrl Pts',(-7.99414654909593,-1.03296022179267,
14.9486434407871));
#29504=CARTESIAN_POINT('Ctrl Pts',(-7.57094976588598,-0.678064917522287,
14.9717973616362));
#29505=CARTESIAN_POINT('Ctrl Pts',(-7.36199319242599,-0.166805022305877,
14.9949512824853));
#29506=CARTESIAN_POINT('Ctrl Pts',(-7.41542504263034,0.382891329542149,
15.0181052033344));
#29507=CARTESIAN_POINT('Ctrl Pts',(-7.71900337524653,0.844337023853018,
15.0412591241835));
#29508=CARTESIAN_POINT('Ctrl Pts',(-8.04137679167335,1.02205575453657,15.0566950714162));
#29509=CARTESIAN_POINT('Ctrl Pts',(-8.21405824218101,1.06827677035487,15.0644130450326));
#29510=CARTESIAN_POINT('Ctrl Pts',(-7.62232680887878,-0.761025107359497,
13.7355869549674));
#29511=CARTESIAN_POINT('Ctrl Pts',(-7.49931101085863,-0.619153746004188,
13.7433049285838));
#29512=CARTESIAN_POINT('Ctrl Pts',(-7.32348339807046,-0.274757541984661,
13.7587408758165));
#29513=CARTESIAN_POINT('Ctrl Pts',(-7.33104200943215,0.305406384456951,
13.7818947966656));
#29514=CARTESIAN_POINT('Ctrl Pts',(-7.60817422204316,0.815079640291225,
13.8050487175147));
#29515=CARTESIAN_POINT('Ctrl Pts',(-8.09094713131479,1.13684173215214,13.8282026383638));
#29516=CARTESIAN_POINT('Ctrl Pts',(-8.66804703772436,1.19644494480687,13.8513565592128));
#29517=CARTESIAN_POINT('Ctrl Pts',(-9.20639578434712,0.980168577358818,
13.8745104800619));
#29518=CARTESIAN_POINT('Ctrl Pts',(-9.58185808581058,0.537872611249743,
13.897664400911));
#29519=CARTESIAN_POINT('Ctrl Pts',(-9.70785538429531,-0.0284493273463784,
13.9208183217601));
#29520=CARTESIAN_POINT('Ctrl Pts',(-9.55533453334542,-0.588211889720436,
13.9439722426092));
#29521=CARTESIAN_POINT('Ctrl Pts',(-9.15946496346172,-1.01233885743619,
13.9671261634583));
#29522=CARTESIAN_POINT('Ctrl Pts',(-8.61152998549543,-1.20303166363919,
13.9902800843074));
#29523=CARTESIAN_POINT('Ctrl Pts',(-8.03787739293296,-1.11631839633895,
14.0134340051565));
#29524=CARTESIAN_POINT('Ctrl Pts',(-7.5707852481159,-0.772194295721099,
14.0365879260055));
#29525=CARTESIAN_POINT('Ctrl Pts',(-7.31795990365474,-0.250010583757875,
14.0597418468546));
#29526=CARTESIAN_POINT('Ctrl Pts',(-7.33770013542236,0.32982283936603,14.0828957677037));
#29527=CARTESIAN_POINT('Ctrl Pts',(-7.62545405885339,0.833602710475383,
14.1060496885528));
#29528=CARTESIAN_POINT('Ctrl Pts',(-8.11486875355584,1.14516287227018,14.1292036094019));
#29529=CARTESIAN_POINT('Ctrl Pts',(-8.69309051979833,1.19266094625859,14.152357530251));
#29530=CARTESIAN_POINT('Ctrl Pts',(-9.22678771483062,0.965144392780252,
14.1755114511001));
#29531=CARTESIAN_POINT('Ctrl Pts',(-9.59289557689136,0.515076052073095,
14.1986653719492));
#29532=CARTESIAN_POINT('Ctrl Pts',(-9.70699361963491,-0.0537632175714332,
14.2218192927982));
#29533=CARTESIAN_POINT('Ctrl Pts',(-9.54277207681493,-0.610205274648177,
14.2449732136473));
#29534=CARTESIAN_POINT('Ctrl Pts',(-9.13809864798247,-1.02594064002028,
14.2681271344964));
#29535=CARTESIAN_POINT('Ctrl Pts',(-8.58628661927369,-1.20510526541518,
14.2912810553455));
#29536=CARTESIAN_POINT('Ctrl Pts',(-8.01457783574869,-1.10638573917644,
14.3144349761946));
#29537=CARTESIAN_POINT('Ctrl Pts',(-7.55480211746658,-0.752545709078824,
14.3375888970437));
#29538=CARTESIAN_POINT('Ctrl Pts',(-7.31297873849841,-0.225176833048898,
14.3607428178928));
#29539=CARTESIAN_POINT('Ctrl Pts',(-7.34486953678376,0.35411536869879,14.3838967387419));
#29540=CARTESIAN_POINT('Ctrl Pts',(-7.64312084150182,0.851752422438698,
14.4070506595909));
#29541=CARTESIAN_POINT('Ctrl Pts',(-8.13895914948646,1.15298464242117,14.43020458044));
#29542=CARTESIAN_POINT('Ctrl Pts',(-8.71804954617321,1.18835115888069,14.4533585012891));
#29543=CARTESIAN_POINT('Ctrl Pts',(-9.24686009188489,0.949696838231421,
14.4765124221382));
#29544=CARTESIAN_POINT('Ctrl Pts',(-9.60345283307926,0.492052768076384,
14.4996663429873));
#29545=CARTESIAN_POINT('Ctrl Pts',(-9.70560136662048,-0.0790533123670655,
14.5228202638364));
#29546=CARTESIAN_POINT('Ctrl Pts',(-9.52975135299969,-0.63193055979143,
14.5459741846855));
#29547=CARTESIAN_POINT('Ctrl Pts',(-9.11645189046791,-1.03909150133491,
14.5691281055345));
#29548=CARTESIAN_POINT('Ctrl Pts',(-8.56100533467875,-1.2066492574417,14.5922820263836));
#29549=CARTESIAN_POINT('Ctrl Pts',(-7.99149161290154,-1.09596683426869,
14.6154359472327));
#29550=CARTESIAN_POINT('Ctrl Pts',(-7.53923438819912,-0.732566393028366,
14.6385898680818));
#29551=CARTESIAN_POINT('Ctrl Pts',(-7.30851925115672,-0.200244119074141,
14.6617437889309));
#29552=CARTESIAN_POINT('Ctrl Pts',(-7.3525466016804,0.37825226932493,14.68489770978));
#29553=CARTESIAN_POINT('Ctrl Pts',(-7.66116420870248,0.869527800934012,
14.7080516306291));
#29554=CARTESIAN_POINT('Ctrl Pts',(-8.16320822011973,1.16029969510826,14.7312055514782));
#29555=CARTESIAN_POINT('Ctrl Pts',(-8.74291273748866,1.18351910332405,14.7543594723272));
#29556=CARTESIAN_POINT('Ctrl Pts',(-9.26660424679858,0.933831917517003,
14.7775133931763));
#29557=CARTESIAN_POINT('Ctrl Pts',(-9.61352511225915,0.468813208727148,
14.8006673140254));
#29558=CARTESIAN_POINT('Ctrl Pts',(-9.70367932539607,-0.104308609874565,
14.8238212348745));
#29559=CARTESIAN_POINT('Ctrl Pts',(-9.51627794801315,-0.653378241128233,
14.8469751557236));
#29560=CARTESIAN_POINT('Ctrl Pts',(-9.09453447466908,-1.05178544494412,
14.8701290765727));
#29561=CARTESIAN_POINT('Ctrl Pts',(-8.53569667586763,-1.20766352578729,
14.8932829974218));
#29562=CARTESIAN_POINT('Ctrl Pts',(-7.96863012180288,-1.08506514338386,
14.9164369182709));
#29563=CARTESIAN_POINT('Ctrl Pts',(-7.52408630630496,-0.712268092645449,
14.9395908391199));
#29564=CARTESIAN_POINT('Ctrl Pts',(-7.30458947616674,-0.175219056481539,
14.962744759969));
#29565=CARTESIAN_POINT('Ctrl Pts',(-7.36071655345402,0.402205260788326,
14.9858986808181));
#29566=CARTESIAN_POINT('Ctrl Pts',(-7.67960808485951,0.886927351627739,
15.0090526016672));
#29567=CARTESIAN_POINT('Ctrl Pts',(-8.01824276791754,1.07361062937921,15.0244885488999));
#29568=CARTESIAN_POINT('Ctrl Pts',(-8.1996346733383,1.12216314098435,15.0322065225163));
#29569=CARTESIAN_POINT('Ctrl Pts',(-7.58018086668821,-0.797569598526387,
13.7033804324511));
#29570=CARTESIAN_POINT('Ctrl Pts',(-7.45125783945754,-0.648885562186053,
13.7110984060675));
#29571=CARTESIAN_POINT('Ctrl Pts',(-7.26698696956747,-0.287951422802777,
13.7265343533002));
#29572=CARTESIAN_POINT('Ctrl Pts',(-7.27490854609742,0.320072025328937,
13.7496882741493));
#29573=CARTESIAN_POINT('Ctrl Pts',(-7.56534867141445,0.854219834782685,
13.7728421949984));
#29574=CARTESIAN_POINT('Ctrl Pts',(-8.07130437734794,1.19143296999308,13.7959961158475));
#29575=CARTESIAN_POINT('Ctrl Pts',(-8.67611667094192,1.25389833405033,13.8191500366966));
#29576=CARTESIAN_POINT('Ctrl Pts',(-9.24031697072028,1.02723635681965,13.8423039575456));
#29577=CARTESIAN_POINT('Ctrl Pts',(-9.63380900422103,0.563701300343758,
13.8654578783947));
#29578=CARTESIAN_POINT('Ctrl Pts',(-9.76585670382525,-0.0298154664945606,
13.8886117992438));
#29579=CARTESIAN_POINT('Ctrl Pts',(-9.60601178848326,-0.616457875299982,
13.9117657200929));
#29580=CARTESIAN_POINT('Ctrl Pts',(-9.19113252777601,-1.06095145651566,
13.934919640942));
#29581=CARTESIAN_POINT('Ctrl Pts',(-8.61688566499978,-1.26080134768798,
13.9580735617911));
#29582=CARTESIAN_POINT('Ctrl Pts',(-8.0156862255606,-1.16992410182742,13.9812274826402));
#29583=CARTESIAN_POINT('Ctrl Pts',(-7.52616427574063,-0.809275132274592,
14.0043814034892));
#29584=CARTESIAN_POINT('Ctrl Pts',(-7.26119823647443,-0.262016113511643,
14.0275353243383));
#29585=CARTESIAN_POINT('Ctrl Pts',(-7.28188639587083,0.345660960504597,
14.0506892451874));
#29586=CARTESIAN_POINT('Ctrl Pts',(-7.5834582874758,0.873632384391611,14.0738431660365));
#29587=CARTESIAN_POINT('Ctrl Pts',(-8.09637471794825,1.2001536919759,14.0969970868856));
#29588=CARTESIAN_POINT('Ctrl Pts',(-8.7023627431809,1.24993262756601,14.1201510077347));
#29589=CARTESIAN_POINT('Ctrl Pts',(-9.26168812346101,1.01149070960429,14.1433049285838));
#29590=CARTESIAN_POINT('Ctrl Pts',(-9.64537651657365,0.539810048433048,
14.1664588494329));
#29591=CARTESIAN_POINT('Ctrl Pts',(-9.76495355715166,-0.0563449319073242,
14.1896127702819));
#29592=CARTESIAN_POINT('Ctrl Pts',(-9.59284608170875,-0.639507384465213,
14.212766691131));
#29593=CARTESIAN_POINT('Ctrl Pts',(-9.16874019998817,-1.07520639787033,
14.2359206119801));
#29594=CARTESIAN_POINT('Ctrl Pts',(-8.59043011015904,-1.26297452399975,
14.2590745328292));
#29595=CARTESIAN_POINT('Ctrl Pts',(-7.99126782163464,-1.15951447761293,
14.2822284536783));
#29596=CARTESIAN_POINT('Ctrl Pts',(-7.50941363378165,-0.788683018810342,
14.3053823745274));
#29597=CARTESIAN_POINT('Ctrl Pts',(-7.25597787533851,-0.235989843955851,
14.3285362953765));
#29598=CARTESIAN_POINT('Ctrl Pts',(-7.28940007250277,0.371120019187095,
14.3516902162256));
#29599=CARTESIAN_POINT('Ctrl Pts',(-7.60197343054782,0.892653647085789,
14.3748441370747));
#29600=CARTESIAN_POINT('Ctrl Pts',(-8.12162193676524,1.20835106420286,14.3979980579237));
#29601=CARTESIAN_POINT('Ctrl Pts',(-8.72852030415086,1.24541588382723,14.4211519787728));
#29602=CARTESIAN_POINT('Ctrl Pts',(-9.28272437778932,0.995301362156251,
14.4443058996219));
#29603=CARTESIAN_POINT('Ctrl Pts',(-9.65644073311249,0.515681184356895,
14.467459820471));
#29604=CARTESIAN_POINT('Ctrl Pts',(-9.76349444802764,-0.0828494592320952,
14.4906137413201));
#29605=CARTESIAN_POINT('Ctrl Pts',(-9.57920010161505,-0.662275919671228,
14.5137676621692));
#29606=CARTESIAN_POINT('Ctrl Pts',(-9.14605396331434,-1.08898876467735,
14.5369215830183));
#29607=CARTESIAN_POINT('Ctrl Pts',(-8.56393481610157,-1.2645926586563,14.5600755038673));
#29608=CARTESIAN_POINT('Ctrl Pts',(-7.96707299637902,-1.14859525599462,
14.5832294247164));
#29609=CARTESIAN_POINT('Ctrl Pts',(-7.49309834081465,-0.767744294283258,
14.6063833455655));
#29610=CARTESIAN_POINT('Ctrl Pts',(-7.25130424303077,-0.209859858909738,
14.6295372664146));
#29611=CARTESIAN_POINT('Ctrl Pts',(-7.29744579071662,0.396415975859085,
14.6526911872637));
#29612=CARTESIAN_POINT('Ctrl Pts',(-7.62088324179469,0.911282600786611,
14.6758451081128));
#29613=CARTESIAN_POINT('Ctrl Pts',(-8.14703544985776,1.21601738634968,14.6989990289619));
#29614=CARTESIAN_POINT('Ctrl Pts',(-8.75457742805358,1.2403517925468,14.722152949811));
#29615=CARTESIAN_POINT('Ctrl Pts',(-9.3034166487216,0.978674606583422,14.74530687066));
#29616=CARTESIAN_POINT('Ctrl Pts',(-9.66699668400565,0.491325659367174,
14.7684607915091));
#29617=CARTESIAN_POINT('Ctrl Pts',(-9.76148011021817,-0.109317518299962,
14.7916147123582));
#29618=CARTESIAN_POINT('Ctrl Pts',(-9.56507970256121,-0.68475352051211,
14.8147686332073));
#29619=CARTESIAN_POINT('Ctrl Pts',(-9.12308407132213,-1.10229227255141,
14.8379225540564));
#29620=CARTESIAN_POINT('Ctrl Pts',(-8.53741083331568,-1.26565563225515,
14.8610764749055));
#29621=CARTESIAN_POINT('Ctrl Pts',(-7.94311369450983,-1.13717006497505,
14.8842303957546));
#29622=CARTESIAN_POINT('Ctrl Pts',(-7.47722284672394,-0.74647126776861,
14.9073843166036));
#29623=CARTESIAN_POINT('Ctrl Pts',(-7.24718575990748,-0.183633090657203,
14.9305382374527));
#29624=CARTESIAN_POINT('Ctrl Pts',(-7.3060080642777,0.421519192034503,14.9536921583018));
#29625=CARTESIAN_POINT('Ctrl Pts',(-7.64021279447249,0.92951767940246,14.9768460791509));
#29626=CARTESIAN_POINT('Ctrl Pts',(-7.99510874416173,1.12516550422186,14.9922820263836));
#29627=CARTESIAN_POINT('Ctrl Pts',(-8.18521110449559,1.17604951161383,15.));
#29628=CARTESIAN_POINT('Ctrl Pts',(-8.18521110449559,1.17604951161383,15.));
#29629=CARTESIAN_POINT('Ctrl Pts',(-8.13719918410313,1.15963858074114,15.));
#29630=CARTESIAN_POINT('Ctrl Pts',(-8.09039143005571,1.14022106600632,15.));
#29631=CARTESIAN_POINT('Ctrl Pts',(-8.04502571698153,1.11798781401985,15.));
#29632=CARTESIAN_POINT('Ctrl Pts',(-7.99968245369021,1.09576556443245,15.));
#29633=CARTESIAN_POINT('Ctrl Pts',(-7.95577890640656,1.07072966351069,15.));
#29634=CARTESIAN_POINT('Ctrl Pts',(-7.91357983441579,1.04302643998004,15.));
#29635=CARTESIAN_POINT('Ctrl Pts',(-7.87480106608641,1.01756860793323,15.));
#29636=CARTESIAN_POINT('Ctrl Pts',(-7.8374614440569,0.989857442508656,15.));
#29637=CARTESIAN_POINT('Ctrl Pts',(-7.80179646271021,0.959980963961019,
15.));
#29638=CARTESIAN_POINT('Ctrl Pts',(-7.79470070794682,0.954036865381321,
15.));
#29639=CARTESIAN_POINT('Ctrl Pts',(-7.78766969979432,0.94800553688181,15.));
#29640=CARTESIAN_POINT('Ctrl Pts',(-7.78071079958526,0.941892285934689,
15.));
#29641=CARTESIAN_POINT('Ctrl Pts',(-7.75269258257066,0.917278857583148,
15.));
#29642=CARTESIAN_POINT('Ctrl Pts',(-7.72591191331948,0.891400647665221,
15.));
#29643=CARTESIAN_POINT('Ctrl Pts',(-7.70047025475673,0.864321952622116,
15.));
#29644=CARTESIAN_POINT('Ctrl Pts',(-7.66652586503523,0.828193420536614,
15.));
#29645=CARTESIAN_POINT('Ctrl Pts',(-7.63496310561488,0.789928497182938,
15.));
#29646=CARTESIAN_POINT('Ctrl Pts',(-7.60593174101237,0.749793509612499,
15.));
#29647=CARTESIAN_POINT('Ctrl Pts',(-7.58573652511221,0.721874231609796,
15.));
#29648=CARTESIAN_POINT('Ctrl Pts',(-7.5667671232806,0.693049287271894,15.));
#29649=CARTESIAN_POINT('Ctrl Pts',(-7.54908765839019,0.663402582514798,
15.));
#29650=CARTESIAN_POINT('Ctrl Pts',(-7.53965695670849,0.64758823348654,15.));
#29651=CARTESIAN_POINT('Ctrl Pts',(-7.53059349991873,0.631539998511114,
15.));
#29652=CARTESIAN_POINT('Ctrl Pts',(-7.52190847036827,0.615270358408881,
15.));
#29653=CARTESIAN_POINT('Ctrl Pts',(-7.51748854481548,0.606990524977705,
15.));
#29654=CARTESIAN_POINT('Ctrl Pts',(-7.51316664579,0.598653347566876,15.));
#29655=CARTESIAN_POINT('Ctrl Pts',(-7.50894435340399,0.590260465682536,
15.));
#29656=CARTESIAN_POINT('Ctrl Pts',(-7.50442240551159,0.581271942132195,
15.));
#29657=CARTESIAN_POINT('Ctrl Pts',(-7.50001807492301,0.572226073963554,
15.));
#29658=CARTESIAN_POINT('Ctrl Pts',(-7.49573609254012,0.563132443556206,
15.));
#29659=CARTESIAN_POINT('Ctrl Pts',(-7.47506492170153,0.519233153254429,
15.));
#29660=CARTESIAN_POINT('Ctrl Pts',(-7.45721452036603,0.474169527752238,
15.));
#29661=CARTESIAN_POINT('Ctrl Pts',(-7.44233237690941,0.428189108276674,
15.));
#29662=CARTESIAN_POINT('Ctrl Pts',(-7.43702150858781,0.411780453574552,
15.));
#29663=CARTESIAN_POINT('Ctrl Pts',(-7.43208910475981,0.395254894640867,
15.));
#29664=CARTESIAN_POINT('Ctrl Pts',(-7.42754344368022,0.378623315021146,
15.));
#29665=CARTESIAN_POINT('Ctrl Pts',(-7.41562266198816,0.335007782237456,
15.));
#29666=CARTESIAN_POINT('Ctrl Pts',(-7.40635883556592,0.29066280905082,15.));
#29667=CARTESIAN_POINT('Ctrl Pts',(-7.39978217647955,0.245835647048946,
15.));
#29668=CARTESIAN_POINT('Ctrl Pts',(-7.397018590817,0.226998772493948,15.));
#29669=CARTESIAN_POINT('Ctrl Pts',(-7.39472997377155,0.208076803222566,
15.));
#29670=CARTESIAN_POINT('Ctrl Pts',(-7.39292062669322,0.189088525473043,
15.));
#29671=CARTESIAN_POINT('Ctrl Pts',(-7.39203074058723,0.179749574009065,
15.));
#29672=CARTESIAN_POINT('Ctrl Pts',(-7.39125667019278,0.170392618111359,
15.));
#29673=CARTESIAN_POINT('Ctrl Pts',(-7.39059946538832,0.161026195275006,
15.));
#29674=CARTESIAN_POINT('Ctrl Pts',(-7.38726347674367,0.113481989859994,
15.));
#29675=CARTESIAN_POINT('Ctrl Pts',(-7.38694625368064,0.0658815596571062,
15.));
#29676=CARTESIAN_POINT('Ctrl Pts',(-7.38964513362731,0.0185137802117043,
15.));
#29677=CARTESIAN_POINT('Ctrl Pts',(-7.39231343455405,-0.0283173098292195,
15.));
#29678=CARTESIAN_POINT('Ctrl Pts',(-7.39793005971206,-0.0749220643021994,
15.));
#29679=CARTESIAN_POINT('Ctrl Pts',(-7.40654190918745,-0.121012249417508,
15.));
#29680=CARTESIAN_POINT('Ctrl Pts',(-7.40892379251999,-0.133759969176599,
15.));
#29681=CARTESIAN_POINT('Ctrl Pts',(-7.41153508910055,-0.146468219675886,
15.));
#29682=CARTESIAN_POINT('Ctrl Pts',(-7.41437744335462,-0.159130611434646,
15.));
#29683=CARTESIAN_POINT('Ctrl Pts',(-7.41931615775307,-0.181132068996878,
15.));
#29684=CARTESIAN_POINT('Ctrl Pts',(-7.42495234417919,-0.202995174294252,
15.));
#29685=CARTESIAN_POINT('Ctrl Pts',(-7.43127605846836,-0.224688120790961,
15.));
#29686=CARTESIAN_POINT('Ctrl Pts',(-7.4344860198212,-0.235699611301021,
15.));
#29687=CARTESIAN_POINT('Ctrl Pts',(-7.43787316641254,-0.246667231430326,
15.));
#29688=CARTESIAN_POINT('Ctrl Pts',(-7.44143639509547,-0.257586640410256,
15.));
#29689=CARTESIAN_POINT('Ctrl Pts',(-7.4446649858989,-0.267480561499389,
15.));
#29690=CARTESIAN_POINT('Ctrl Pts',(-7.44803553776462,-0.277326794204636,
15.));
#29691=CARTESIAN_POINT('Ctrl Pts',(-7.45154507732052,-0.287118296675091,
15.));
#29692=CARTESIAN_POINT('Ctrl Pts',(-7.46731977428534,-0.331129193786157,
15.));
#29693=CARTESIAN_POINT('Ctrl Pts',(-7.48590786965047,-0.374063763344147,
15.));
#29694=CARTESIAN_POINT('Ctrl Pts',(-7.50719066652686,-0.415647384120069,
15.));
#29695=CARTESIAN_POINT('Ctrl Pts',(-7.51904302719296,-0.43880524603553,
15.));
#29696=CARTESIAN_POINT('Ctrl Pts',(-7.5317319029862,-0.461543654707363,
15.));
#29697=CARTESIAN_POINT('Ctrl Pts',(-7.54524209132987,-0.483810502964833,
15.));
#29698=CARTESIAN_POINT('Ctrl Pts',(-7.55097581847724,-0.493260558662993,
15.));
#29699=CARTESIAN_POINT('Ctrl Pts',(-7.55685694084107,-0.502624435497839,
15.));
#29700=CARTESIAN_POINT('Ctrl Pts',(-7.56287744573998,-0.511888023199772,
15.));
#29701=CARTESIAN_POINT('Ctrl Pts',(-7.58817054843871,-0.550805834751792,
15.));
#29702=CARTESIAN_POINT('Ctrl Pts',(-7.61595074867493,-0.588006977343887,
15.));
#29703=CARTESIAN_POINT('Ctrl Pts',(-7.64611669191102,-0.623204223528289,
15.));
#29704=CARTESIAN_POINT('Ctrl Pts',(-7.66532331964563,-0.645614277126032,
15.));
#29705=CARTESIAN_POINT('Ctrl Pts',(-7.68549798951779,-0.667211207796954,
15.));
#29706=CARTESIAN_POINT('Ctrl Pts',(-7.70658096099555,-0.687940818620793,
15.));
#29707=CARTESIAN_POINT('Ctrl Pts',(-7.70661869325992,-0.687936125025717,
13.8));
#29708=CARTESIAN_POINT('Ctrl Pts',(-7.67409790832043,-0.65590132663166,
13.8));
#29709=CARTESIAN_POINT('Ctrl Pts',(-7.64381311621299,-0.621806798728219,
13.8));
#29710=CARTESIAN_POINT('Ctrl Pts',(-7.61585476886247,-0.585951934642269,
13.8));
#29711=CARTESIAN_POINT('Ctrl Pts',(-7.58749800537564,-0.549586126320677,
13.8));
#29712=CARTESIAN_POINT('Ctrl Pts',(-7.56153373633204,-0.511408666095284,
13.8));
#29713=CARTESIAN_POINT('Ctrl Pts',(-7.53808668428465,-0.471686692826258,
13.8));
#29714=CARTESIAN_POINT('Ctrl Pts',(-7.51732520369006,-0.436514383081886,
13.8));
#29715=CARTESIAN_POINT('Ctrl Pts',(-7.49853744049679,-0.40013004713118,
13.8));
#29716=CARTESIAN_POINT('Ctrl Pts',(-7.48183644885479,-0.362697961579565,
13.8));
#29717=CARTESIAN_POINT('Ctrl Pts',(-7.477109485266,-0.352103374788074,13.8));
#29718=CARTESIAN_POINT('Ctrl Pts',(-7.47254853386425,-0.341421047886299,
13.8));
#29719=CARTESIAN_POINT('Ctrl Pts',(-7.46816654485215,-0.330680261275302,
13.8));
#29720=CARTESIAN_POINT('Ctrl Pts',(-7.45706638332686,-0.30347241890934,
13.8));
#29721=CARTESIAN_POINT('Ctrl Pts',(-7.44710002577023,-0.275860115753735,
13.8));
#29722=CARTESIAN_POINT('Ctrl Pts',(-7.43829488164217,-0.247911966218546,
13.8));
#29723=CARTESIAN_POINT('Ctrl Pts',(-7.42417532395293,-0.203095492583373,
13.8));
#29724=CARTESIAN_POINT('Ctrl Pts',(-7.41303896601868,-0.157416559281343,
13.8));
#29725=CARTESIAN_POINT('Ctrl Pts',(-7.40485046498018,-0.111178664922763,
13.8));
#29726=CARTESIAN_POINT('Ctrl Pts',(-7.399063774025,-0.0785030379901238,
13.8));
#29727=CARTESIAN_POINT('Ctrl Pts',(-7.39475021303378,-0.0455475244970284,
13.8));
#29728=CARTESIAN_POINT('Ctrl Pts',(-7.39191194648372,-0.0124134397669909,
13.8));
#29729=CARTESIAN_POINT('Ctrl Pts',(-7.39015335429547,0.00811646520966508,
13.8));
#29730=CARTESIAN_POINT('Ctrl Pts',(-7.38896137677175,0.0287150012886081,
13.8));
#29731=CARTESIAN_POINT('Ctrl Pts',(-7.38833895669897,0.0493584273596811,
13.8));
#29732=CARTESIAN_POINT('Ctrl Pts',(-7.38797680356068,0.0613697391144699,
13.8));
#29733=CARTESIAN_POINT('Ctrl Pts',(-7.38780768251601,0.0734006750408645,
13.8));
#29734=CARTESIAN_POINT('Ctrl Pts',(-7.38783191166033,0.0854177210780557,
13.8));
#29735=CARTESIAN_POINT('Ctrl Pts',(-7.38792937970413,0.133759418733823,
13.8));
#29736=CARTESIAN_POINT('Ctrl Pts',(-7.39114708267554,0.181957500267464,
13.8));
#29737=CARTESIAN_POINT('Ctrl Pts',(-7.39745279060964,0.229700973635331,
13.8));
#29738=CARTESIAN_POINT('Ctrl Pts',(-7.39992953931477,0.248453600156905,
13.8));
#29739=CARTESIAN_POINT('Ctrl Pts',(-7.40288323259558,0.267136279136232,
13.8));
#29740=CARTESIAN_POINT('Ctrl Pts',(-7.40631404968938,0.285730658351667,
13.8));
#29741=CARTESIAN_POINT('Ctrl Pts',(-7.41475420643096,0.33147471022025,13.8));
#29742=CARTESIAN_POINT('Ctrl Pts',(-7.42607873358428,0.376684794101564,
13.8));
#29743=CARTESIAN_POINT('Ctrl Pts',(-7.44015748288889,0.421130921718887,
13.8));
#29744=CARTESIAN_POINT('Ctrl Pts',(-7.44619773201859,0.440199780596242,
13.8));
#29745=CARTESIAN_POINT('Ctrl Pts',(-7.45274552285538,0.459127950334225,
13.8));
#29746=CARTESIAN_POINT('Ctrl Pts',(-7.45979307537158,0.477896691038924,
13.8));
#29747=CARTESIAN_POINT('Ctrl Pts',(-7.46424191712361,0.489744656284764,
13.8));
#29748=CARTESIAN_POINT('Ctrl Pts',(-7.46889207365577,0.50153379748079,13.8));
#29749=CARTESIAN_POINT('Ctrl Pts',(-7.47372950591637,0.513230703803242,
13.8));
#29750=CARTESIAN_POINT('Ctrl Pts',(-7.49246787387759,0.558540058615907,
13.8));
#29751=CARTESIAN_POINT('Ctrl Pts',(-7.51403700466946,0.602538901598153,
13.8));
#29752=CARTESIAN_POINT('Ctrl Pts',(-7.53825696201999,0.644973296328836,
13.8));
#29753=CARTESIAN_POINT('Ctrl Pts',(-7.56269793086436,0.687794912590659,
13.8));
#29754=CARTESIAN_POINT('Ctrl Pts',(-7.58983864981357,0.729024481326262,
13.8));
#29755=CARTESIAN_POINT('Ctrl Pts',(-7.61954508825485,0.768389329203374,
13.8));
#29756=CARTESIAN_POINT('Ctrl Pts',(-7.62494286994729,0.775542083499952,
13.8));
#29757=CARTESIAN_POINT('Ctrl Pts',(-7.63042548902675,0.782633214974312,
13.8));
#29758=CARTESIAN_POINT('Ctrl Pts',(-7.63599230650583,0.789661002536044,
13.8));
#29759=CARTESIAN_POINT('Ctrl Pts',(-7.65116967374115,0.8088215575708,13.8));
#29760=CARTESIAN_POINT('Ctrl Pts',(-7.66697273174487,0.827511407193791,
13.8));
#29761=CARTESIAN_POINT('Ctrl Pts',(-7.68337323824041,0.845709888164107,
13.8));
#29762=CARTESIAN_POINT('Ctrl Pts',(-7.6911253557073,0.854311864099374,13.8));
#29763=CARTESIAN_POINT('Ctrl Pts',(-7.69901099219276,0.862804028438582,
13.8));
#29764=CARTESIAN_POINT('Ctrl Pts',(-7.7070273463286,0.871184032005587,13.8));
#29765=CARTESIAN_POINT('Ctrl Pts',(-7.71445506730095,0.878948699981603,
13.8));
#29766=CARTESIAN_POINT('Ctrl Pts',(-7.72198930646464,0.886611035023255,
13.8));
#29767=CARTESIAN_POINT('Ctrl Pts',(-7.72962347583117,0.894165851015352,
13.8));
#29768=CARTESIAN_POINT('Ctrl Pts',(-7.76528151517699,0.929453242866773,
13.8));
#29769=CARTESIAN_POINT('Ctrl Pts',(-7.80314150536528,0.962423770257437,
13.8));
#29770=CARTESIAN_POINT('Ctrl Pts',(-7.84293209092609,0.992921897771992,
13.8));
#29771=CARTESIAN_POINT('Ctrl Pts',(-7.86517990438843,1.00997408844301,13.8));
#29772=CARTESIAN_POINT('Ctrl Pts',(-7.88803208111194,1.02625286763951,13.8));
#29773=CARTESIAN_POINT('Ctrl Pts',(-7.91144653285245,1.04172643812877,13.8));
#29774=CARTESIAN_POINT('Ctrl Pts',(-7.92363390847077,1.04978053300143,13.8));
#29775=CARTESIAN_POINT('Ctrl Pts',(-7.93597590810809,1.05761754617181,13.8));
#29776=CARTESIAN_POINT('Ctrl Pts',(-7.94844649246672,1.06522079436794,13.8));
#29777=CARTESIAN_POINT('Ctrl Pts',(-7.99400652040546,1.09299849830535,13.8));
#29778=CARTESIAN_POINT('Ctrl Pts',(-8.04133364966062,1.11769701342198,13.8));
#29779=CARTESIAN_POINT('Ctrl Pts',(-8.09012859132893,1.13911578403477,13.8));
#29780=CARTESIAN_POINT('Ctrl Pts',(-8.12124378281263,1.15277394461815,13.8));
#29781=CARTESIAN_POINT('Ctrl Pts',(-8.15295678898405,1.16509764664083,13.8));
#29782=CARTESIAN_POINT('Ctrl Pts',(-8.1851779246473,1.17607853534585,13.8));
#29783=CARTESIAN_POINT('Ctrl Pts',(-9.55016480120948,-1.36965928395627E-5,
14.2841069671524));
#29784=CARTESIAN_POINT('Ctrl Pts',(-9.55006211521689,0.154119214996547,
14.2770974504288));
#29785=CARTESIAN_POINT('Ctrl Pts',(-9.51567268207578,0.308296476102981,
14.2700879337053));
#29786=CARTESIAN_POINT('Ctrl Pts',(-9.44996590537973,0.447714034607548,
14.2630784169817));
#29787=CARTESIAN_POINT('Ctrl Pts',(-9.37761809754114,0.601222625946185,
14.2553604433654));
#29788=CARTESIAN_POINT('Ctrl Pts',(-9.26730249755549,0.736837192539179,
14.247642469749));
#29789=CARTESIAN_POINT('Ctrl Pts',(-9.13173789347323,0.838922113254271,
14.2399244961327));
#29790=CARTESIAN_POINT('Ctrl Pts',(-8.99617328939096,0.941007033969362,
14.2322065225163));
#29791=CARTESIAN_POINT('Ctrl Pts',(-8.83535968121208,1.00956230880655,14.2244885488999));
#29792=CARTESIAN_POINT('Ctrl Pts',(-8.66783800241227,1.03668388776098,14.2167705752836));
#29793=CARTESIAN_POINT('Ctrl Pts',(-8.50031632361246,1.06380546671541,14.2090526016672));
#29794=CARTESIAN_POINT('Ctrl Pts',(-8.32608657419173,1.04949334978708,14.2013346280508));
#29795=CARTESIAN_POINT('Ctrl Pts',(-8.16523649562096,0.995397646286945,
14.1936166544345));
#29796=CARTESIAN_POINT('Ctrl Pts',(-8.00438641705019,0.941301942786809,
14.1858986808181));
#29797=CARTESIAN_POINT('Ctrl Pts',(-7.85691600932937,0.847422652714868,
14.1781807072018));
#29798=CARTESIAN_POINT('Ctrl Pts',(-7.73982780762178,0.724583546753225,
14.1704627335854));
#29799=CARTESIAN_POINT('Ctrl Pts',(-7.62273960591418,0.601744440791583,
14.162744759969));
#29800=CARTESIAN_POINT('Ctrl Pts',(-7.5360336102198,0.44994551894024,14.1550267863527));
#29801=CARTESIAN_POINT('Ctrl Pts',(-7.48970654962093,0.286688371124695,
14.1473088127363));
#29802=CARTESIAN_POINT('Ctrl Pts',(-7.44337948902206,0.123431223309151,
14.1395908391199));
#29803=CARTESIAN_POINT('Ctrl Pts',(-7.43743136351871,-0.0512841504705941,
14.1318728655036));
#29804=CARTESIAN_POINT('Ctrl Pts',(-7.47254795990888,-0.217314020421096,
14.1241548918872));
#29805=CARTESIAN_POINT('Ctrl Pts',(-7.50766455629905,-0.383343890371597,
14.1164369182709));
#29806=CARTESIAN_POINT('Ctrl Pts',(-7.58384587458274,-0.540688256492854,
14.1087189446545));
#29807=CARTESIAN_POINT('Ctrl Pts',(-7.69230862285979,-0.671206166678132,
14.1010009710381));
#29808=CARTESIAN_POINT('Ctrl Pts',(-7.80077137113685,-0.801724076863409,
14.0932829974218));
#29809=CARTESIAN_POINT('Ctrl Pts',(-7.94151554940726,-0.905415531112706,
14.0855650238054));
#29810=CARTESIAN_POINT('Ctrl Pts',(-8.09831412167731,-0.970325476600624,
14.077847050189));
#29811=CARTESIAN_POINT('Ctrl Pts',(-8.25511269394736,-1.03523542208854,
14.0701290765727));
#29812=CARTESIAN_POINT('Ctrl Pts',(-8.42796566021704,-1.06136385881508,
14.0624111029563));
#29813=CARTESIAN_POINT('Ctrl Pts',(-8.59694401140962,-1.04569830446762,
14.05469312934));
#29814=CARTESIAN_POINT('Ctrl Pts',(-8.7659223626022,-1.03003275012016,14.0469751557236));
#29815=CARTESIAN_POINT('Ctrl Pts',(-8.93102609871766,-0.97257320469871,
14.0392571821072));
#29816=CARTESIAN_POINT('Ctrl Pts',(-9.07321966481483,-0.879944475201997,
14.0315392084909));
#29817=CARTESIAN_POINT('Ctrl Pts',(-9.215413230912,-0.787315745705285,14.0238212348745));
#29818=CARTESIAN_POINT('Ctrl Pts',(-9.33469662699088,-0.659517832133316,
14.0161032612581));
#29819=CARTESIAN_POINT('Ctrl Pts',(-9.41731711205793,-0.51128506376211,
14.0083852876418));
#29820=CARTESIAN_POINT('Ctrl Pts',(-9.49993759712498,-0.363052295390903,
14.0006673140254));
#29821=CARTESIAN_POINT('Ctrl Pts',(-9.54589517118021,-0.194384672220457,
13.9929493404091));
#29822=CARTESIAN_POINT('Ctrl Pts',(-9.54989120883354,-0.0247288136166145,
13.9852313667927));
#29823=CARTESIAN_POINT('Ctrl Pts',(-9.55008526423043,-0.0164899936069937,
13.9848565669126));
#29824=CARTESIAN_POINT('Ctrl Pts',(-9.55018036327262,-0.00824884307793844,
13.9844817670325));
#29825=CARTESIAN_POINT('Ctrl Pts',(-9.55017700723911,-7.61513114500012E-6,
13.9841069671524));
#29826=CARTESIAN_POINT('Ctrl Pts',(-8.81478889550439,1.17604951161383,13.8));
#29827=CARTESIAN_POINT('Ctrl Pts',(-9.00489125583826,1.12516550422186,13.8077179736164));
#29828=CARTESIAN_POINT('Ctrl Pts',(-9.35978714971093,0.929517388355175,
13.8231539208491));
#29829=CARTESIAN_POINT('Ctrl Pts',(-9.69399194673282,0.421519158642242,
13.8463078416982));
#29830=CARTESIAN_POINT('Ctrl Pts',(-9.75281425601952,-0.18363315341468,
13.8694617625473));
#29831=CARTESIAN_POINT('Ctrl Pts',(-9.52277717161101,-0.746471281904888,
13.8926156833963));
#29832=CARTESIAN_POINT('Ctrl Pts',(-9.05688631633702,-1.13717009764717,
13.9157696042454));
#29833=CARTESIAN_POINT('Ctrl Pts',(-8.46258916536876,-1.26565565606363,
13.9389235250945));
#29834=CARTESIAN_POINT('Ctrl Pts',(-7.87691591618916,-1.10229229667761,
13.9620774459436));
#29835=CARTESIAN_POINT('Ctrl Pts',(-7.43492027566404,-0.684753533801549,
13.9852313667927));
#29836=CARTESIAN_POINT('Ctrl Pts',(-7.23851986425691,-0.109317520883414,
14.0083852876418));
#29837=CARTESIAN_POINT('Ctrl Pts',(-7.33300329226471,0.491325669494413,
14.0315392084909));
#29838=CARTESIAN_POINT('Ctrl Pts',(-7.6965833349978,0.978674626363476,14.05469312934));
#29839=CARTESIAN_POINT('Ctrl Pts',(-8.24542256676704,1.24035181775585,14.077847050189));
#29840=CARTESIAN_POINT('Ctrl Pts',(-8.8529645573119,1.21601741100899,14.1010009710381));
#29841=CARTESIAN_POINT('Ctrl Pts',(-9.37911677604257,0.911282619288843,
14.1241548918872));
#29842=CARTESIAN_POINT('Ctrl Pts',(-9.70255423368964,0.396415983899717,
14.1473088127363));
#29843=CARTESIAN_POINT('Ctrl Pts',(-9.74869578230927,-0.209859863166589,
14.1704627335854));
#29844=CARTESIAN_POINT('Ctrl Pts',(-9.50690167961977,-0.767744309864743,
14.1936166544345));
#29845=CARTESIAN_POINT('Ctrl Pts',(-9.03292701443594,-1.14859527930365,
14.2167705752836));
#29846=CARTESIAN_POINT('Ctrl Pts',(-8.43606518260107,-1.26459268432005,
14.2399244961327));
#29847=CARTESIAN_POINT('Ctrl Pts',(-7.85394602357466,-1.08898878677709,
14.2630784169817));
#29848=CARTESIAN_POINT('Ctrl Pts',(-7.4207998764838,-0.662275933111461,
14.2862323378308));
#29849=CARTESIAN_POINT('Ctrl Pts',(-7.23650552633111,-0.0828494609134307,
14.3093862586799));
#29850=CARTESIAN_POINT('Ctrl Pts',(-7.3435592434188,0.515681194822054,14.332540179529));
#29851=CARTESIAN_POINT('Ctrl Pts',(-7.71727560632613,0.995301382354801,
14.3556941003781));
#29852=CARTESIAN_POINT('Ctrl Pts',(-8.27147969121155,1.24541590910158,14.3788480212272));
#29853=CARTESIAN_POINT('Ctrl Pts',(-8.87837807091352,1.20835108872504,14.4020019420763));
#29854=CARTESIAN_POINT('Ctrl Pts',(-9.39802658767663,0.892653665201231,
14.4251558629254));
#29855=CARTESIAN_POINT('Ctrl Pts',(-9.71059995206503,0.371120026718582,
14.4483097837744));
#29856=CARTESIAN_POINT('Ctrl Pts',(-9.74402214990757,-0.235989848744997,
14.4714637046235));
#29857=CARTESIAN_POINT('Ctrl Pts',(-9.49058638632123,-0.788683034815797,
14.4946176254726));
#29858=CARTESIAN_POINT('Ctrl Pts',(-9.00873218868954,-1.159514501144,14.5177715463217));
#29859=CARTESIAN_POINT('Ctrl Pts',(-8.40956988800579,-1.26297454963044,
14.5409254671708));
#29860=CARTESIAN_POINT('Ctrl Pts',(-7.8312597864405,-1.07520641969046,14.5640793880199));
#29861=CARTESIAN_POINT('Ctrl Pts',(-7.40715389611314,-0.639507397443362,
14.587233308869));
#29862=CARTESIAN_POINT('Ctrl Pts',(-7.23504641717748,-0.0563449330507459,
14.6103872297181));
#29863=CARTESIAN_POINT('Ctrl Pts',(-7.35462346018219,0.539810059387775,
14.6335411505671));
#29864=CARTESIAN_POINT('Ctrl Pts',(-7.73831186108132,1.01149073013163,14.6566950714162));
#29865=CARTESIAN_POINT('Ctrl Pts',(-8.29763725271243,1.24993265293153,14.6798489922653));
#29866=CARTESIAN_POINT('Ctrl Pts',(-8.9036252902427,1.20015371633275,14.7030029131144));
#29867=CARTESIAN_POINT('Ctrl Pts',(-9.4165417311248,0.873632402118881,14.7261568339635));
#29868=CARTESIAN_POINT('Ctrl Pts',(-9.71811362884852,0.345660967523886,
14.7493107548126));
#29869=CARTESIAN_POINT('Ctrl Pts',(-9.73880178866775,-0.262016118838121,
14.7724646756617));
#29870=CARTESIAN_POINT('Ctrl Pts',(-9.47383574401748,-0.809275148678942,
14.7956185965108));
#29871=CARTESIAN_POINT('Ctrl Pts',(-8.98431378427829,-1.16992412560805,
14.8187725173598));
#29872=CARTESIAN_POINT('Ctrl Pts',(-8.38311433260251,-1.26080137319404,
14.8419264382089));
#29873=CARTESIAN_POINT('Ctrl Pts',(-7.80886745824715,-1.06095147820218,
14.865080359058));
#29874=CARTESIAN_POINT('Ctrl Pts',(-7.39398818892938,-0.616457887465797,
14.8882342799071));
#29875=CARTESIAN_POINT('Ctrl Pts',(-7.23414327069309,-0.0298154676920097,
14.9113882007562));
#29876=CARTESIAN_POINT('Ctrl Pts',(-7.36619097191447,0.563701313325544,
14.9345421216053));
#29877=CARTESIAN_POINT('Ctrl Pts',(-7.75968301484676,1.02723637580027,14.9576960424544));
#29878=CARTESIAN_POINT('Ctrl Pts',(-8.32388331973028,1.25389836718814,14.9808499633034));
#29879=CARTESIAN_POINT('Ctrl Pts',(-8.9286956299142,1.19143299197639,15.0040038841525));
#29880=CARTESIAN_POINT('Ctrl Pts',(-9.43465130660384,0.85421989568406,15.0271578050016));
#29881=CARTESIAN_POINT('Ctrl Pts',(-9.72509144430676,0.320072059154916,
15.0503117258507));
#29882=CARTESIAN_POINT('Ctrl Pts',(-9.73301282108904,-0.287951213042609,
15.0734656466998));
#29883=CARTESIAN_POINT('Ctrl Pts',(-9.54874216054247,-0.648885562186042,
15.0889015939325));
#29884=CARTESIAN_POINT('Ctrl Pts',(-9.4198191333118,-0.797569598526378,
15.0966195675489));
#29885=CARTESIAN_POINT('Ctrl Pts',(-8.80036532666169,1.12216314098435,13.7677934774837));
#29886=CARTESIAN_POINT('Ctrl Pts',(-8.98175723208245,1.07361062937922,13.7755114511001));
#29887=CARTESIAN_POINT('Ctrl Pts',(-9.32039186188141,0.886927073916187,
13.7909473983328));
#29888=CARTESIAN_POINT('Ctrl Pts',(-9.639283457052,0.402205228926093,13.8141013191819));
#29889=CARTESIAN_POINT('Ctrl Pts',(-9.69541053903049,-0.175219116363481,
13.837255240031));
#29890=CARTESIAN_POINT('Ctrl Pts',(-9.47591371118989,-0.712268106134006,
13.8604091608801));
#29891=CARTESIAN_POINT('Ctrl Pts',(-9.03136988854697,-1.08506517455896,
13.8835630817291));
#29892=CARTESIAN_POINT('Ctrl Pts',(-8.46430332287709,-1.20766354850487,
13.9067170025782));
#29893=CARTESIAN_POINT('Ctrl Pts',(-7.90546551341444,-1.05178546796487,
13.9298709234273));
#29894=CARTESIAN_POINT('Ctrl Pts',(-7.48372203120982,-0.653378253808753,
13.9530248442764));
#29895=CARTESIAN_POINT('Ctrl Pts',(-7.29632065024857,-0.104308612339644,
13.9761787651255));
#29896=CARTESIAN_POINT('Ctrl Pts',(-7.3864748650985,0.46881321839036,13.9993326859746));
#29897=CARTESIAN_POINT('Ctrl Pts',(-7.7333957376668,0.933831936390738,14.0224866068237));
#29898=CARTESIAN_POINT('Ctrl Pts',(-8.25708725756928,1.18351912737802,14.0456405276728));
#29899=CARTESIAN_POINT('Ctrl Pts',(-8.83679178672141,1.16029971863768,14.0687944485218));
#29900=CARTESIAN_POINT('Ctrl Pts',(-9.33883580831748,0.869527818588475,
14.0919483693709));
#29901=CARTESIAN_POINT('Ctrl Pts',(-9.64745342160757,0.378252276997143,
14.11510229022));
#29902=CARTESIAN_POINT('Ctrl Pts',(-9.69148077302225,-0.200244123135943,
14.1382562110691));
#29903=CARTESIAN_POINT('Ctrl Pts',(-9.460765631299,-0.73256640789591,14.1614101319182));
#29904=CARTESIAN_POINT('Ctrl Pts',(-9.00850839741789,-1.0959668565097,14.1845640527673));
#29905=CARTESIAN_POINT('Ctrl Pts',(-8.43899466408332,-1.20664928192954,
14.2077179736164));
#29906=CARTESIAN_POINT('Ctrl Pts',(-7.88354809702183,-1.03909152242205,
14.2308718944655));
#29907=CARTESIAN_POINT('Ctrl Pts',(-7.47024862610266,-0.631930572615834,
14.2540258153145));
#29908=CARTESIAN_POINT('Ctrl Pts',(-7.29439860891314,-0.0790533139713622,
14.2771797361636));
#29909=CARTESIAN_POINT('Ctrl Pts',(-7.39654714452737,0.49205277806203,14.3003336570127));
#29910=CARTESIAN_POINT('Ctrl Pts',(-7.75313989295838,0.949696857504478,
14.3234875778618));
#29911=CARTESIAN_POINT('Ctrl Pts',(-8.28195044940169,1.18835118299697,14.3466414987109));
#29912=CARTESIAN_POINT('Ctrl Pts',(-8.86104085784046,1.15298466581975,14.36979541956));
#29913=CARTESIAN_POINT('Ctrl Pts',(-9.3568791758876,0.851752439724092,14.3929493404091));
#29914=CARTESIAN_POINT('Ctrl Pts',(-9.65513048665835,0.354115375885186,
14.4161032612581));
#29915=CARTESIAN_POINT('Ctrl Pts',(-9.68702128559088,-0.225176837618606,
14.4392571821072));
#29916=CARTESIAN_POINT('Ctrl Pts',(-9.4451979017152,-0.752545724350912,
14.4624111029563));
#29917=CARTESIAN_POINT('Ctrl Pts',(-8.98542217410244,-1.10638576162932,
14.4855650238054));
#29918=CARTESIAN_POINT('Ctrl Pts',(-8.41371337897523,-1.20510528987148,
14.5087189446545));
#29919=CARTESIAN_POINT('Ctrl Pts',(-7.86190133906803,-1.02594066084063,
14.5318728655036));
#29920=CARTESIAN_POINT('Ctrl Pts',(-7.45722790202316,-0.610205287031669,
14.5550267863527));
#29921=CARTESIAN_POINT('Ctrl Pts',(-7.29300635587047,-0.0537632186624639,
14.5781807072018));
#29922=CARTESIAN_POINT('Ctrl Pts',(-7.40710440092952,0.515076062525879,
14.6013346280508));
#29923=CARTESIAN_POINT('Ctrl Pts',(-7.77321227041997,0.965144412367029,
14.6244885488999));
#29924=CARTESIAN_POINT('Ctrl Pts',(-8.30690947628316,1.19266097046186,14.647642469749));
#29925=CARTESIAN_POINT('Ctrl Pts',(-8.88513125425981,1.14516289551101,14.6707963905981));
#29926=CARTESIAN_POINT('Ctrl Pts',(-9.37454595889494,0.833602727390392,
14.6939503114472));
#29927=CARTESIAN_POINT('Ctrl Pts',(-9.66229988816436,0.329822846063696,
14.7171042322963));
#29928=CARTESIAN_POINT('Ctrl Pts',(-9.68204012033543,-0.250010588840295,
14.7402581531454));
#29929=CARTESIAN_POINT('Ctrl Pts',(-9.4292147707369,-0.772194311373804,
14.7634120739945));
#29930=CARTESIAN_POINT('Ctrl Pts',(-8.96212261645511,-1.11631841902995,
14.7865659948435));
#29931=CARTESIAN_POINT('Ctrl Pts',(-8.38847001221673,-1.20303168797658,
14.8097199156926));
#29932=CARTESIAN_POINT('Ctrl Pts',(-7.84053502320186,-1.01233887812903,
14.8328738365417));
#29933=CARTESIAN_POINT('Ctrl Pts',(-7.44466544510217,-0.588211901328816,
14.8560277573908));
#29934=CARTESIAN_POINT('Ctrl Pts',(-7.29214459139059,-0.0284493284889608,
14.8791816782399));
#29935=CARTESIAN_POINT('Ctrl Pts',(-7.41814189141838,0.537872623636706,
14.902335599089));
#29936=CARTESIAN_POINT('Ctrl Pts',(-7.79360420188124,0.980168595469752,
14.9254895199381));
#29937=CARTESIAN_POINT('Ctrl Pts',(-8.33195295337524,1.19644497642632,14.9486434407871));
#29938=CARTESIAN_POINT('Ctrl Pts',(-8.9090528756146,1.13684175312818,14.9717973616362));
#29939=CARTESIAN_POINT('Ctrl Pts',(-9.39182575698232,0.815079698402111,
14.9949512824853));
#29940=CARTESIAN_POINT('Ctrl Pts',(-9.6689579814117,0.30540641673303,15.0181052033344));
#29941=CARTESIAN_POINT('Ctrl Pts',(-9.67651640217813,-0.274757341835666,
15.0412591241835));
#29942=CARTESIAN_POINT('Ctrl Pts',(-9.50068898914137,-0.619153746004177,
15.0566950714162));
#29943=CARTESIAN_POINT('Ctrl Pts',(-9.37767319112123,-0.761025107359488,
15.0644130450326));
#29944=CARTESIAN_POINT('Ctrl Pts',(-8.78594175781898,1.06827677035487,13.7355869549674));
#29945=CARTESIAN_POINT('Ctrl Pts',(-8.95862320832664,1.02205575453658,13.7433049285838));
#29946=CARTESIAN_POINT('Ctrl Pts',(-9.2809965740519,0.844336759477199,13.7587408758165));
#29947=CARTESIAN_POINT('Ctrl Pts',(-9.58457496737118,0.382891299209943,
13.7818947966656));
#29948=CARTESIAN_POINT('Ctrl Pts',(-9.63800682204146,-0.166805079312282,
13.8050487175147));
#29949=CARTESIAN_POINT('Ctrl Pts',(-9.42905025076876,-0.678064930363123,
13.8282026383638));
#29950=CARTESIAN_POINT('Ctrl Pts',(-9.00585346075692,-1.03296025147074,
13.8513565592128));
#29951=CARTESIAN_POINT('Ctrl Pts',(-8.46601748038542,-1.1496714409461,13.8745104800619));
#29952=CARTESIAN_POINT('Ctrl Pts',(-7.93401511063972,-1.00127863925212,
13.897664400911));
#29953=CARTESIAN_POINT('Ctrl Pts',(-7.5325237867556,-0.622002973815956,
13.9208183217601));
#29954=CARTESIAN_POINT('Ctrl Pts',(-7.35412143624022,-0.099299703795874,
13.9439722426092));
#29955=CARTESIAN_POINT('Ctrl Pts',(-7.4399464379323,0.446300767286306,13.9671261634583));
#29956=CARTESIAN_POINT('Ctrl Pts',(-7.7702081403358,0.888989246418001,13.9902800843074));
#29957=CARTESIAN_POINT('Ctrl Pts',(-8.26875194837151,1.1266864370002,14.0134340051564));
#29958=CARTESIAN_POINT('Ctrl Pts',(-8.82061901613093,1.10458202626637,14.0365879260055));
#29959=CARTESIAN_POINT('Ctrl Pts',(-9.2985548405924,0.827773017888108,14.0597418468546));
#29960=CARTESIAN_POINT('Ctrl Pts',(-9.59235260952549,0.360088570094568,
14.0828957677037));
#29961=CARTESIAN_POINT('Ctrl Pts',(-9.63426576373522,-0.190628383105298,
14.1060496885528));
#29962=CARTESIAN_POINT('Ctrl Pts',(-9.41462958297823,-0.697388505927078,
14.1292036094019));
#29963=CARTESIAN_POINT('Ctrl Pts',(-8.98408978039985,-1.04333843371576,
14.152357530251));
#29964=CARTESIAN_POINT('Ctrl Pts',(-8.44192414556558,-1.14870587953904,
14.1755114511001));
#29965=CARTESIAN_POINT('Ctrl Pts',(-7.913150170469,-0.989194258067005,14.1986653719492));
#29966=CARTESIAN_POINT('Ctrl Pts',(-7.51969737572152,-0.601585212120206,
14.2218192927982));
#29967=CARTESIAN_POINT('Ctrl Pts',(-7.35229169149517,-0.0752571670292948,
14.2449732136473));
#29968=CARTESIAN_POINT('Ctrl Pts',(-7.44953504563593,0.468424361302008,
14.2681271344964));
#29969=CARTESIAN_POINT('Ctrl Pts',(-7.78900417959064,0.904092332654155,
14.2912810553455));
#29970=CARTESIAN_POINT('Ctrl Pts',(-8.29242120759183,1.13128645689237,14.3144349761946));
#29971=CARTESIAN_POINT('Ctrl Pts',(-8.8437036447674,1.09761824291446,14.3375888970437));
#29972=CARTESIAN_POINT('Ctrl Pts',(-9.31573176409856,0.810851214246954,
14.3607428178928));
#29973=CARTESIAN_POINT('Ctrl Pts',(-9.59966102125167,0.337110725051789,
14.3838967387418));
#29974=CARTESIAN_POINT('Ctrl Pts',(-9.6300204212742,-0.214363826492215,
14.4070506595909));
#29975=CARTESIAN_POINT('Ctrl Pts',(-9.39980941710916,-0.716408413886026,
14.43020458044));
#29976=CARTESIAN_POINT('Ctrl Pts',(-8.96211215951534,-1.05325702211464,
14.4533585012891));
#29977=CARTESIAN_POINT('Ctrl Pts',(-8.41785686994467,-1.14723603011252,
14.4765124221382));
#29978=CARTESIAN_POINT('Ctrl Pts',(-7.89254289169556,-0.976674901990792,
14.4996663429873));
#29979=CARTESIAN_POINT('Ctrl Pts',(-7.50730190793318,-0.580903176619976,
14.5228202638364));
#29980=CARTESIAN_POINT('Ctrl Pts',(-7.35096629456346,-0.0511815042741817,
14.5459741846855));
#29981=CARTESIAN_POINT('Ctrl Pts',(-7.45958534167685,0.490342065663984,
14.5691281055345));
#29982=CARTESIAN_POINT('Ctrl Pts',(-7.80811267975863,0.918798094602432,
14.5922820263836));
#29983=CARTESIAN_POINT('Ctrl Pts',(-8.3161816998539,1.1353892879922,14.6154359472327));
#29984=CARTESIAN_POINT('Ctrl Pts',(-8.86663721827691,1.09017207468927,14.6385898680818));
#29985=CARTESIAN_POINT('Ctrl Pts',(-9.33255018666507,0.793573052661904,
14.6617437889309));
#29986=CARTESIAN_POINT('Ctrl Pts',(-9.6064861474802,0.313984724603508,14.68489770978));
#29987=CARTESIAN_POINT('Ctrl Pts',(-9.62527845200311,-0.238005058842469,
14.7080516306291));
#29988=CARTESIAN_POINT('Ctrl Pts',(-9.38459379745632,-0.735113474068666,
14.7312055514782));
#29989=CARTESIAN_POINT('Ctrl Pts',(-8.93993144863193,-1.06271271245186,
14.7543594723273));
#29990=CARTESIAN_POINT('Ctrl Pts',(-8.39382569183094,-1.14526200275911,
14.7775133931763));
#29991=CARTESIAN_POINT('Ctrl Pts',(-7.87220258815657,-0.963726278055894,
14.8006673140254));
#29992=CARTESIAN_POINT('Ctrl Pts',(-7.49534270127495,-0.559965915191835,
14.8238212348745));
#29993=CARTESIAN_POINT('Ctrl Pts',(-7.35014591208809,-0.0270831892859103,
14.8469751557236));
#29994=CARTESIAN_POINT('Ctrl Pts',(-7.47009281092229,0.512043933947867,
14.8701290765727));
#29995=CARTESIAN_POINT('Ctrl Pts',(-7.82752538891573,0.933100815139231,
14.8932829974218));
#29996=CARTESIAN_POINT('Ctrl Pts',(-8.34002258702019,1.1389915856645,14.9164369182709));
#29997=CARTESIAN_POINT('Ctrl Pts',(-8.889410121315,1.08225051427998,14.9395908391199));
#29998=CARTESIAN_POINT('Ctrl Pts',(-9.3490002073608,0.775939501120161,14.962744759969));
#29999=CARTESIAN_POINT('Ctrl Pts',(-9.61282451851665,0.290740774311144,
14.9858986808181));
#30000=CARTESIAN_POINT('Ctrl Pts',(-9.62001998326722,-0.261563470628722,
15.0090526016672));
#30001=CARTESIAN_POINT('Ctrl Pts',(-9.45263581774028,-0.589421929822312,
15.0244885488999));
#30002=CARTESIAN_POINT('Ctrl Pts',(-9.33552724893066,-0.724480616192598,
15.0322065225163));
#30003=CARTESIAN_POINT('Ctrl Pts',(-8.77151818897627,1.01439039972539,13.7033804324511));
#30004=CARTESIAN_POINT('Ctrl Pts',(-8.93548918457083,0.970500879693933,
13.7110984060675));
#30005=CARTESIAN_POINT('Ctrl Pts',(-9.24160128622238,0.80174644503821,13.7265343533002));
#30006=CARTESIAN_POINT('Ctrl Pts',(-9.52986647769036,0.363577369493793,
13.7496882741493));
#30007=CARTESIAN_POINT('Ctrl Pts',(-9.58060310505244,-0.158391042261083,
13.7728421949984));
#30008=CARTESIAN_POINT('Ctrl Pts',(-9.38218679034763,-0.64386175459224,
13.7959961158475));
#30009=CARTESIAN_POINT('Ctrl Pts',(-8.98033703296686,-0.980855328382519,
13.8191500366965));
#30010=CARTESIAN_POINT('Ctrl Pts',(-8.46773163789374,-1.09167933338734,
13.8423039575456));
#30011=CARTESIAN_POINT('Ctrl Pts',(-7.962564707865,-0.950771810539374,13.8654578783947));
#30012=CARTESIAN_POINT('Ctrl Pts',(-7.58132554230138,-0.59062769382316,
13.8886117992438));
#30013=CARTESIAN_POINT('Ctrl Pts',(-7.41192222223187,-0.0942907952521036,
13.9117657200929));
#30014=CARTESIAN_POINT('Ctrl Pts',(-7.49341801076609,0.423788316182253,
13.934919640942));
#30015=CARTESIAN_POINT('Ctrl Pts',(-7.8070205430048,0.844146556445263,13.9580735617911));
#30016=CARTESIAN_POINT('Ctrl Pts',(-8.28041663917374,1.06985374662238,13.9812274826402));
#30017=CARTESIAN_POINT('Ctrl Pts',(-8.80444624554045,1.04886433389506,14.0043814034893));
#30018=CARTESIAN_POINT('Ctrl Pts',(-9.25827387286731,0.78601821718774,14.0275353243383));
#30019=CARTESIAN_POINT('Ctrl Pts',(-9.53725179744342,0.341924863191994,
14.0506892451874));
#30020=CARTESIAN_POINT('Ctrl Pts',(-9.5770507544482,-0.181012643074652,
14.0738431660365));
#30021=CARTESIAN_POINT('Ctrl Pts',(-9.36849353465746,-0.662210603958245,
14.0969970868856));
#30022=CARTESIAN_POINT('Ctrl Pts',(-8.95967116338181,-0.990710010921813,
14.1201510077347));
#30023=CARTESIAN_POINT('Ctrl Pts',(-8.44485362704783,-1.09076247714853,
14.1433049285838));
#30024=CARTESIAN_POINT('Ctrl Pts',(-7.94275224391618,-0.93929699371196,
14.1664588494329));
#30025=CARTESIAN_POINT('Ctrl Pts',(-7.56914612534038,-0.57123985162458,
14.1896127702819));
#30026=CARTESIAN_POINT('Ctrl Pts',(-7.4101847740772,-0.0714610200872263,
14.212766691131));
#30027=CARTESIAN_POINT('Ctrl Pts',(-7.50252294674449,0.444795944541984,
14.2359206119801));
#30028=CARTESIAN_POINT('Ctrl Pts',(-7.8248684662229,0.858487807803833,14.2590745328292));
#30029=CARTESIAN_POINT('Ctrl Pts',(-8.30289196578197,1.07422173078777,14.2822284536783));
#30030=CARTESIAN_POINT('Ctrl Pts',(-8.82636643169434,1.04225182000917,14.3053823745274));
#30031=CARTESIAN_POINT('Ctrl Pts',(-9.27458435230953,0.769949988769815,
14.3285362953765));
#30032=CARTESIAN_POINT('Ctrl Pts',(-9.54419155584499,0.320106074218393,
14.3516902162256));
#30033=CARTESIAN_POINT('Ctrl Pts',(-9.57301955695752,-0.203550815365823,
14.3748441370746));
#30034=CARTESIAN_POINT('Ctrl Pts',(-9.35442093250312,-0.680271103421141,
14.3979980579237));
#30035=CARTESIAN_POINT('Ctrl Pts',(-8.93880214492824,-1.00012828259996,
14.4211519787728));
#30036=CARTESIAN_POINT('Ctrl Pts',(-8.42200036091411,-1.08936677035355,
14.4443058996219));
#30037=CARTESIAN_POINT('Ctrl Pts',(-7.9231844443231,-0.927409143140955,
14.467459820471));
#30038=CARTESIAN_POINT('Ctrl Pts',(-7.5573759138432,-0.551601066208283,
14.4906137413201));
#30039=CARTESIAN_POINT('Ctrl Pts',(-7.40892623325645,-0.0485997898858995,
14.5137676621692));
#30040=CARTESIAN_POINT('Ctrl Pts',(-7.51206628242418,0.465608068802088,
14.5369215830183));
#30041=CARTESIAN_POINT('Ctrl Pts',(-7.84301308909729,0.872451776837834,
14.5600755038673));
#30042=CARTESIAN_POINT('Ctrl Pts',(-8.32545392342464,1.07811760552253,14.5832294247164));
#30043=CARTESIAN_POINT('Ctrl Pts',(-8.84814318229402,1.03518125386753,14.6063833455655));
#30044=CARTESIAN_POINT('Ctrl Pts',(-9.29055441443522,0.753543377933415,
14.6295372664146));
#30045=CARTESIAN_POINT('Ctrl Pts',(-9.55067240679603,0.298146603143318,
14.6526911872637));
#30046=CARTESIAN_POINT('Ctrl Pts',(-9.56851678367079,-0.225999528844643,
14.6758451081128));
#30047=CARTESIAN_POINT('Ctrl Pts',(-9.33997282417574,-0.698032636763528,
14.6989990289619));
#30048=CARTESIAN_POINT('Ctrl Pts',(-8.91774028080876,-1.00910700587376,
14.722152949811));
#30049=CARTESIAN_POINT('Ctrl Pts',(-8.39918137144515,-1.08749231754164,
14.74530687066));
#30050=CARTESIAN_POINT('Ctrl Pts',(-7.90387015311128,-0.915113677982754,
14.7684607915091));
#30051=CARTESIAN_POINT('Ctrl Pts',(-7.54601995744774,-0.531719929054855,
14.7916147123582));
#30052=CARTESIAN_POINT('Ctrl Pts',(-7.40814723278559,-0.0257170500828612,
14.8147686332073));
#30053=CARTESIAN_POINT('Ctrl Pts',(-7.52204373042621,0.486215244259028,
14.8379225540564));
#30054=CARTESIAN_POINT('Ctrl Pts',(-7.86144657595021,0.886033034808711,
14.8610764749055));
#30055=CARTESIAN_POINT('Ctrl Pts',(-8.34809222066514,1.08153819490268,14.8842303957546));
#30056=CARTESIAN_POINT('Ctrl Pts',(-8.8697673670154,1.02765927543177,14.9073843166036));
#30057=CARTESIAN_POINT('Ctrl Pts',(-9.30617465773928,0.736799303838212,
14.9305382374527));
#30058=CARTESIAN_POINT('Ctrl Pts',(-9.5566910556216,0.276075131889258,14.9536921583018));
#30059=CARTESIAN_POINT('Ctrl Pts',(-9.56352356435632,-0.248369599421778,
14.9768460791509));
#30060=CARTESIAN_POINT('Ctrl Pts',(-9.40458264633919,-0.559690113640447,
14.9922820263836));
#30061=CARTESIAN_POINT('Ctrl Pts',(-9.29338130674009,-0.687936125025709,
15.));
#30062=CARTESIAN_POINT('Ctrl Pts',(-9.29338130674009,-0.687936125025709,
15.));
#30063=CARTESIAN_POINT('Ctrl Pts',(-9.3259020578849,-0.655901359921301,
15.));
#30064=CARTESIAN_POINT('Ctrl Pts',(-9.35618681437,-0.62180686309643,15.));
#30065=CARTESIAN_POINT('Ctrl Pts',(-9.38414512772406,-0.585952030068796,
15.));
#30066=CARTESIAN_POINT('Ctrl Pts',(-9.41250187315505,-0.54958623218394,
15.));
#30067=CARTESIAN_POINT('Ctrl Pts',(-9.43846612303508,-0.511408780275333,
15.));
#30068=CARTESIAN_POINT('Ctrl Pts',(-9.46191315816531,-0.471686815958835,
15.));
#30069=CARTESIAN_POINT('Ctrl Pts',(-9.48267465073316,-0.436514468480486,
15.));
#30070=CARTESIAN_POINT('Ctrl Pts',(-9.50146242253628,-0.400130092146184,
15.));
#30071=CARTESIAN_POINT('Ctrl Pts',(-9.51816342133453,-0.362697966110186,
15.));
#30072=CARTESIAN_POINT('Ctrl Pts',(-9.52289039443137,-0.352103351089404,
15.));
#30073=CARTESIAN_POINT('Ctrl Pts',(-9.5274513547165,-0.341420995627983,
15.));
#30074=CARTESIAN_POINT('Ctrl Pts',(-9.5318333519652,-0.330680180343462,
15.));
#30075=CARTESIAN_POINT('Ctrl Pts',(-9.5429335098473,-0.303472325414772,
15.));
#30076=CARTESIAN_POINT('Ctrl Pts',(-9.55289986461919,-0.27586001076394,
15.));
#30077=CARTESIAN_POINT('Ctrl Pts',(-9.56170500757217,-0.247911851598931,
15.));
#30078=CARTESIAN_POINT('Ctrl Pts',(-9.57582456759079,-0.203095349147118,
15.));
#30079=CARTESIAN_POINT('Ctrl Pts',(-9.58696093020466,-0.157416391299935,
15.));
#30080=CARTESIAN_POINT('Ctrl Pts',(-9.59514943628876,-0.111178475189023,
15.));
#30081=CARTESIAN_POINT('Ctrl Pts',(-9.60093612680025,-0.0785028555238702,
15.));
#30082=CARTESIAN_POINT('Ctrl Pts',(-9.60524968957201,-0.0455473510823616,
15.));
#30083=CARTESIAN_POINT('Ctrl Pts',(-9.60808795943142,-0.0124132764720893,
15.));
#30084=CARTESIAN_POINT('Ctrl Pts',(-9.60984655705952,0.00811666180204036,
15.));
#30085=CARTESIAN_POINT('Ctrl Pts',(-9.61103853842703,0.0287152310324904,
15.));
#30086=CARTESIAN_POINT('Ctrl Pts',(-9.61166096056637,0.0493586901403063,
15.));
#30087=CARTESIAN_POINT('Ctrl Pts',(-9.61202311273082,0.0613699489391692,
15.));
#30088=CARTESIAN_POINT('Ctrl Pts',(-9.61219223451897,0.0734008315968733,
15.));
#30089=CARTESIAN_POINT('Ctrl Pts',(-9.61216800780618,0.0854178244046445,
15.));
#30090=CARTESIAN_POINT('Ctrl Pts',(-9.61207054909412,0.133759531018345,
15.));
#30091=CARTESIAN_POINT('Ctrl Pts',(-9.60885285388807,0.181957620798743,
15.));
#30092=CARTESIAN_POINT('Ctrl Pts',(-9.60254715011237,0.22970110335093,15.));
#30093=CARTESIAN_POINT('Ctrl Pts',(-9.60007040651486,0.248453707174439,
15.));
#30094=CARTESIAN_POINT('Ctrl Pts',(-9.59711671912308,0.267136363796024,
15.));
#30095=CARTESIAN_POINT('Ctrl Pts',(-9.59368590857673,0.285730721169551,
15.));
#30096=CARTESIAN_POINT('Ctrl Pts',(-9.58524575907286,0.331474767376859,
15.));
#30097=CARTESIAN_POINT('Ctrl Pts',(-9.57392123707722,0.37668484759268,15.));
#30098=CARTESIAN_POINT('Ctrl Pts',(-9.55984249148786,0.421130972866353,
15.));
#30099=CARTESIAN_POINT('Ctrl Pts',(-9.55380224394171,0.440199830771102,
15.));
#30100=CARTESIAN_POINT('Ctrl Pts',(-9.54725445442082,0.459127999779685,
15.));
#30101=CARTESIAN_POINT('Ctrl Pts',(-9.54020690300201,0.47789673994602,15.));
#30102=CARTESIAN_POINT('Ctrl Pts',(-9.53575806190591,0.489744704950029,
15.));
#30103=CARTESIAN_POINT('Ctrl Pts',(-9.53110790593948,0.501533845979217,
15.));
#30104=CARTESIAN_POINT('Ctrl Pts',(-9.52627047416585,0.513230752196449,
15.));
#30105=CARTESIAN_POINT('Ctrl Pts',(-9.50753211141022,0.558540098575664,
15.));
#30106=CARTESIAN_POINT('Ctrl Pts',(-9.48596298565104,0.60253893451057,15.));
#30107=CARTESIAN_POINT('Ctrl Pts',(-9.46174303380365,0.644973322939031,
15.));
#30108=CARTESIAN_POINT('Ctrl Pts',(-9.43730206706482,0.687794938881859,
15.));
#30109=CARTESIAN_POINT('Ctrl Pts',(-9.410161349938,0.729024507609743,15.));
#30110=CARTESIAN_POINT('Ctrl Pts',(-9.38045491375756,0.768389355049031,
15.));
#30111=CARTESIAN_POINT('Ctrl Pts',(-9.37505712673739,0.77554211687035,15.));
#30112=CARTESIAN_POINT('Ctrl Pts',(-9.36957450216427,0.782633255724265,
15.));
#30113=CARTESIAN_POINT('Ctrl Pts',(-9.36400767903199,0.789661050510416,
15.));
#30114=CARTESIAN_POINT('Ctrl Pts',(-9.34883031194736,0.808821605593667,
15.));
#30115=CARTESIAN_POINT('Ctrl Pts',(-9.33302725419171,0.827511455077708,
15.));
#30116=CARTESIAN_POINT('Ctrl Pts',(-9.31662674801348,0.845709935759477,
15.));
#30117=CARTESIAN_POINT('Ctrl Pts',(-9.30887462895217,0.85431191349399,15.));
#30118=CARTESIAN_POINT('Ctrl Pts',(-9.30098899082769,0.862804079549591,
15.));
#30119=CARTESIAN_POINT('Ctrl Pts',(-9.29297263500711,0.87118408475251,15.));
#30120=CARTESIAN_POINT('Ctrl Pts',(-9.28554491584687,0.878948750718174,
15.));
#30121=CARTESIAN_POINT('Ctrl Pts',(-9.27801067856311,0.886611083762791,
15.));
#30122=CARTESIAN_POINT('Ctrl Pts',(-9.27037651112731,0.894165897788687,
15.));
#30123=CARTESIAN_POINT('Ctrl Pts',(-9.23471847327201,0.929453287905647,
15.));
#30124=CARTESIAN_POINT('Ctrl Pts',(-9.19685848483383,0.962423813168413,
15.));
#30125=CARTESIAN_POINT('Ctrl Pts',(-9.15706790102718,0.992921938496583,
15.));
#30126=CARTESIAN_POINT('Ctrl Pts',(-9.1348200881594,1.00997412824118,15.));
#30127=CARTESIAN_POINT('Ctrl Pts',(-9.11196791201093,1.02625290646587,15.));
#30128=CARTESIAN_POINT('Ctrl Pts',(-9.08855346078412,1.04172647599397,15.));
#30129=CARTESIAN_POINT('Ctrl Pts',(-9.07636608581335,1.0497805701151,15.));
#30130=CARTESIAN_POINT('Ctrl Pts',(-9.06402408681735,1.05761758254984,15.));
#30131=CARTESIAN_POINT('Ctrl Pts',(-9.05155350308553,1.06522083003624,15.));
#30132=CARTESIAN_POINT('Ctrl Pts',(-9.00599347684328,1.09299853174258,15.));
#30133=CARTESIAN_POINT('Ctrl Pts',(-8.95866634904485,1.11769704489194,15.));
#30134=CARTESIAN_POINT('Ctrl Pts',(-8.9098714082964,1.13911581419075,15.));
#30135=CARTESIAN_POINT('Ctrl Pts',(-8.87875621717539,1.15277397403451,15.));
#30136=CARTESIAN_POINT('Ctrl Pts',(-8.84704321113986,1.16509767556388,15.));
#30137=CARTESIAN_POINT('Ctrl Pts',(-8.81482207543407,1.17607856395778,15.));
#30138=CARTESIAN_POINT('Ctrl Pts',(-9.5500522825869,-1.91003407042144E-5,
14.0658930328476));
#30139=CARTESIAN_POINT('Ctrl Pts',(-9.55009297052377,-0.0583092030762354,
14.0685430772439));
#30140=CARTESIAN_POINT('Ctrl Pts',(-9.54531553472187,-0.116592705360584,
14.0711931216402));
#30141=CARTESIAN_POINT('Ctrl Pts',(-9.53565805831561,-0.174056052177473,
14.0738431660365));
#30142=CARTESIAN_POINT('Ctrl Pts',(-9.50753168118462,-0.34141196336918,
14.0815611396529));
#30143=CARTESIAN_POINT('Ctrl Pts',(-9.43801260792104,-0.501811283663713,
14.0892791132692));
#30144=CARTESIAN_POINT('Ctrl Pts',(-9.33511600940998,-0.636760844971574,
14.0969970868856));
#30145=CARTESIAN_POINT('Ctrl Pts',(-9.23221941089891,-0.771710406279434,
14.104715060502));
#30146=CARTESIAN_POINT('Ctrl Pts',(-9.09594528714036,-0.881210208600624,
14.1124330341183));
#30147=CARTESIAN_POINT('Ctrl Pts',(-8.94200530253875,-0.952635520799005,
14.1201510077347));
#30148=CARTESIAN_POINT('Ctrl Pts',(-8.78806531793715,-1.02406083299739,
14.127868981351));
#30149=CARTESIAN_POINT('Ctrl Pts',(-8.61645947249249,-1.05741165507296,
14.1355869549674));
#30150=CARTESIAN_POINT('Ctrl Pts',(-8.44697298591488,-1.04884281887132,
14.1433049285838));
#30151=CARTESIAN_POINT('Ctrl Pts',(-8.27748649933728,-1.04027398266968,
14.1510229022001));
#30152=CARTESIAN_POINT('Ctrl Pts',(-8.11011937162673,-0.989785488190817,
14.1587408758165));
#30153=CARTESIAN_POINT('Ctrl Pts',(-7.96416812134215,-0.903198383936824,
14.1664588494329));
#30154=CARTESIAN_POINT('Ctrl Pts',(-7.81821687105758,-0.816611279682832,
14.1741768230492));
#30155=CARTESIAN_POINT('Ctrl Pts',(-7.69368149819898,-0.693925565653706,
14.1818947966656));
#30156=CARTESIAN_POINT('Ctrl Pts',(-7.60492025322581,-0.549286236716252,
14.1896127702819));
#30157=CARTESIAN_POINT('Ctrl Pts',(-7.51615900825265,-0.404646907778796,
14.1973307438983));
#30158=CARTESIAN_POINT('Ctrl Pts',(-7.46317189116493,-0.238053963933011,
14.2050487175147));
#30159=CARTESIAN_POINT('Ctrl Pts',(-7.45206802806561,-0.0687146645719171,
14.212766691131));
#30160=CARTESIAN_POINT('Ctrl Pts',(-7.4409641649663,0.100624634789177,14.2204846647474));
#30161=CARTESIAN_POINT('Ctrl Pts',(-7.4717435558554,0.272710289665581,14.2282026383638));
#30162=CARTESIAN_POINT('Ctrl Pts',(-7.54085750454635,0.427701760980757,
14.2359206119801));
#30163=CARTESIAN_POINT('Ctrl Pts',(-7.6099714532373,0.582693232295935,14.2436385855965));
#30164=CARTESIAN_POINT('Ctrl Pts',(-7.7174199597301,0.720590520049885,14.2513565592128));
#30165=CARTESIAN_POINT('Ctrl Pts',(-7.85081479623634,0.825494817757516,
14.2590745328292));
#30166=CARTESIAN_POINT('Ctrl Pts',(-7.98420963274259,0.930399115465145,
14.2667925064456));
#30167=CARTESIAN_POINT('Ctrl Pts',(-8.14355079926228,1.00231042312646,14.2745104800619));
#30168=CARTESIAN_POINT('Ctrl Pts',(-8.31046712684085,1.03293775849401,14.2822284536783));
#30169=CARTESIAN_POINT('Ctrl Pts',(-8.47738345441942,1.06356509386157,14.2899464272947));
#30170=CARTESIAN_POINT('Ctrl Pts',(-8.65187494305688,1.05290845693537,14.297664400911));
#30171=CARTESIAN_POINT('Ctrl Pts',(-8.81382367414481,1.00219649993237,14.3053823745274));
#30172=CARTESIAN_POINT('Ctrl Pts',(-8.97577240523274,0.951484542929382,
14.3131003481437));
#30173=CARTESIAN_POINT('Ctrl Pts',(-9.12517837877114,0.860717265849599,
14.3208183217601));
#30174=CARTESIAN_POINT('Ctrl Pts',(-9.24481589946291,0.740359641551137,
14.3285362953765));
#30175=CARTESIAN_POINT('Ctrl Pts',(-9.36445342015469,0.620002017252674,
14.3362542689928));
#30176=CARTESIAN_POINT('Ctrl Pts',(-9.45432248799984,0.470054045735534,
14.3439722426092));
#30177=CARTESIAN_POINT('Ctrl Pts',(-9.5040616887745,0.307803911712927,14.3516902162256));
#30178=CARTESIAN_POINT('Ctrl Pts',(-9.53457214754885,0.208278266987425,
14.3564244884329));
#30179=CARTESIAN_POINT('Ctrl Pts',(-9.54998293159569,0.104123684619262,
14.3611587606403));
#30180=CARTESIAN_POINT('Ctrl Pts',(-9.55003832846065,-1.48519270705213E-5,
14.3658930328476));
#30181=CARTESIAN_POINT('Ctrl Pts',(-8.81478889550439,1.17604951161383,13.8));
#30182=CARTESIAN_POINT('Ctrl Pts',(-8.86280079884564,1.15963858656941,13.8));
#30183=CARTESIAN_POINT('Ctrl Pts',(-8.90960853485214,1.14022107018164,13.8));
#30184=CARTESIAN_POINT('Ctrl Pts',(-8.95497423007167,1.11798781340007,13.8));
#30185=CARTESIAN_POINT('Ctrl Pts',(-9.00031750369391,1.09576554521081,13.8));
#30186=CARTESIAN_POINT('Ctrl Pts',(-9.04422105970477,1.07072961904385,13.8));
#30187=CARTESIAN_POINT('Ctrl Pts',(-9.08642013951975,1.04302636820761,13.8));
#30188=CARTESIAN_POINT('Ctrl Pts',(-9.12519890659286,1.0175685166133,13.8));
#30189=CARTESIAN_POINT('Ctrl Pts',(-9.16253852722804,0.989857330873132,
13.8));
#30190=CARTESIAN_POINT('Ctrl Pts',(-9.1982035077309,0.959980834798695,13.8));
#30191=CARTESIAN_POINT('Ctrl Pts',(-9.20529926268142,0.954036732434542,
13.8));
#30192=CARTESIAN_POINT('Ctrl Pts',(-9.21233027103493,0.948005400253259,
13.8));
#30193=CARTESIAN_POINT('Ctrl Pts',(-9.21928917146909,0.941892145754135,
13.8));
#30194=CARTESIAN_POINT('Ctrl Pts',(-9.24730738764004,0.917278704638696,
13.8));
#30195=CARTESIAN_POINT('Ctrl Pts',(-9.27408805651624,0.891400484316834,
13.8));
#30196=CARTESIAN_POINT('Ctrl Pts',(-9.29952971553077,0.864321783055097,
13.8));
#30197=CARTESIAN_POINT('Ctrl Pts',(-9.33347410635491,0.828193242140612,
13.8));
#30198=CARTESIAN_POINT('Ctrl Pts',(-9.36503686827907,0.789928317341295,
13.8));
#30199=CARTESIAN_POINT('Ctrl Pts',(-9.394068236154,0.749793332929783,13.8));
#30200=CARTESIAN_POINT('Ctrl Pts',(-9.41426345293716,0.721874059050893,
13.8));
#30201=CARTESIAN_POINT('Ctrl Pts',(-9.43323285619316,0.693049121192648,
13.8));
#30202=CARTESIAN_POINT('Ctrl Pts',(-9.45091232284862,0.663402424323938,
13.8));
#30203=CARTESIAN_POINT('Ctrl Pts',(-9.4603430291963,0.647588073258055,13.8));
#30204=CARTESIAN_POINT('Ctrl Pts',(-9.46940649045895,0.631539836461061,
13.8));
#30205=CARTESIAN_POINT('Ctrl Pts',(-9.47809152424505,0.615270194622729,
13.8));
#30206=CARTESIAN_POINT('Ctrl Pts',(-9.48251143380655,0.606990394302504,
13.8));
#30207=CARTESIAN_POINT('Ctrl Pts',(-9.48683331758414,0.5986532504956,13.8));
#30208=CARTESIAN_POINT('Ctrl Pts',(-9.49105559547924,0.590260402670554,
13.8));
#30209=CARTESIAN_POINT('Ctrl Pts',(-9.49557755522519,0.581271861186176,
13.8));
#30210=CARTESIAN_POINT('Ctrl Pts',(-9.49998189717905,0.572225974771678,
13.8));
#30211=CARTESIAN_POINT('Ctrl Pts',(-9.50426389034573,0.563132325953286,
13.8));
#30212=CARTESIAN_POINT('Ctrl Pts',(-9.52493506409048,0.519233051157331,
13.8));
#30213=CARTESIAN_POINT('Ctrl Pts',(-9.54278546875511,0.474169441819486,
13.8));
#30214=CARTESIAN_POINT('Ctrl Pts',(-9.55766761541056,0.42818903643647,13.8));
#30215=CARTESIAN_POINT('Ctrl Pts',(-9.56297848681177,0.411780380775562,
13.8));
#30216=CARTESIAN_POINT('Ctrl Pts',(-9.56791089342669,0.395254820533891,
13.8));
#30217=CARTESIAN_POINT('Ctrl Pts',(-9.57245655696628,0.378623239143664,
13.8));
#30218=CARTESIAN_POINT('Ctrl Pts',(-9.58437734139714,0.335007715299727,
13.8));
#30219=CARTESIAN_POINT('Ctrl Pts',(-9.59364116996622,0.290662748326304,
13.8));
#30220=CARTESIAN_POINT('Ctrl Pts',(-9.60021783074656,0.245835590658758,
13.8));
#30221=CARTESIAN_POINT('Ctrl Pts',(-9.60298141730899,0.226998716643231,
13.8));
#30222=CARTESIAN_POINT('Ctrl Pts',(-9.60527003510969,0.208076747567834,
13.8));
#30223=CARTESIAN_POINT('Ctrl Pts',(-9.60707938280791,0.189088469737628,
13.8));
#30224=CARTESIAN_POINT('Ctrl Pts',(-9.60796926912187,0.179749519250995,
13.8));
#30225=CARTESIAN_POINT('Ctrl Pts',(-9.60874333971694,0.170392564265823,
13.8));
#30226=CARTESIAN_POINT('Ctrl Pts',(-9.60940054471547,0.161026142289271,
13.8));
#30227=CARTESIAN_POINT('Ctrl Pts',(-9.61273653439172,0.113481940576065,
13.8));
#30228=CARTESIAN_POINT('Ctrl Pts',(-9.61305375823859,0.065881512589885,
13.8));
#30229=CARTESIAN_POINT('Ctrl Pts',(-9.6103548789984,0.0185137348807834,
13.8));
#30230=CARTESIAN_POINT('Ctrl Pts',(-9.60768657879641,-0.0283173529821776,
13.8));
#30231=CARTESIAN_POINT('Ctrl Pts',(-9.60206995434507,-0.0749221057539117,
13.8));
#30232=CARTESIAN_POINT('Ctrl Pts',(-9.59345810572669,-0.121012288686138,
13.8));
#30233=CARTESIAN_POINT('Ctrl Pts',(-9.59107622215987,-0.133760010363862,
13.8));
#30234=CARTESIAN_POINT('Ctrl Pts',(-9.5884649252658,-0.146468262729219,
13.8));
#30235=CARTESIAN_POINT('Ctrl Pts',(-9.58562257062166,-0.159130656277011,
13.8));
#30236=CARTESIAN_POINT('Ctrl Pts',(-9.580683856266,-0.181132113737854,13.8));
#30237=CARTESIAN_POINT('Ctrl Pts',(-9.57504766985512,-0.202995218741589,
13.8));
#30238=CARTESIAN_POINT('Ctrl Pts',(-9.56872395555178,-0.224688164794557,
13.8));
#30239=CARTESIAN_POINT('Ctrl Pts',(-9.56551399339403,-0.235699657815915,
13.8));
#30240=CARTESIAN_POINT('Ctrl Pts',(-9.56212684590213,-0.246667280396052,
13.8));
#30241=CARTESIAN_POINT('Ctrl Pts',(-9.55856361622354,-0.257586691768621,
13.8));
#30242=CARTESIAN_POINT('Ctrl Pts',(-9.55533502617401,-0.267480609950803,
13.8));
#30243=CARTESIAN_POINT('Ctrl Pts',(-9.55196447513525,-0.27732683973438,
13.8));
#30244=CARTESIAN_POINT('Ctrl Pts',(-9.54845493647163,-0.287118339294702,
13.8));
#30245=CARTESIAN_POINT('Ctrl Pts',(-9.53268023941429,-0.331129234772824,
13.8));
#30246=CARTESIAN_POINT('Ctrl Pts',(-9.51409214385052,-0.374063802247248,
13.8));
#30247=CARTESIAN_POINT('Ctrl Pts',(-9.49280934665199,-0.415647420881541,
13.8));
#30248=CARTESIAN_POINT('Ctrl Pts',(-9.48095698558012,-0.438805282046661,
13.8));
#30249=CARTESIAN_POINT('Ctrl Pts',(-9.4682681093108,-0.461543689934097,
13.8));
#30250=CARTESIAN_POINT('Ctrl Pts',(-9.4547579204182,-0.483810537438775,
13.8));
#30251=CARTESIAN_POINT('Ctrl Pts',(-9.44902419320865,-0.49326059253597,
13.8));
#30252=CARTESIAN_POINT('Ctrl Pts',(-9.4431430707807,-0.502624468776889,
13.8));
#30253=CARTESIAN_POINT('Ctrl Pts',(-9.43712256581291,-0.51188805590247,
13.8));
#30254=CARTESIAN_POINT('Ctrl Pts',(-9.41182946395985,-0.550805863286665,
13.8));
#30255=CARTESIAN_POINT('Ctrl Pts',(-9.38404926471349,-0.588007002160364,
13.8));
#30256=CARTESIAN_POINT('Ctrl Pts',(-9.35388332257603,-0.623204245519968,
13.8));
#30257=CARTESIAN_POINT('Ctrl Pts',(-9.33467669468324,-0.645614298319899,
13.8));
#30258=CARTESIAN_POINT('Ctrl Pts',(-9.31450202461069,-0.667211228483348,
13.8));
#30259=CARTESIAN_POINT('Ctrl Pts',(-9.29341905289388,-0.68794083902027,
13.8));
#30260=CARTESIAN_POINT('Origin',(-8.5,0.,15.));
#30261=CARTESIAN_POINT('',(-7.46076951545867,-1.8,15.));
#30262=CARTESIAN_POINT('',(-6.42153903091735,0.,15.));
#30263=CARTESIAN_POINT('',(-7.46076951545867,-1.8,15.));
#30264=CARTESIAN_POINT('',(-7.46076951545867,1.8,15.));
#30265=CARTESIAN_POINT('',(-6.42153903091735,0.,15.));
#30266=CARTESIAN_POINT('',(-9.53923048454133,1.8,15.));
#30267=CARTESIAN_POINT('',(-7.46076951545867,1.8,15.));
#30268=CARTESIAN_POINT('',(-10.5784609690827,2.22044604925031E-16,15.));
#30269=CARTESIAN_POINT('',(-9.53923048454133,1.8,15.));
#30270=CARTESIAN_POINT('',(-9.53923048454133,-1.8,15.));
#30271=CARTESIAN_POINT('',(-10.5784609690827,2.54538057293978E-16,15.));
#30272=CARTESIAN_POINT('',(-9.53923048454133,-1.8,15.));
#30273=CARTESIAN_POINT('Origin',(-8.5,0.,13.7));
#30274=CARTESIAN_POINT('Origin',(-9.53923048454133,-1.8,13.8));
#30275=CARTESIAN_POINT('',(-9.53923048454133,-1.8,13.8));
#30276=CARTESIAN_POINT('',(-7.46076951545867,-1.8,13.8));
#30277=CARTESIAN_POINT('',(-9.53923048454133,-1.8,13.8));
#30278=CARTESIAN_POINT('',(-7.46076951545867,-1.8,13.8));
#30279=CARTESIAN_POINT('',(-9.53923048454133,-1.8,13.8));
#30280=CARTESIAN_POINT('Origin',(-10.5784609690827,2.54538057293978E-16,
13.8));
#30281=CARTESIAN_POINT('',(-10.5784609690827,2.54538057293978E-16,13.8));
#30282=CARTESIAN_POINT('',(-10.5784609690827,2.54538057293978E-16,13.8));
#30283=CARTESIAN_POINT('',(-10.5784609690827,2.54538057293978E-16,13.8));
#30284=CARTESIAN_POINT('Origin',(-9.53923048454133,1.8,13.8));
#30285=CARTESIAN_POINT('',(-9.53923048454133,1.8,13.8));
#30286=CARTESIAN_POINT('',(-9.53923048454133,1.8,13.8));
#30287=CARTESIAN_POINT('',(-9.53923048454133,1.8,13.8));
#30288=CARTESIAN_POINT('Origin',(-7.46076951545867,1.8,13.8));
#30289=CARTESIAN_POINT('',(-7.46076951545867,1.8,13.8));
#30290=CARTESIAN_POINT('',(-7.46076951545867,1.8,13.8));
#30291=CARTESIAN_POINT('',(-7.46076951545867,1.8,13.8));
#30292=CARTESIAN_POINT('Origin',(-6.42153903091735,0.,13.8));
#30293=CARTESIAN_POINT('',(-6.42153903091735,0.,13.8));
#30294=CARTESIAN_POINT('',(-6.42153903091735,0.,13.8));
#30295=CARTESIAN_POINT('',(-6.42153903091735,0.,13.8));
#30296=CARTESIAN_POINT('Origin',(-7.46076951545867,-1.8,13.8));
#30297=CARTESIAN_POINT('',(-7.46076951545867,-1.8,13.8));
#30298=CARTESIAN_POINT('Origin',(-8.5,0.,13.8));
#30299=CARTESIAN_POINT('',(0.,0.,0.));
#30300=CARTESIAN_POINT('',(0.,0.,0.));
#30301=CARTESIAN_POINT('',(0.,0.,0.));
#30302=CARTESIAN_POINT('Origin',(-8.5,0.,16.1));
#30303=CARTESIAN_POINT('',(-9.55012800649379,-2.18440497826711E-5,17.2841069671524));
#30304=CARTESIAN_POINT('',(-9.5500106216945,-1.13051919086155E-6,17.3658930328476));
#30305=CARTESIAN_POINT('',(-9.5501,-1.28600160378464E-16,16.1));
#30306=CARTESIAN_POINT('',(-9.29338130674014,-0.687936125025652,17.4));
#30307=CARTESIAN_POINT('Ctrl Pts',(-9.5500106216945,-1.13051919086155E-6,
17.3658930328476));
#30308=CARTESIAN_POINT('Ctrl Pts',(-9.55001831318254,-0.0803156021754179,
17.3695440482821));
#30309=CARTESIAN_POINT('Ctrl Pts',(-9.5409068063874,-0.160625002221925,
17.3731950637165));
#30310=CARTESIAN_POINT('Ctrl Pts',(-9.52264867059269,-0.238791324198228,
17.3768460791509));
#30311=CARTESIAN_POINT('Ctrl Pts',(-9.48405233681149,-0.404029083812233,
17.3845640527673));
#30312=CARTESIAN_POINT('Ctrl Pts',(-9.40458264633922,-0.55969011364039,
17.3922820263836));
#30313=CARTESIAN_POINT('Ctrl Pts',(-9.29338130674014,-0.687936125025652,
17.4));
#30314=CARTESIAN_POINT('',(-7.70661869325993,-0.687936125025728,17.4));
#30315=CARTESIAN_POINT('Origin',(-8.5,0.,17.4));
#30316=CARTESIAN_POINT('Ctrl Pts',(-7.70658083841847,-0.687941007616013,
17.4));
#30317=CARTESIAN_POINT('Ctrl Pts',(-7.79864150585798,-0.793915583878177,
17.3936166544345));
#30318=CARTESIAN_POINT('Ctrl Pts',(-7.91206827104569,-0.881430774697101,
17.387233308869));
#30319=CARTESIAN_POINT('Ctrl Pts',(-8.03812217198675,-0.943160594462135,
17.3808499633034));
#30320=CARTESIAN_POINT('Ctrl Pts',(-8.19053138620163,-1.01779686715008,
17.3731319896871));
#30321=CARTESIAN_POINT('Ctrl Pts',(-8.36139987870404,-1.05473818277663,
17.3654140160707));
#30322=CARTESIAN_POINT('Ctrl Pts',(-8.5310286260214,-1.04972425335905,17.3576960424544));
#30323=CARTESIAN_POINT('Ctrl Pts',(-8.70065737333876,-1.04471032394146,
17.349978068838));
#30324=CARTESIAN_POINT('Ctrl Pts',(-8.86904637547108,-0.99774114947973,
17.3422600952216));
#30325=CARTESIAN_POINT('Ctrl Pts',(-9.016780747997,-0.914232530587763,17.3345421216053));
#30326=CARTESIAN_POINT('Ctrl Pts',(-9.16451512052293,-0.830723911695799,
17.3268241479889));
#30327=CARTESIAN_POINT('Ctrl Pts',(-9.29159486344247,-0.7106758483736,17.3191061743725));
#30328=CARTESIAN_POINT('Ctrl Pts',(-9.38336862586148,-0.567928987999592,
17.3113882007562));
#30329=CARTESIAN_POINT('Ctrl Pts',(-9.47514238828048,-0.425182127625583,
17.3036702271398));
#30330=CARTESIAN_POINT('Ctrl Pts',(-9.53161017019895,-0.259736470199762,
17.2959522535235));
#30331=CARTESIAN_POINT('Ctrl Pts',(-9.5462614276818,-0.0906671084845678,
17.2882342799071));
#30332=CARTESIAN_POINT('Ctrl Pts',(-9.5488730942879,-0.0605295720566002,
17.2868585089888));
#30333=CARTESIAN_POINT('Ctrl Pts',(-9.5501560404896,-0.0302768923953349,
17.2854827380706));
#30334=CARTESIAN_POINT('Ctrl Pts',(-9.55012800649379,-2.18440497826711E-5,
17.2841069671524));
#30335=CARTESIAN_POINT('Origin',(-8.5,0.,16.1));
#30336=CARTESIAN_POINT('',(-9.55014795915375,-1.85392213186142E-5,16.9841069671524));
#30337=CARTESIAN_POINT('',(-9.55002861856303,-9.63118433582547E-6,17.0658930328476));
#30338=CARTESIAN_POINT('',(-9.5501,-1.28600160378464E-16,16.1));
#30339=CARTESIAN_POINT('Ctrl Pts',(-9.55002861856303,-9.63118433582547E-6,
17.0658930328476));
#30340=CARTESIAN_POINT('Ctrl Pts',(-9.5500534563119,-0.0729826763478919,
17.0692103912693));
#30341=CARTESIAN_POINT('Ctrl Pts',(-9.54254615138756,-0.145950682283606,
17.0725277496911));
#30342=CARTESIAN_POINT('Ctrl Pts',(-9.5274522464353,-0.217314064080866,
17.0758451081128));
#30343=CARTESIAN_POINT('Ctrl Pts',(-9.49233564298756,-0.38334396735565,
17.0835630817291));
#30344=CARTESIAN_POINT('Ctrl Pts',(-9.41615430938654,-0.540688365002029,
17.0912810553455));
#30345=CARTESIAN_POINT('Ctrl Pts',(-9.30769153933757,-0.6712063014371,17.0989990289619));
#30346=CARTESIAN_POINT('Ctrl Pts',(-9.1992287692886,-0.801724237872172,
17.1067170025782));
#30347=CARTESIAN_POINT('Ctrl Pts',(-9.05848456279167,-0.905415713095935,
17.1144349761946));
#30348=CARTESIAN_POINT('Ctrl Pts',(-8.90168595900391,-0.970325671537641,
17.122152949811));
#30349=CARTESIAN_POINT('Ctrl Pts',(-8.74488735521615,-1.03523562997935,
17.1298709234273));
#30350=CARTESIAN_POINT('Ctrl Pts',(-8.57203435413756,-1.061364071639,17.1375888970437));
#30351=CARTESIAN_POINT('Ctrl Pts',(-8.40305596905745,-1.04569851429791,
17.14530687066));
#30352=CARTESIAN_POINT('Ctrl Pts',(-8.23407758397734,-1.03003295695682,
17.1530248442764));
#30353=CARTESIAN_POINT('Ctrl Pts',(-8.06897381489572,-0.972573400614992,
17.1607428178928));
#30354=CARTESIAN_POINT('Ctrl Pts',(-7.92678022008012,-0.879944652158432,
17.1684607915091));
#30355=CARTESIAN_POINT('Ctrl Pts',(-7.78458662526451,-0.787315903701873,
17.1761787651255));
#30356=CARTESIAN_POINT('Ctrl Pts',(-7.66530320471492,-0.659517963130584,
17.1838967387419));
#30357=CARTESIAN_POINT('Ctrl Pts',(-7.58268270323884,-0.511285165544643,
17.1916147123582));
#30358=CARTESIAN_POINT('Ctrl Pts',(-7.50006220176276,-0.363052367958701,
17.1993326859746));
#30359=CARTESIAN_POINT('Ctrl Pts',(-7.45410461936019,-0.194384713358108,
17.2070506595909));
#30360=CARTESIAN_POINT('Ctrl Pts',(-7.45010857988296,-0.0247288190203272,
17.2147686332073));
#30361=CARTESIAN_POINT('Ctrl Pts',(-7.44611254040573,0.144927075317456,
17.2224866068237));
#30362=CARTESIAN_POINT('Ctrl Pts',(-7.48407804385384,0.315571209392425,
17.23020458044));
#30363=CARTESIAN_POINT('Ctrl Pts',(-7.55962794825812,0.467529582998103,
17.2379225540564));
#30364=CARTESIAN_POINT('Ctrl Pts',(-7.6351778526624,0.619487956603781,17.2456405276728));
#30365=CARTESIAN_POINT('Ctrl Pts',(-7.74831215802285,0.752760569740168,
17.2533585012891));
#30366=CARTESIAN_POINT('Ctrl Pts',(-7.88598692485404,0.851981087282268,
17.2610764749055));
#30367=CARTESIAN_POINT('Ctrl Pts',(-8.02366169168523,0.951201604824368,
17.2687944485218));
#30368=CARTESIAN_POINT('Ctrl Pts',(-8.18587691998715,1.01637002677218,17.2765124221382));
#30369=CARTESIAN_POINT('Ctrl Pts',(-8.35393041166614,1.03997440538661,17.2842303957546));
#30370=CARTESIAN_POINT('Ctrl Pts',(-8.52198390334514,1.06357878400103,17.2919483693709));
#30371=CARTESIAN_POINT('Ctrl Pts',(-8.6958756584012,1.04561911928206,17.2996663429873));
#30372=CARTESIAN_POINT('Ctrl Pts',(-8.85555604832858,0.988162672768926,
17.3073843166036));
#30373=CARTESIAN_POINT('Ctrl Pts',(-9.01523643825595,0.930706226255792,
17.31510229022));
#30374=CARTESIAN_POINT('Ctrl Pts',(-9.16070546305465,0.833752997948491,
17.3228202638364));
#30375=CARTESIAN_POINT('Ctrl Pts',(-9.2751927205708,0.708488991223898,17.3305382374527));
#30376=CARTESIAN_POINT('Ctrl Pts',(-9.38967997808695,0.5832249844993,17.3382562110691));
#30377=CARTESIAN_POINT('Ctrl Pts',(-9.47318546832054,0.429650199357407,
17.3459741846855));
#30378=CARTESIAN_POINT('Ctrl Pts',(-9.51607672489228,0.265455562086529,
17.3536921583018));
#30379=CARTESIAN_POINT('Ctrl Pts',(-9.53867811685325,0.178933793981138,
17.3577591164838));
#30380=CARTESIAN_POINT('Ctrl Pts',(-9.55000205395197,0.0894631852297447,
17.3618260746657));
#30381=CARTESIAN_POINT('Ctrl Pts',(-9.5500106216945,-1.13051919086155E-6,
17.3658930328476));
#30382=CARTESIAN_POINT('Ctrl Pts',(-9.55012800649379,-2.18440497826711E-5,
17.2841069671524));
#30383=CARTESIAN_POINT('Ctrl Pts',(-9.54999877183601,0.139451702530489,
17.2777647644542));
#30384=CARTESIAN_POINT('Ctrl Pts',(-9.52200934434521,0.278975587019088,
17.2714225617561));
#30385=CARTESIAN_POINT('Ctrl Pts',(-9.46789768755617,0.407501569956399,
17.265080359058));
#30386=CARTESIAN_POINT('Ctrl Pts',(-9.40204795690043,0.563907820677612,
17.2573623854416));
#30387=CARTESIAN_POINT('Ctrl Pts',(-9.29751376254171,0.704027256115468,
17.2496444118253));
#30388=CARTESIAN_POINT('Ctrl Pts',(-9.16634730336329,0.811704845033145,
17.2419264382089));
#30389=CARTESIAN_POINT('Ctrl Pts',(-9.03518084418487,0.919382433950822,
17.2342084645926));
#30390=CARTESIAN_POINT('Ctrl Pts',(-8.87738212018675,0.994618176348321,
17.2264904909762));
#30391=CARTESIAN_POINT('Ctrl Pts',(-8.7111444764068,1.02873781147201,17.2187725173598));
#30392=CARTESIAN_POINT('Ctrl Pts',(-8.54490683262685,1.0628574465957,17.2110545437435));
#30393=CARTESIAN_POINT('Ctrl Pts',(-8.37023026906508,1.05586097444558,17.2033365701271));
#30394=CARTESIAN_POINT('Ctrl Pts',(-8.20725403725456,1.00855504524276,17.1956185965107));
#30395=CARTESIAN_POINT('Ctrl Pts',(-8.04427780544405,0.961249116039934,
17.1879006228944));
#30396=CARTESIAN_POINT('Ctrl Pts',(-7.8930019053848,0.873633729784408,17.180182649278));
#30397=CARTESIAN_POINT('Ctrl Pts',(-7.77086762711664,0.755810465752038,
17.1724646756617));
#30398=CARTESIAN_POINT('Ctrl Pts',(-7.64873334884848,0.637987201719667,
17.1647467020453));
#30399=CARTESIAN_POINT('Ctrl Pts',(-7.55574069237142,0.489956059910451,
17.1570287284289));
#30400=CARTESIAN_POINT('Ctrl Pts',(-7.50261120356912,0.328784223964852,
17.1493107548126));
#30401=CARTESIAN_POINT('Ctrl Pts',(-7.44948171476683,0.167612388019253,
17.1415927811962));
#30402=CARTESIAN_POINT('Ctrl Pts',(-7.4362153936393,-0.00670014206272976,
17.1338748075798));
#30403=CARTESIAN_POINT('Ctrl Pts',(-7.46434177529062,-0.17405608013945,
17.1261568339635));
#30404=CARTESIAN_POINT('Ctrl Pts',(-7.49246815694194,-0.341412018216172,
17.1184388603471));
#30405=CARTESIAN_POINT('Ctrl Pts',(-7.56198724137211,-0.501811364287633,
17.1107208867308));
#30406=CARTESIAN_POINT('Ctrl Pts',(-7.66488385641448,-0.636760947278931,
17.1030029131144));
#30407=CARTESIAN_POINT('Ctrl Pts',(-7.76778047145686,-0.771710530270227,
17.095284939498));
#30408=CARTESIAN_POINT('Ctrl Pts',(-7.90405461711142,-0.881210350181365,
17.0875669658817));
#30409=CARTESIAN_POINT('Ctrl Pts',(-8.05799462644632,-0.952635673854597,
17.0798489922653));
#30410=CARTESIAN_POINT('Ctrl Pts',(-8.21193463578122,-1.02406099752783,
17.0721310186489));
#30411=CARTESIAN_POINT('Ctrl Pts',(-8.38354050879644,-1.05741182496316,
17.0644130450326));
#30412=CARTESIAN_POINT('Ctrl Pts',(-8.5530270226046,-1.04884298738516,17.0566950714162));
#30413=CARTESIAN_POINT('Ctrl Pts',(-8.72251353641277,-1.04027414980716,
17.0489770977999));
#30414=CARTESIAN_POINT('Ctrl Pts',(-8.88988069101389,-0.989785647215842,
17.0412591241835));
#30415=CARTESIAN_POINT('Ctrl Pts',(-9.03583196474797,-0.903198529050057,
17.0335411505671));
#30416=CARTESIAN_POINT('Ctrl Pts',(-9.18178323848206,-0.816611410884273,
17.0258231769508));
#30417=CARTESIAN_POINT('Ctrl Pts',(-9.3063186313491,-0.693925677144025,
17.0181052033344));
#30418=CARTESIAN_POINT('Ctrl Pts',(-9.39507989058315,-0.549286324968012,
17.010387229718));
#30419=CARTESIAN_POINT('Ctrl Pts',(-9.48384114981719,-0.404646972791997,
17.0026692561017));
#30420=CARTESIAN_POINT('Ctrl Pts',(-9.53682827541823,-0.238054002180217,
16.9949512824853));
#30421=CARTESIAN_POINT('Ctrl Pts',(-9.54793214030158,-0.0687146756119928,
16.987233308869));
#30422=CARTESIAN_POINT('Ctrl Pts',(-9.54943143177046,-0.0458497533225895,
16.9861911949634));
#30423=CARTESIAN_POINT('Ctrl Pts',(-9.55016712610837,-0.0229347606830505,
16.9851490810579));
#30424=CARTESIAN_POINT('Ctrl Pts',(-9.55014795915375,-1.85392213186142E-5,
16.9841069671524));
#30425=CARTESIAN_POINT('Origin',(-8.5,0.,16.1));
#30426=CARTESIAN_POINT('',(-9.55016499124735,-1.36965953006496E-5,16.6841069671524));
#30427=CARTESIAN_POINT('',(-9.55003851802847,-1.48519297202892E-5,16.7658930328476));
#30428=CARTESIAN_POINT('',(-9.5501,-1.28600160378464E-16,16.1));
#30429=CARTESIAN_POINT('Ctrl Pts',(-9.55003851802847,-1.48519297202892E-5,
16.7658930328476));
#30430=CARTESIAN_POINT('Ctrl Pts',(-9.55007343104712,-0.065646556384278,
16.7688767342566));
#30431=CARTESIAN_POINT('Ctrl Pts',(-9.54400925298908,-0.131271887510206,
16.7718604356656));
#30432=CARTESIAN_POINT('Ctrl Pts',(-9.53178197230159,-0.195728083779944,
16.7748441370746));
#30433=CARTESIAN_POINT('Ctrl Pts',(-9.50015352936794,-0.362457643486915,
16.782562110691));
#30434=CARTESIAN_POINT('Ctrl Pts',(-9.42728730806163,-0.521364434860128,
16.7902800843074));
#30435=CARTESIAN_POINT('Ctrl Pts',(-9.32158438697376,-0.654127370034059,
16.7979980579237));
#30436=CARTESIAN_POINT('Ctrl Pts',(-9.21588146588589,-0.786890305207989,
16.8057160315401));
#30437=CARTESIAN_POINT('Ctrl Pts',(-9.07734184501646,-0.893509384182638,
16.8134340051565));
#30438=CARTESIAN_POINT('Ctrl Pts',(-8.92193838836266,-0.961692007647338,
16.8211519787728));
#30439=CARTESIAN_POINT('Ctrl Pts',(-8.76653493170886,-1.02987463111204,
16.8288699523892));
#30440=CARTESIAN_POINT('Ctrl Pts',(-8.59426763927069,-1.05962079906679,
16.8365879260055));
#30441=CARTESIAN_POINT('Ctrl Pts',(-8.42499799194421,-1.04750094030223,
16.8443058996219));
#30442=CARTESIAN_POINT('Ctrl Pts',(-8.25572834461773,-1.03538108153767,
16.8520238732383));
#30443=CARTESIAN_POINT('Ctrl Pts',(-8.08945634240295,-0.9813951960538,16.8597418468546));
#30444=CARTESIAN_POINT('Ctrl Pts',(-7.94535224187542,-0.89176756251543,
16.867459820471));
#30445=CARTESIAN_POINT('Ctrl Pts',(-7.8012481413479,-0.802139928977061,
16.8751777940874));
#30446=CARTESIAN_POINT('Ctrl Pts',(-7.67931194250762,-0.676870547384194,
16.8828957677037));
#30447=CARTESIAN_POINT('Ctrl Pts',(-7.59360222518964,-0.530402295399115,
16.8906137413201));
#30448=CARTESIAN_POINT('Ctrl Pts',(-7.50789250787166,-0.383934043414033,
16.8983317149364));
#30449=CARTESIAN_POINT('Ctrl Pts',(-7.45840927207598,-0.216266921036739,
16.9060496885528));
#30450=CARTESIAN_POINT('Ctrl Pts',(-7.45085766547616,-0.0467320345949428,
16.9137676621692));
#30451=CARTESIAN_POINT('Ctrl Pts',(-7.44330605887635,0.122802851846853,
16.9214856357855));
#30452=CARTESIAN_POINT('Ctrl Pts',(-7.4776860814724,0.294205502353147,16.9292036094019));
#30453=CARTESIAN_POINT('Ctrl Pts',(-7.55003390384043,0.447714124520869,
16.9369215830182));
#30454=CARTESIAN_POINT('Ctrl Pts',(-7.62238172620845,0.60122274668859,16.9446395566346));
#30455=CARTESIAN_POINT('Ctrl Pts',(-7.73269734834845,0.736837340517737,
16.952357530251));
#30456=CARTESIAN_POINT('Ctrl Pts',(-7.86826197965597,0.838922281733849,
16.9600755038673));
#30457=CARTESIAN_POINT('Ctrl Pts',(-8.0038266109635,0.941007222949962,16.9677934774837));
#30458=CARTESIAN_POINT('Ctrl Pts',(-8.16464025143855,1.00956251155304,16.9755114511001));
#30459=CARTESIAN_POINT('Ctrl Pts',(-8.33216196388124,1.0366840959553,16.9832294247164));
#30460=CARTESIAN_POINT('Ctrl Pts',(-8.49968367632392,1.06380568035755,16.9909473983328));
#30461=CARTESIAN_POINT('Ctrl Pts',(-8.67391346073423,1.04949356055899,16.9986653719492));
#30462=CARTESIAN_POINT('Ctrl Pts',(-8.83476357160864,0.995397846192756,
17.0063833455655));
#30463=CARTESIAN_POINT('Ctrl Pts',(-8.99561368248304,0.941302131826525,
17.0141013191819));
#30464=CARTESIAN_POINT('Ctrl Pts',(-9.14308411982153,0.84742282289263,17.0218192927982));
#30465=CARTESIAN_POINT('Ctrl Pts',(-9.26017234504276,0.724583692265943,
17.0295372664146));
#30466=CARTESIAN_POINT('Ctrl Pts',(-9.37726057026399,0.601744561639255,
17.037255240031));
#30467=CARTESIAN_POINT('Ctrl Pts',(-9.46396658336796,0.449945609319775,
17.0449732136473));
#30468=CARTESIAN_POINT('Ctrl Pts',(-9.51029365327272,0.286688428708442,
17.0526911872637));
#30469=CARTESIAN_POINT('Ctrl Pts',(-9.53670830793207,0.193602851412619,
17.0570918024583));
#30470=CARTESIAN_POINT('Ctrl Pts',(-9.54999567024658,0.0967921763152249,
17.061492417653));
#30471=CARTESIAN_POINT('Ctrl Pts',(-9.55002861856303,-9.63118433582547E-6,
17.0658930328476));
#30472=CARTESIAN_POINT('Ctrl Pts',(-9.55014795915375,-1.85392213186142E-5,
16.9841069671524));
#30473=CARTESIAN_POINT('Ctrl Pts',(-9.55002517420727,0.146784491396649,
16.9774311074415));
#30474=CARTESIAN_POINT('Ctrl Pts',(-9.51892454602037,0.293637950168291,
16.9707552477307));
#30475=CARTESIAN_POINT('Ctrl Pts',(-9.45914264955535,0.427701829697936,
16.9640793880199));
#30476=CARTESIAN_POINT('Ctrl Pts',(-9.39002868976012,0.58269332591497,16.9563614144035));
#30477=CARTESIAN_POINT('Ctrl Pts',(-9.28258016600401,0.720590635824375,
16.9486434407871));
#30478=CARTESIAN_POINT('Ctrl Pts',(-9.14918530806574,0.82549495038658,16.9409254671708));
#30479=CARTESIAN_POINT('Ctrl Pts',(-9.01579045012747,0.930399264948787,
16.9332074935544));
#30480=CARTESIAN_POINT('Ctrl Pts',(-8.85644925800704,1.00231058416379,16.9254895199381));
#30481=CARTESIAN_POINT('Ctrl Pts',(-8.68953290361066,1.03293792445212,16.9177715463217));
#30482=CARTESIAN_POINT('Ctrl Pts',(-8.52261654921428,1.06356526474045,16.9100535727053));
#30483=CARTESIAN_POINT('Ctrl Pts',(-8.34812503254195,1.05290862610209,16.902335599089));
#30484=CARTESIAN_POINT('Ctrl Pts',(-8.18617627543435,1.00219666095141,16.8946176254726));
#30485=CARTESIAN_POINT('Ctrl Pts',(-8.02422751832675,0.951484695800729,
16.8868996518562));
#30486=CARTESIAN_POINT('Ctrl Pts',(-7.87482152078387,0.860717404137714,
16.8791816782399));
#30487=CARTESIAN_POINT('Ctrl Pts',(-7.7551839808704,0.740359760501857,16.8714637046235));
#30488=CARTESIAN_POINT('Ctrl Pts',(-7.63554644095693,0.620002116866001,
16.8637457310072));
#30489=CARTESIAN_POINT('Ctrl Pts',(-7.54567735867286,0.470054121257305,
16.8560277573908));
#30490=CARTESIAN_POINT('Ctrl Pts',(-7.49593814990679,0.3078039611666,16.8483097837744));
#30491=CARTESIAN_POINT('Ctrl Pts',(-7.44619894114072,0.145553801075895,
16.8405918101581));
#30492=CARTESIAN_POINT('Ctrl Pts',(-7.43658960589264,-0.0289985234968166,
16.8328738365417));
#30493=CARTESIAN_POINT('Ctrl Pts',(-7.4682180481979,-0.195728079891194,
16.8251558629253));
#30494=CARTESIAN_POINT('Ctrl Pts',(-7.49984649050317,-0.362457636285574,
16.817437889309));
#30495=CARTESIAN_POINT('Ctrl Pts',(-7.57271271036177,-0.521364424501619,
16.8097199156926));
#30496=CARTESIAN_POINT('Ctrl Pts',(-7.67841562934952,-0.65412735703781,
16.8020019420763));
#30497=CARTESIAN_POINT('Ctrl Pts',(-7.78411854833728,-0.786890289574002,
16.7942839684599));
#30498=CARTESIAN_POINT('Ctrl Pts',(-7.92265816645419,-0.893509366430338,
16.7865659948435));
#30499=CARTESIAN_POINT('Ctrl Pts',(-8.07806162002042,-0.961691988540383,
16.7788480212272));
#30500=CARTESIAN_POINT('Ctrl Pts',(-8.23346507358666,-1.02987461065043,
16.7711300476108));
#30501=CARTESIAN_POINT('Ctrl Pts',(-8.40573236260221,-1.05962077801418,
16.7634120739944));
#30502=CARTESIAN_POINT('Ctrl Pts',(-8.57500200656563,-1.04750091949042,
16.7556941003781));
#30503=CARTESIAN_POINT('Ctrl Pts',(-8.74427165052905,-1.03538106096666,
16.7479761267617));
#30504=CARTESIAN_POINT('Ctrl Pts',(-8.91054364944032,-0.981395176555395,
16.7402581531454));
#30505=CARTESIAN_POINT('Ctrl Pts',(-9.05464774710478,-0.891767544797753,
16.732540179529));
#30506=CARTESIAN_POINT('Ctrl Pts',(-9.19875184476925,-0.80213991304011,
16.7248222059126));
#30507=CARTESIAN_POINT('Ctrl Pts',(-9.32068804118689,-0.676870533936093,
16.7171042322963));
#30508=CARTESIAN_POINT('Ctrl Pts',(-9.40639775680199,-0.530402284861058,
16.7093862586799));
#30509=CARTESIAN_POINT('Ctrl Pts',(-9.49210747241709,-0.383934035786023,
16.7016682850636));
#30510=CARTESIAN_POINT('Ctrl Pts',(-9.54159070722963,-0.216266916739969,
16.6939503114472));
#30511=CARTESIAN_POINT('Ctrl Pts',(-9.54914231367942,-0.0467320336664906,
16.6862323378308));
#30512=CARTESIAN_POINT('Ctrl Pts',(-9.54983549921064,-0.0311698974819526,
16.685523880938));
#30513=CARTESIAN_POINT('Ctrl Pts',(-9.5501753697963,-0.0155920235602596,
16.6848154240452));
#30514=CARTESIAN_POINT('Ctrl Pts',(-9.55016499124735,-1.36965953006496E-5,
16.6841069671524));
#30515=CARTESIAN_POINT('Origin',(-8.5,0.,16.1));
#30516=CARTESIAN_POINT('',(-9.55017719779692,-7.61530804432864E-6,16.3841069671524));
#30517=CARTESIAN_POINT('',(-9.55005247215833,-1.9100347204657E-5,16.4658930328476));
#30518=CARTESIAN_POINT('',(-9.5501,-1.28600160378464E-16,16.1));
#30519=CARTESIAN_POINT('',(-7.70661869325986,-0.687936125025652,16.2));
#30520=CARTESIAN_POINT('Ctrl Pts',(-9.55017719779692,-7.61530804432864E-6,
16.3841069671524));
#30521=CARTESIAN_POINT('Ctrl Pts',(-9.55011144655369,0.161456631165944,
16.3767637934161));
#30522=CARTESIAN_POINT('Ctrl Pts',(-9.51225308460155,0.322950597851874,
16.3694206196799));
#30523=CARTESIAN_POINT('Ctrl Pts',(-9.44037203261531,0.467529573139717,
16.3620774459436));
#30524=CARTESIAN_POINT('Ctrl Pts',(-9.36482212971608,0.619487943842984,
16.3543594723272));
#30525=CARTESIAN_POINT('Ctrl Pts',(-9.25168782689266,0.75276055510798,16.3466414987109));
#30526=CARTESIAN_POINT('Ctrl Pts',(-9.11401306207929,0.851981069812583,
16.3389235250945));
#30527=CARTESIAN_POINT('Ctrl Pts',(-8.97633829726593,0.951201584517186,
16.3312055514782));
#30528=CARTESIAN_POINT('Ctrl Pts',(-8.81412307046263,1.01637000266139,16.3234875778618));
#30529=CARTESIAN_POINT('Ctrl Pts',(-8.64606958159429,1.03997438059275,16.3157696042454));
#30530=CARTESIAN_POINT('Ctrl Pts',(-8.47801609272595,1.06357875852411,16.3080516306291));
#30531=CARTESIAN_POINT('Ctrl Pts',(-8.30412434179258,1.04561909624262,16.3003336570127));
#30532=CARTESIAN_POINT('Ctrl Pts',(-8.14444395006926,0.988162645854508,
16.2926156833963));
#30533=CARTESIAN_POINT('Ctrl Pts',(-7.98476355834595,0.930706195466399,
16.28489770978));
#30534=CARTESIAN_POINT('Ctrl Pts',(-7.8392945258327,0.833752956971675,16.2771797361636));
#30535=CARTESIAN_POINT('Ctrl Pts',(-7.72480726549775,0.708488948192354,
16.2694617625473));
#30536=CARTESIAN_POINT('Ctrl Pts',(-7.6103200051628,0.583224939413033,16.2617437889309));
#30537=CARTESIAN_POINT('Ctrl Pts',(-7.52681451700616,0.429650160349115,
16.2540258153145));
#30538=CARTESIAN_POINT('Ctrl Pts',(-7.48392323634831,0.26545550415572,16.2463078416982));
#30539=CARTESIAN_POINT('Ctrl Pts',(-7.44103195569046,0.101260847962323,
16.2385898680818));
#30540=CARTESIAN_POINT('Ctrl Pts',(-7.4387548825314,-0.0735536853605511,
16.2308718944654));
#30541=CARTESIAN_POINT('Ctrl Pts',(-7.47735123202398,-0.23879142576123,
16.2231539208491));
#30542=CARTESIAN_POINT('Ctrl Pts',(-7.51594758151656,-0.404029166161908,
16.2154359472327));
#30543=CARTESIAN_POINT('Ctrl Pts',(-7.59541735366078,-0.559690113640392,
16.2077179736164));
#30544=CARTESIAN_POINT('Ctrl Pts',(-7.70661869325987,-0.687936125025659,
16.2));
#30545=CARTESIAN_POINT('',(-9.293419174865,-0.687941029322388,16.2));
#30546=CARTESIAN_POINT('Origin',(-8.5,0.,16.2));
#30547=CARTESIAN_POINT('Ctrl Pts',(-9.293419174865,-0.687941029322388,16.2));
#30548=CARTESIAN_POINT('Ctrl Pts',(-9.20135850648669,-0.793915604248618,
16.2063833455655));
#30549=CARTESIAN_POINT('Ctrl Pts',(-9.08793173951017,-0.881430798173356,
16.212766691131));
#30550=CARTESIAN_POINT('Ctrl Pts',(-8.96187783632725,-0.943160618773336,
16.2191500366966));
#30551=CARTESIAN_POINT('Ctrl Pts',(-8.80946861940179,-1.01779689247079,
16.2268680103129));
#30552=CARTESIAN_POINT('Ctrl Pts',(-8.63860012352652,-1.05473820578714,
16.2345859839293));
#30553=CARTESIAN_POINT('Ctrl Pts',(-8.46897137294775,-1.04972427515045,
16.2423039575456));
#30554=CARTESIAN_POINT('Ctrl Pts',(-8.29934262236897,-1.04471034451375,
16.250021931162));
#30555=CARTESIAN_POINT('Ctrl Pts',(-8.1309536170867,-0.997741169924025,
16.2577399047784));
#30556=CARTESIAN_POINT('Ctrl Pts',(-7.98321924168765,-0.914232549471815,
16.2654578783947));
#30557=CARTESIAN_POINT('Ctrl Pts',(-7.8354848662886,-0.830723929019605,
16.2731758520111));
#30558=CARTESIAN_POINT('Ctrl Pts',(-7.70840512077277,-0.710675862704915,
16.2808938256275));
#30559=CARTESIAN_POINT('Ctrl Pts',(-7.61663135652483,-0.56792899930393,
16.2886117992438));
#30560=CARTESIAN_POINT('Ctrl Pts',(-7.52485759227689,-0.425182135902946,
16.2963297728602));
#30561=CARTESIAN_POINT('Ctrl Pts',(-7.46838980929684,-0.259736475415666,
16.3040477464765));
#30562=CARTESIAN_POINT('Ctrl Pts',(-7.45373855153845,-0.0906671103893211,
16.3117657200929));
#30563=CARTESIAN_POINT('Ctrl Pts',(-7.43908729378006,0.0784022546370248,
16.3194836937093));
#30564=CARTESIAN_POINT('Ctrl Pts',(-7.46625256124332,0.251095324202436,
16.3272016673256));
#30565=CARTESIAN_POINT('Ctrl Pts',(-7.53210229320152,0.407501578067959,
16.334919640942));
#30566=CARTESIAN_POINT('Ctrl Pts',(-7.59795202515973,0.56390783193348,16.3426376145583));
#30567=CARTESIAN_POINT('Ctrl Pts',(-7.70248622161286,0.704027270099115,
16.3503555881747));
#30568=CARTESIAN_POINT('Ctrl Pts',(-7.83365268340161,0.811704861142506,
16.3580735617911));
#30569=CARTESIAN_POINT('Ctrl Pts',(-7.96481914519036,0.919382452185898,
16.3657915354074));
#30570=CARTESIAN_POINT('Ctrl Pts',(-8.12261787231473,0.994618196107047,
16.3735095090238));
#30571=CARTESIAN_POINT('Ctrl Pts',(-8.28885551939544,1.02873783191642,16.3812274826402));
#30572=CARTESIAN_POINT('Ctrl Pts',(-8.45509316647615,1.06285746772579,16.3889454562565));
#30573=CARTESIAN_POINT('Ctrl Pts',(-8.6297697335132,1.05586099542339,16.3966634298729));
#30574=CARTESIAN_POINT('Ctrl Pts',(-8.79274596856292,1.00855506527731,16.4043814034892));
#30575=CARTESIAN_POINT('Ctrl Pts',(-8.95572220361263,0.961249135131234,
16.4120993771056));
#30576=CARTESIAN_POINT('Ctrl Pts',(-9.106998106675,0.873633747141485,16.419817350722));
#30577=CARTESIAN_POINT('Ctrl Pts',(-9.22913238736914,0.755810480769922,
16.4275353243383));
#30578=CARTESIAN_POINT('Ctrl Pts',(-9.35126666806328,0.637987214398357,
16.4352532979547));
#30579=CARTESIAN_POINT('Ctrl Pts',(-9.44425932638919,0.489956069644978,
16.4429712715711));
#30580=CARTESIAN_POINT('Ctrl Pts',(-9.49738881624737,0.328784230496411,
16.4506892451874));
#30581=CARTESIAN_POINT('Ctrl Pts',(-9.53227575775345,0.222952374406485,
16.4557571744075));
#30582=CARTESIAN_POINT('Ctrl Pts',(-9.54997466077663,0.111454567273571,
16.4608251036276));
#30583=CARTESIAN_POINT('Ctrl Pts',(-9.55005247215833,-1.9100347204657E-5,
16.4658930328476));
#30584=CARTESIAN_POINT('Origin',(-8.5,0.,15.5374873996035));
#30585=CARTESIAN_POINT('',(-9.71736724280504,-1.11660654972812E-5,17.1625126003965));
#30586=CARTESIAN_POINT('',(-9.71748246977037,-2.53252437245375E-5,17.1874873996035));
#30587=CARTESIAN_POINT('',(-9.71745,1.66304456946628E-15,15.5374873996035));
#30588=CARTESIAN_POINT('',(-8.18521110449555,1.17604951161381,17.4));
#30589=CARTESIAN_POINT('Ctrl Pts',(-9.71748246977038,-2.53252437245645E-5,
17.1874873996035));
#30590=CARTESIAN_POINT('Ctrl Pts',(-9.71751497142563,-0.0351019928070867,
17.1888631705217));
#30591=CARTESIAN_POINT('Ctrl Pts',(-9.70768334098354,-0.266938032321857,
17.1979569150563));
#30592=CARTESIAN_POINT('Ctrl Pts',(-9.56507989669121,-0.68475363956845,
17.2147686332073));
#30593=CARTESIAN_POINT('Ctrl Pts',(-9.12308418289996,-1.1022924873685,17.2379225540564));
#30594=CARTESIAN_POINT('Ctrl Pts',(-8.53741084518169,-1.26565584737736,
17.2610764749055));
#30595=CARTESIAN_POINT('Ctrl Pts',(-7.94311359864215,-1.13717035634921,
17.2842303957546));
#30596=CARTESIAN_POINT('Ctrl Pts',(-7.47722268493459,-0.746471406749234,
17.3073843166036));
#30597=CARTESIAN_POINT('Ctrl Pts',(-7.24718561960605,-0.183633649692887,
17.3305382374527));
#30598=CARTESIAN_POINT('Ctrl Pts',(-7.3060079723258,0.421518864292242,17.3536921583018));
#30599=CARTESIAN_POINT('Ctrl Pts',(-7.64021327215519,0.929515170005604,
17.3768460791509));
#30600=CARTESIAN_POINT('Ctrl Pts',(-7.99510874416169,1.12516550422184,17.3922820263836));
#30601=CARTESIAN_POINT('Ctrl Pts',(-8.18521110449555,1.17604951161381,17.4));
#30602=CARTESIAN_POINT('',(-8.81478889550434,1.17604951161384,17.4));
#30603=CARTESIAN_POINT('Origin',(-8.5,0.,17.4));
#30604=CARTESIAN_POINT('Ctrl Pts',(-9.71736724280504,-1.11660654973089E-5,
17.1625126003965));
#30605=CARTESIAN_POINT('Ctrl Pts',(-9.71739603884099,-0.0846136171028923,
17.1658299588182));
#30606=CARTESIAN_POINT('Ctrl Pts',(-9.68844277423369,-0.366027787036859,
17.1768652908563));
#30607=CARTESIAN_POINT('Ctrl Pts',(-9.47383591978867,-0.809275294625564,
17.1956185965107));
#30608=CARTESIAN_POINT('Ctrl Pts',(-8.98431387179416,-1.16992433712962,
17.2187725173598));
#30609=CARTESIAN_POINT('Ctrl Pts',(-8.38311431128619,-1.26080160014802,
17.2419264382089));
#30610=CARTESIAN_POINT('Ctrl Pts',(-7.80886733385048,-1.06095167099359,
17.265080359058));
#30611=CARTESIAN_POINT('Ctrl Pts',(-7.39398798803169,-0.616457995871644,
17.2882342799071));
#30612=CARTESIAN_POINT('Ctrl Pts',(-7.23414304365684,-0.0298154777491022,
17.3113882007562));
#30613=CARTESIAN_POINT('Ctrl Pts',(-7.36619075960647,0.563701428344329,
17.3345421216053));
#30614=CARTESIAN_POINT('Ctrl Pts',(-7.75968288434054,1.02723654746506,17.3576960424544));
#30615=CARTESIAN_POINT('Ctrl Pts',(-8.29136184904107,1.24083350426797,17.3795153352526));
#30616=CARTESIAN_POINT('Ctrl Pts',(-8.65756927545989,1.21801527236963,17.3936166544345));
#30617=CARTESIAN_POINT('Ctrl Pts',(-8.81482206889626,1.17607882593354,17.4));
#30618=CARTESIAN_POINT('Origin',(-8.5,0.,15.5374873996035));
#30619=CARTESIAN_POINT('',(-9.71737871990645,-1.72188190057376E-5,16.8625126003965));
#30620=CARTESIAN_POINT('',(-9.71750560220144,-2.14937386861674E-5,16.8874873996035));
#30621=CARTESIAN_POINT('',(-9.71745,1.66304456946628E-15,15.5374873996035));
#30622=CARTESIAN_POINT('Ctrl Pts',(-9.71750560220144,-2.1493738686134E-5,
16.8874873996035));
#30623=CARTESIAN_POINT('Ctrl Pts',(-9.71752782371263,-0.0265897765865916,
16.888529513509));
#30624=CARTESIAN_POINT('Ctrl Pts',(-9.71035795599032,-0.249912775849858,
16.8972896010309));
#30625=CARTESIAN_POINT('Ctrl Pts',(-9.57920029690692,-0.66227603951712,
16.9137676621692));
#30626=CARTESIAN_POINT('Ctrl Pts',(-9.14605408022473,-1.08898896173995,
16.9369215830183));
#30627=CARTESIAN_POINT('Ctrl Pts',(-8.56393482767032,-1.26459288749884,
16.9600755038673));
#30628=CARTESIAN_POINT('Ctrl Pts',(-7.96707289994234,-1.1485954638407,16.9832294247164));
#30629=CARTESIAN_POINT('Ctrl Pts',(-7.49309815860203,-0.767744433222239,
17.0063833455655));
#30630=CARTESIAN_POINT('Ctrl Pts',(-7.25130401707404,-0.209859896869422,
17.0295372664146));
#30631=CARTESIAN_POINT('Ctrl Pts',(-7.29744557308788,0.396416047559612,
17.0526911872637));
#30632=CARTESIAN_POINT('Ctrl Pts',(-7.62088308273839,0.911282765764439,
17.0758451081128));
#30633=CARTESIAN_POINT('Ctrl Pts',(-8.14703538592992,1.21601760624665,17.0989990289619));
#30634=CARTESIAN_POINT('Ctrl Pts',(-8.75457747423087,1.24035201730987,17.122152949811));
#30635=CARTESIAN_POINT('Ctrl Pts',(-9.30341679390951,0.978674783003138,
17.14530687066));
#30636=CARTESIAN_POINT('Ctrl Pts',(-9.64539351645688,0.520283291202953,
17.1670850205909));
#30637=CARTESIAN_POINT('Ctrl Pts',(-9.71733263953124,0.161675531135822,
17.1811451969054));
#30638=CARTESIAN_POINT('Ctrl Pts',(-9.71748246977038,-2.53252437245645E-5,
17.1874873996035));
#30639=CARTESIAN_POINT('Ctrl Pts',(-9.71737871990645,-1.72188190057931E-5,
16.8625126003965));
#30640=CARTESIAN_POINT('Ctrl Pts',(-9.71741919686537,-0.0761083706980662,
16.8654963018055));
#30641=CARTESIAN_POINT('Ctrl Pts',(-9.69220246389315,-0.348998849073912,
16.8761979768309));
#30642=CARTESIAN_POINT('Ctrl Pts',(-9.49058656515595,-0.788683177200059,
16.8946176254726));
#30643=CARTESIAN_POINT('Ctrl Pts',(-9.0087322805331,-1.15951471047599,16.9177715463217));
#30644=CARTESIAN_POINT('Ctrl Pts',(-8.40956987168007,-1.26297477764059,
16.9409254671708));
#30645=CARTESIAN_POINT('Ctrl Pts',(-7.83125966571002,-1.07520661380189,
16.9640793880199));
#30646=CARTESIAN_POINT('Ctrl Pts',(-7.40715369881707,-0.639507512896534,
16.987233308869));
#30647=CARTESIAN_POINT('Ctrl Pts',(-7.23504618881006,-0.0563449432224961,
17.010387229718));
#30648=CARTESIAN_POINT('Ctrl Pts',(-7.35462325340267,0.539810156841002,
17.0335411505671));
#30649=CARTESIAN_POINT('Ctrl Pts',(-7.73831172357029,1.01149091274223,17.0566950714162));
#30650=CARTESIAN_POINT('Ctrl Pts',(-8.29763721617962,1.24993287858306,17.0798489922653));
#30651=CARTESIAN_POINT('Ctrl Pts',(-8.90362536310944,1.20015393300998,17.1030029131144));
#30652=CARTESIAN_POINT('Ctrl Pts',(-9.41654189659505,0.873632559821981,
17.1261568339635));
#30653=CARTESIAN_POINT('Ctrl Pts',(-9.67490638243313,0.421305704246767,
17.1459933963908));
#30654=CARTESIAN_POINT('Ctrl Pts',(-9.71732904365461,0.112217536477445,
17.1581119852019));
#30655=CARTESIAN_POINT('Ctrl Pts',(-9.71736724280504,-1.11660654973089E-5,
17.1625126003965));
#30656=CARTESIAN_POINT('Origin',(-8.5,0.,15.5374873996035));
#30657=CARTESIAN_POINT('',(-9.71739489784702,-2.21442888292955E-5,16.5625126003965));
#30658=CARTESIAN_POINT('',(-9.71752534862784,-1.58793637348338E-5,16.5874873996035));
#30659=CARTESIAN_POINT('',(-9.71745,1.66304456946628E-15,15.5374873996035));
#30660=CARTESIAN_POINT('Ctrl Pts',(-9.71752534862784,-1.5879363734872E-5,
16.5874873996035));
#30661=CARTESIAN_POINT('Ctrl Pts',(-9.71753738116228,-0.0180768584738382,
16.5881958564963));
#30662=CARTESIAN_POINT('Ctrl Pts',(-9.71285071230468,-0.232889024209207,
16.5966222870055));
#30663=CARTESIAN_POINT('Ctrl Pts',(-9.59284627947019,-0.639507500190754,
16.612766691131));
#30664=CARTESIAN_POINT('Ctrl Pts',(-9.1687403210034,-1.07520659243964,16.6359206119801));
#30665=CARTESIAN_POINT('Ctrl Pts',(-8.59043012652324,-1.26297475254772,
16.6590745328292));
#30666=CARTESIAN_POINT('Ctrl Pts',(-7.99126772957441,-1.15951468743868,
16.6822284536783));
#30667=CARTESIAN_POINT('Ctrl Pts',(-7.50941345452508,-0.788683161530444,
16.7053823745274));
#30668=CARTESIAN_POINT('Ctrl Pts',(-7.2559776502202,-0.235989886660555,
16.7285362953765));
#30669=CARTESIAN_POINT('Ctrl Pts',(-7.28939985343257,0.371120086345011,
16.7516902162256));
#30670=CARTESIAN_POINT('Ctrl Pts',(-7.60197326804091,0.892653808620445,
16.7748441370746));
#30671=CARTESIAN_POINT('Ctrl Pts',(-8.12162186829395,1.20835128286614,16.7979980579237));
#30672=CARTESIAN_POINT('Ctrl Pts',(-8.72852034550391,1.24541610919772,16.8211519787728));
#30673=CARTESIAN_POINT('Ctrl Pts',(-9.28272451943119,0.995301542266061,
16.8443058996219));
#30674=CARTESIAN_POINT('Ctrl Pts',(-9.63962067752837,0.537268072859732,
16.8664177065655));
#30675=CARTESIAN_POINT('Ctrl Pts',(-9.71736324953685,0.170176915580277,
16.8808115398927));
#30676=CARTESIAN_POINT('Ctrl Pts',(-9.71750560220144,-2.1493738686134E-5,
16.8874873996035));
#30677=CARTESIAN_POINT('Ctrl Pts',(-9.71739489784702,-2.2144288829358E-5,
16.5625126003965));
#30678=CARTESIAN_POINT('Ctrl Pts',(-9.71744207005576,-0.0676017066010113,
16.5651626447928));
#30679=CARTESIAN_POINT('Ctrl Pts',(-9.69577211517131,-0.331969647279349,
16.5755306628055));
#30680=CARTESIAN_POINT('Ctrl Pts',(-9.50690186140351,-0.767744448476627,
16.5936166544345));
#30681=CARTESIAN_POINT('Ctrl Pts',(-9.0329271106457,-1.14859548666069,16.6167705752836));
#30682=CARTESIAN_POINT('Ctrl Pts',(-8.4360651710595,-1.26459291262403,16.6399244961327));
#30683=CARTESIAN_POINT('Ctrl Pts',(-7.85394590693938,-1.08898898337596,
16.6630784169817));
#30684=CARTESIAN_POINT('Ctrl Pts',(-7.42079968165148,-0.662276052675294,
16.6862323378308));
#30685=CARTESIAN_POINT('Ctrl Pts',(-7.23650529822705,-0.0828494758703863,
16.7093862586799));
#30686=CARTESIAN_POINT('Ctrl Pts',(-7.34355903464176,0.515681287920065,
16.732540179529));
#30687=CARTESIAN_POINT('Ctrl Pts',(-7.71727546501759,0.995301562040781,
16.7556941003781));
#30688=CARTESIAN_POINT('Ctrl Pts',(-8.27147964995585,1.24541613394172,16.7788480212272));
#30689=CARTESIAN_POINT('Ctrl Pts',(-8.8783781392237,1.20835130687373,16.8020019420763));
#30690=CARTESIAN_POINT('Ctrl Pts',(-9.39802674980115,0.892653826355733,
16.8251558629254));
#30691=CARTESIAN_POINT('Ctrl Pts',(-9.67032078285669,0.438326893942781,
16.8453260823654));
#30692=CARTESIAN_POINT('Ctrl Pts',(-9.7173144946656,0.120717458075642,16.8577783281891));
#30693=CARTESIAN_POINT('Ctrl Pts',(-9.71737871990645,-1.72188190057931E-5,
16.8625126003965));
#30694=CARTESIAN_POINT('Origin',(-8.5,0.,15.5374873996035));
#30695=CARTESIAN_POINT('',(-9.71741527458843,-3.00182063334153E-5,16.2625126003965));
#30696=CARTESIAN_POINT('',(-9.71753950048363,-8.82892751896623E-6,16.2874873996035));
#30697=CARTESIAN_POINT('',(-9.71745,1.66304456946628E-15,15.5374873996035));
#30698=CARTESIAN_POINT('',(-8.81478889550445,1.17604951161381,16.2));
#30699=CARTESIAN_POINT('Ctrl Pts',(-8.81478889550445,1.17604951161381,16.2));
#30700=CARTESIAN_POINT('Ctrl Pts',(-9.00489125583831,1.12516550422184,16.2077179736164));
#30701=CARTESIAN_POINT('Ctrl Pts',(-9.35978667802179,0.929514905730451,
16.2231539208491));
#30702=CARTESIAN_POINT('Ctrl Pts',(-9.66055713486829,0.472340269425348,
16.2439914543146));
#30703=CARTESIAN_POINT('Ctrl Pts',(-9.7173031168173,0.137707734298517,16.2571110141637));
#30704=CARTESIAN_POINT('Ctrl Pts',(-9.71741527458843,-3.00182063335264E-5,
16.2625126003965));
#30705=CARTESIAN_POINT('',(-8.18517792975417,1.1760787964605,16.2));
#30706=CARTESIAN_POINT('Origin',(-8.5,0.,16.2));
#30707=CARTESIAN_POINT('Ctrl Pts',(-8.18517792975417,1.1760787964605,16.2));
#30708=CARTESIAN_POINT('Ctrl Pts',(-8.34243072315718,1.21801524478933,16.2063833455655));
#30709=CARTESIAN_POINT('Ctrl Pts',(-8.70863814132373,1.24083347266754,16.2204846647474));
#30710=CARTESIAN_POINT('Ctrl Pts',(-9.24031710111236,1.02723652833138,16.2423039575456));
#30711=CARTESIAN_POINT('Ctrl Pts',(-9.62743963500528,0.571204805999074,
16.2650830785146));
#30712=CARTESIAN_POINT('Ctrl Pts',(-9.71746327074259,0.187187292270235,
16.2801442258672));
#30713=CARTESIAN_POINT('Ctrl Pts',(-9.71753950048363,-8.82892751894945E-6,
16.2874873996035));
#30714=CARTESIAN_POINT('Origin',(-8.5,0.,15.5374873996035));
#30715=CARTESIAN_POINT('Ctrl Pts',(-9.71753950048363,-8.82892751894945E-6,
16.2874873996035));
#30716=CARTESIAN_POINT('Ctrl Pts',(-9.71754339129418,-0.00956342838294255,
16.2878621994836));
#30717=CARTESIAN_POINT('Ctrl Pts',(-9.71516274507233,-0.215866810278111,
16.2959549729801));
#30718=CARTESIAN_POINT('Ctrl Pts',(-9.60601198986148,-0.616457983927628,
16.3117657200929));
#30719=CARTESIAN_POINT('Ctrl Pts',(-9.19113265245436,-1.06095164978761,
16.334919640942));
#30720=CARTESIAN_POINT('Ctrl Pts',(-8.61688568636888,-1.26080157516723,
16.3580735617911));
#30721=CARTESIAN_POINT('Ctrl Pts',(-8.01568613783619,-1.16992431385386,
16.3812274826402));
#30722=CARTESIAN_POINT('Ctrl Pts',(-7.52616409955547,-0.809275278562791,
16.4043814034892));
#30723=CARTESIAN_POINT('Ctrl Pts',(-7.26119801228416,-0.26201616100183,
16.4275353243383));
#30724=CARTESIAN_POINT('Ctrl Pts',(-7.28188617544855,0.345661023092506,
16.4506892451874));
#30725=CARTESIAN_POINT('Ctrl Pts',(-7.58345812161518,0.873632542466389,
16.4738431660365));
#30726=CARTESIAN_POINT('Ctrl Pts',(-8.09637464490968,1.20015390916439,16.4969970868856));
#30727=CARTESIAN_POINT('Ctrl Pts',(-8.7023627797999,1.24993285374973,16.5201510077347));
#30728=CARTESIAN_POINT('Ctrl Pts',(-9.26168826129643,1.01149089264566,16.5433049285838));
#30729=CARTESIAN_POINT('Ctrl Pts',(-9.63363673657241,0.554242495534025,
16.56575039254));
#30730=CARTESIAN_POINT('Ctrl Pts',(-9.71740629798092,0.178680575422754,
16.5804778828799));
#30731=CARTESIAN_POINT('Ctrl Pts',(-9.71752534862784,-1.5879363734872E-5,
16.5874873996035));
#30732=CARTESIAN_POINT('Ctrl Pts',(-9.71741527458843,-3.00182063335264E-5,
16.2625126003965));
#30733=CARTESIAN_POINT('Ctrl Pts',(-9.71746337172782,-0.059096740164705,
16.2648289877801));
#30734=CARTESIAN_POINT('Ctrl Pts',(-9.69914896928468,-0.314938316431683,
16.27486334878));
#30735=CARTESIAN_POINT('Ctrl Pts',(-9.52277733259636,-0.746471423726082,
16.2926156833963));
#30736=CARTESIAN_POINT('Ctrl Pts',(-9.05688641176464,-1.13717038838356,
16.3157696042454));
#30737=CARTESIAN_POINT('Ctrl Pts',(-8.46258915349396,-1.26565587137657,
16.3389235250945));
#30738=CARTESIAN_POINT('Ctrl Pts',(-7.87691580481983,-1.10229251092252,
16.3620774459436));
#30739=CARTESIAN_POINT('Ctrl Pts',(-7.43492008199845,-0.684753652714294,
16.3852313667927));
#30740=CARTESIAN_POINT('Ctrl Pts',(-7.23851963711968,-0.109317543695422,
16.4083852876418));
#30741=CARTESIAN_POINT('Ctrl Pts',(-7.33300308119116,0.491325759444495,
16.4315392084909));
#30742=CARTESIAN_POINT('Ctrl Pts',(-7.69658319014803,0.978674802377791,
16.45469312934));
#30743=CARTESIAN_POINT('Ctrl Pts',(-8.24542252070005,1.24035204198393,16.477847050189));
#30744=CARTESIAN_POINT('Ctrl Pts',(-8.85296462108838,1.21601763039105,16.5010009710381));
#30745=CARTESIAN_POINT('Ctrl Pts',(-9.37911693472505,0.911282783877038,
16.5241548918872));
#30746=CARTESIAN_POINT('Ctrl Pts',(-9.66553593534035,0.455344290414368,
16.54465876834));
#30747=CARTESIAN_POINT('Ctrl Pts',(-9.7173046859942,0.129216610729656,16.5574446711764));
#30748=CARTESIAN_POINT('Ctrl Pts',(-9.71739489784702,-2.2144288829358E-5,
16.5625126003965));
#30749=CARTESIAN_POINT('Ctrl Pts',(-7.70661869325987,-0.687936125025659,
16.2));
#30750=CARTESIAN_POINT('Ctrl Pts',(-7.59541735366078,-0.559690113640392,
16.2077179736164));
#30751=CARTESIAN_POINT('Ctrl Pts',(-7.43647780937234,-0.248368218683425,
16.2231539208491));
#30752=CARTESIAN_POINT('Ctrl Pts',(-7.44330902884952,0.276075381285195,
16.2463078416982));
#30753=CARTESIAN_POINT('Ctrl Pts',(-7.69382549331944,0.73679971847695,16.2694617625473));
#30754=CARTESIAN_POINT('Ctrl Pts',(-8.1302325908592,1.02765943396112,16.2926156833963));
#30755=CARTESIAN_POINT('Ctrl Pts',(-8.65190784365933,1.0815384208056,16.3157696042454));
#30756=CARTESIAN_POINT('Ctrl Pts',(-9.13855352406923,0.886033166372978,
16.3389235250945));
#30757=CARTESIAN_POINT('Ctrl Pts',(-9.47795643253951,0.486215332577987,
16.3620774459436));
#30758=CARTESIAN_POINT('Ctrl Pts',(-9.59185294146457,-0.0257170578466189,
16.3852313667927));
#30759=CARTESIAN_POINT('Ctrl Pts',(-9.45398019676664,-0.531720012257096,
16.4083852876418));
#30760=CARTESIAN_POINT('Ctrl Pts',(-9.09612994237326,-0.915113825982153,
16.4315392084909));
#30761=CARTESIAN_POINT('Ctrl Pts',(-8.60081864491845,-1.0874924917517,16.4546931293399));
#30762=CARTESIAN_POINT('Ctrl Pts',(-8.08225965201181,-1.0091071682434,16.4778470501891));
#30763=CARTESIAN_POINT('Ctrl Pts',(-7.66002704089959,-0.698032748793615,
16.5010009710381));
#30764=CARTESIAN_POINT('Ctrl Pts',(-7.43148304464216,-0.225999565212552,
16.5241548918872));
#30765=CARTESIAN_POINT('Ctrl Pts',(-7.44932742440225,0.298146651073506,
16.5473088127363));
#30766=CARTESIAN_POINT('Ctrl Pts',(-7.70944545854705,0.753543498988833,
16.5704627335854));
#30767=CARTESIAN_POINT('Ctrl Pts',(-8.15185676177228,1.03518142019264,16.5936166544345));
#30768=CARTESIAN_POINT('Ctrl Pts',(-8.67454610461857,1.07811777873637,16.6167705752836));
#30769=CARTESIAN_POINT('Ctrl Pts',(-9.15698701645849,0.872451917012778,
16.6399244961327));
#30770=CARTESIAN_POINT('Ctrl Pts',(-9.48793387630323,0.465608143608788,
16.6630784169817));
#30771=CARTESIAN_POINT('Ctrl Pts',(-9.59107394204218,-0.0485997976939159,
16.6862323378308));
#30772=CARTESIAN_POINT('Ctrl Pts',(-9.44262423760454,-0.551601154832076,
16.7093862586799));
#30773=CARTESIAN_POINT('Ctrl Pts',(-9.07681564835161,-0.927409292144124,
16.732540179529));
#30774=CARTESIAN_POINT('Ctrl Pts',(-8.57799965161777,-1.08936694537793,
16.7556941003781));
#30775=CARTESIAN_POINT('Ctrl Pts',(-8.0611977845711,-1.00012844328667,16.7788480212272));
#30776=CARTESIAN_POINT('Ctrl Pts',(-7.64557893022037,-0.680271212717664,
16.8020019420763));
#30777=CARTESIAN_POINT('Ctrl Pts',(-7.42698027064457,-0.203550848069529,
16.8251558629253));
#30778=CARTESIAN_POINT('Ctrl Pts',(-7.45580827638879,0.320106125648607,
16.8483097837744));
#30779=CARTESIAN_POINT('Ctrl Pts',(-7.725415523241,0.769950112474704,16.8714637046235));
#30780=CARTESIAN_POINT('Ctrl Pts',(-8.17363351586963,1.04225198746374,16.8946176254726));
#30781=CARTESIAN_POINT('Ctrl Pts',(-8.69710806588661,1.0742219033788,16.9177715463217));
#30782=CARTESIAN_POINT('Ctrl Pts',(-9.17513164224789,0.85848794573378,16.9409254671708));
#30783=CARTESIAN_POINT('Ctrl Pts',(-9.49747721351624,0.444796016005563,
16.9640793880199));
#30784=CARTESIAN_POINT('Ctrl Pts',(-9.58981540101927,-0.0714610315684377,
16.987233308869));
#30785=CARTESIAN_POINT('Ctrl Pts',(-9.43085402421615,-0.571239943403776,
17.0103872297181));
#30786=CARTESIAN_POINT('Ctrl Pts',(-9.05724784561501,-0.939297144624521,
17.0335411505671));
#30787=CARTESIAN_POINT('Ctrl Pts',(-8.55514638181166,-1.09076265239848,
17.0566950714162));
#30788=CARTESIAN_POINT('Ctrl Pts',(-8.04032876276599,-0.990710170092501,
17.0798489922653));
#30789=CARTESIAN_POINT('Ctrl Pts',(-7.63150632580228,-0.662210710359089,
17.1030029131144));
#30790=CARTESIAN_POINT('Ctrl Pts',(-7.42294907251177,-0.181012672144712,
17.1261568339635));
#30791=CARTESIAN_POINT('Ctrl Pts',(-7.46274803589435,0.341924918101235,
17.1493107548126));
#30792=CARTESIAN_POINT('Ctrl Pts',(-7.74172600532555,0.786018343528881,
17.1724646756617));
#30793=CARTESIAN_POINT('Ctrl Pts',(-8.19555370550331,1.04886450229546,17.1956185965107));
#30794=CARTESIAN_POINT('Ctrl Pts',(-8.71958339618863,1.06985391874582,17.2187725173598));
#30795=CARTESIAN_POINT('Ctrl Pts',(-9.19297956818299,0.844146691553324,
17.2419264382089));
#30796=CARTESIAN_POINT('Ctrl Pts',(-9.50658215125916,0.423788385239755,
17.265080359058));
#30797=CARTESIAN_POINT('Ctrl Pts',(-9.58807795211741,-0.0942908127739469,
17.2882342799071));
#30798=CARTESIAN_POINT('Ctrl Pts',(-9.41867460636201,-0.590627785051402,
17.3113882007562));
#30799=CARTESIAN_POINT('Ctrl Pts',(-9.03743537760339,-0.950771975017998,
17.3345421216053));
#30800=CARTESIAN_POINT('Ctrl Pts',(-8.53226837120644,-1.09167949840319,
17.3576960424544));
#30801=CARTESIAN_POINT('Ctrl Pts',(-8.01966289369923,-0.980855551523517,
17.3808499633034));
#30802=CARTESIAN_POINT('Ctrl Pts',(-7.61781308591713,-0.643861862275552,
17.4040038841525));
#30803=CARTESIAN_POINT('Ctrl Pts',(-7.41939678766957,-0.158391470321163,
17.4271578050016));
#30804=CARTESIAN_POINT('Ctrl Pts',(-7.47013345249442,0.36357711560498,17.4503117258507));
#30805=CARTESIAN_POINT('Ctrl Pts',(-7.75839907765424,0.801744531621737,
17.4734656466998));
#30806=CARTESIAN_POINT('Ctrl Pts',(-8.06451081542912,0.970500879693911,
17.4889015939325));
#30807=CARTESIAN_POINT('Ctrl Pts',(-8.22848181102368,1.01439039972538,17.4966195675489));
#30808=CARTESIAN_POINT('Ctrl Pts',(-7.66447275106929,-0.724480616192546,
16.1677934774837));
#30809=CARTESIAN_POINT('Ctrl Pts',(-7.54736418225968,-0.589421929822254,
16.1755114511001));
#30810=CARTESIAN_POINT('Ctrl Pts',(-7.37998146343654,-0.261562016542889,
16.1909473983328));
#30811=CARTESIAN_POINT('Ctrl Pts',(-7.38717557044174,0.290741036955474,
16.2141013191819));
#30812=CARTESIAN_POINT('Ctrl Pts',(-7.65099995172245,0.775939937785307,
16.237255240031));
#30813=CARTESIAN_POINT('Ctrl Pts',(-8.11058983432182,1.08225068123072,16.26040916088));
#30814=CARTESIAN_POINT('Ctrl Pts',(-8.65997748072132,1.13899182356782,16.2835630817291));
#30815=CARTESIAN_POINT('Ctrl Pts',(-9.17247471641694,0.933100953692445,
16.3067170025782));
#30816=CARTESIAN_POINT('Ctrl Pts',(-9.52990736070048,0.512044026958499,
16.3298709234273));
#30817=CARTESIAN_POINT('Ctrl Pts',(-9.64985427141858,-0.0270831974620941,
16.3530248442764));
#30818=CARTESIAN_POINT('Ctrl Pts',(-9.50465746113159,-0.55996600281394,
16.3761787651255));
#30819=CARTESIAN_POINT('Ctrl Pts',(-9.12779751240029,-0.963726433917306,
16.3993326859746));
#30820=CARTESIAN_POINT('Ctrl Pts',(-8.60617432540192,-1.14526218622354,
16.4224866068237));
#30821=CARTESIAN_POINT('Ctrl Pts',(-8.06006848061994,-1.06271288344689,
16.4456405276728));
#30822=CARTESIAN_POINT('Ctrl Pts',(-7.61540606045155,-0.735113592050007,
16.4687944485218));
#30823=CARTESIAN_POINT('Ctrl Pts',(-7.3747213671895,-0.238005097142311,
16.4919483693709));
#30824=CARTESIAN_POINT('Ctrl Pts',(-7.39351367475101,0.31398477507984,16.51510229022));
#30825=CARTESIAN_POINT('Ctrl Pts',(-7.66744967956976,0.793573180148018,
16.5382562110691));
#30826=CARTESIAN_POINT('Ctrl Pts',(-8.13336272281808,1.09017224984989,16.5614101319182));
#30827=CARTESIAN_POINT('Ctrl Pts',(-8.68381832967901,1.13538947040749,16.5845640527673));
#30828=CARTESIAN_POINT('Ctrl Pts',(-9.19188743140447,0.918798242223738,
16.6077179736164));
#30829=CARTESIAN_POINT('Ctrl Pts',(-9.54041482548246,0.490342144444559,
16.6308718944655));
#30830=CARTESIAN_POINT('Ctrl Pts',(-9.64903389004738,-0.0511815124969747,
16.6540258153145));
#30831=CARTESIAN_POINT('Ctrl Pts',(-9.49269825155976,-0.580903269951635,
16.6771797361636));
#30832=CARTESIAN_POINT('Ctrl Pts',(-9.1074572059022,-0.976675058909296,
16.7003336570127));
#30833=CARTESIAN_POINT('Ctrl Pts',(-8.58214314325293,-1.14723621443453,
16.7234875778618));
#30834=CARTESIAN_POINT('Ctrl Pts',(-8.03788776623887,-1.05325719133734,
16.7466414987109));
#30835=CARTESIAN_POINT('Ctrl Pts',(-7.60019043832194,-0.71640852898859,
16.76979541956));
#30836=CARTESIAN_POINT('Ctrl Pts',(-7.36997939716978,-0.214363860933204,
16.7929493404091));
#30837=CARTESIAN_POINT('Ctrl Pts',(-7.40033880207005,0.337110779214075,
16.8161032612581));
#30838=CARTESIAN_POINT('Ctrl Pts',(-7.68426810484097,0.810851344523284,
16.8392571821072));
#30839=CARTESIAN_POINT('Ctrl Pts',(-8.15629630001107,1.09761841926454,16.8624111029563));
#30840=CARTESIAN_POINT('Ctrl Pts',(-8.70757882575904,1.13128663865177,16.8855650238054));
#30841=CARTESIAN_POINT('Ctrl Pts',(-9.21099593464233,0.904092477911206,
16.9087189446545));
#30842=CARTESIAN_POINT('Ctrl Pts',(-9.55046512313816,0.468424436561869,
16.9318728655036));
#30843=CARTESIAN_POINT('Ctrl Pts',(-9.64770849290277,-0.0752571791204098,
16.9550267863527));
#30844=CARTESIAN_POINT('Ctrl Pts',(-9.48030278177974,-0.601585308774891,
16.9781807072017));
#30845=CARTESIAN_POINT('Ctrl Pts',(-9.08684992381825,-0.989194416996331,
17.0013346280508));
#30846=CARTESIAN_POINT('Ctrl Pts',(-8.55807586376454,-1.1487060640986,17.0244885488999));
#30847=CARTESIAN_POINT('Ctrl Pts',(-8.01591014182478,-1.0433386013419,17.047642469749));
#30848=CARTESIAN_POINT('Ctrl Pts',(-7.58537027006887,-0.697388617980139,
17.0707963905981));
#30849=CARTESIAN_POINT('Ctrl Pts',(-7.36573405403253,-0.190628413719615,
17.0939503114472));
#30850=CARTESIAN_POINT('Ctrl Pts',(-7.40764721495886,0.360088627920694,
17.1171042322963));
#30851=CARTESIAN_POINT('Ctrl Pts',(-7.70144503112983,0.827773150940734,
17.1402581531454));
#30852=CARTESIAN_POINT('Ctrl Pts',(-8.17938093231218,1.10458220361253,17.1634120739944));
#30853=CARTESIAN_POINT('Ctrl Pts',(-8.73124808886938,1.12668661826717,17.1865659948435));
#30854=CARTESIAN_POINT('Ctrl Pts',(-9.22979197675849,0.888989388703262,
17.2097199156926));
#30855=CARTESIAN_POINT('Ctrl Pts',(-9.56005373270004,0.446300840012277,
17.2328738365417));
#30856=CARTESIAN_POINT('Ctrl Pts',(-9.64587874737083,-0.0992997222485111,
17.2560277573908));
#30857=CARTESIAN_POINT('Ctrl Pts',(-9.46747636980508,-0.622003069890418,
17.2791816782399));
#30858=CARTESIAN_POINT('Ctrl Pts',(-9.06598497936891,-1.00127881246817,
17.302335599089));
#30859=CARTESIAN_POINT('Ctrl Pts',(-8.53398252919819,-1.14967161472792,
17.3254895199381));
#30860=CARTESIAN_POINT('Ctrl Pts',(-7.99414646201354,-1.03296048646541,
17.3486434407871));
#30861=CARTESIAN_POINT('Ctrl Pts',(-7.57094961892295,-0.678065043766779,
17.3717973616362));
#30862=CARTESIAN_POINT('Ctrl Pts',(-7.36199306498173,-0.166805530111738,
17.3949512824853));
#30863=CARTESIAN_POINT('Ctrl Pts',(-7.41542495910488,0.382891031834067,
17.4181052033344));
#30864=CARTESIAN_POINT('Ctrl Pts',(-7.71900380915456,0.844334744416359,
17.4412591241835));
#30865=CARTESIAN_POINT('Ctrl Pts',(-8.04137679167331,1.02205575453655,17.4566950714162));
#30866=CARTESIAN_POINT('Ctrl Pts',(-8.21405824218097,1.06827677035486,17.4644130450326));
#30867=CARTESIAN_POINT('Ctrl Pts',(-7.62232680887872,-0.761025107359433,
16.1355869549674));
#30868=CARTESIAN_POINT('Ctrl Pts',(-7.49931101085859,-0.619153746004116,
16.1433049285838));
#30869=CARTESIAN_POINT('Ctrl Pts',(-7.32348511750074,-0.274755814402354,
16.1587408758165));
#30870=CARTESIAN_POINT('Ctrl Pts',(-7.33104211203396,0.305406692625752,
16.1818947966656));
#30871=CARTESIAN_POINT('Ctrl Pts',(-7.60817441012546,0.815080157093664,
16.2050487175147));
#30872=CARTESIAN_POINT('Ctrl Pts',(-8.09094707778444,1.13684192850031,16.2282026383638));
#30873=CARTESIAN_POINT('Ctrl Pts',(-8.66804711778331,1.19644522633004,16.2513565592128));
#30874=CARTESIAN_POINT('Ctrl Pts',(-9.20639590876465,0.980168741011912,
16.2745104800619));
#30875=CARTESIAN_POINT('Ctrl Pts',(-9.58185828886143,0.537872721339012,
16.297664400911));
#30876=CARTESIAN_POINT('Ctrl Pts',(-9.70785560137258,-0.0284493370775698,
16.3208183217601));
#30877=CARTESIAN_POINT('Ctrl Pts',(-9.55533472549653,-0.588211993370783,
16.3439722426092));
#30878=CARTESIAN_POINT('Ctrl Pts',(-9.15946508242732,-1.01233904185246,
16.3671261634583));
#30879=CARTESIAN_POINT('Ctrl Pts',(-8.6115300058854,-1.20303188069538,16.3902800843074));
#30880=CARTESIAN_POINT('Ctrl Pts',(-8.03787730922807,-1.11631859865037,
16.4134340051565));
#30881=CARTESIAN_POINT('Ctrl Pts',(-7.57078508000351,-0.772194435306399,
16.4365879260055));
#30882=CARTESIAN_POINT('Ctrl Pts',(-7.31795968973683,-0.25001062907207,
16.4597418468546));
#30883=CARTESIAN_POINT('Ctrl Pts',(-7.33769992509978,0.329822899086172,
16.4828957677037));
#30884=CARTESIAN_POINT('Ctrl Pts',(-7.62545390059247,0.833602861307204,
16.5060496885528));
#30885=CARTESIAN_POINT('Ctrl Pts',(-8.11486868386388,1.14516307950714,16.5292036094019));
#30886=CARTESIAN_POINT('Ctrl Pts',(-8.69309055473946,1.19266116207861,16.552357530251));
#30887=CARTESIAN_POINT('Ctrl Pts',(-9.22678784635045,0.965144567434699,
16.5755114511001));
#30888=CARTESIAN_POINT('Ctrl Pts',(-9.5928957746617,0.515076145280332,16.5986653719492));
#30889=CARTESIAN_POINT('Ctrl Pts',(-9.70699383805257,-0.0537632273000342,
16.6218192927982));
#30890=CARTESIAN_POINT('Ctrl Pts',(-9.54277226551496,-0.610205385071195,
16.6449732136473));
#30891=CARTESIAN_POINT('Ctrl Pts',(-9.1380987634528,-1.02594082567447,16.6681271344964));
#30892=CARTESIAN_POINT('Ctrl Pts',(-8.58628663488808,-1.20510548349113,
16.6912810553455));
#30893=CARTESIAN_POINT('Ctrl Pts',(-8.01457774790664,-1.10638593938801,
16.7144349761946));
#30894=CARTESIAN_POINT('Ctrl Pts',(-7.55480194642351,-0.752545845259518,
16.7375888970437));
#30895=CARTESIAN_POINT('Ctrl Pts',(-7.31297852369499,-0.22517687379688,
16.7607428178928));
#30896=CARTESIAN_POINT('Ctrl Pts',(-7.3448693277513,0.354115432779543,16.7838967387418));
#30897=CARTESIAN_POINT('Ctrl Pts',(-7.64312068644094,0.851752576571865,
16.8070506595909));
#30898=CARTESIAN_POINT('Ctrl Pts',(-8.13895908415251,1.15298485106534,16.83020458044));
#30899=CARTESIAN_POINT('Ctrl Pts',(-8.71804958563147,1.18835137392474,16.8533585012891));
#30900=CARTESIAN_POINT('Ctrl Pts',(-9.24686022703676,0.949697010088635,
16.8765124221382));
#30901=CARTESIAN_POINT('Ctrl Pts',(-9.60345303276009,0.492052857118175,
16.8996663429873));
#30902=CARTESIAN_POINT('Ctrl Pts',(-9.70560158478626,-0.0790533266723822,
16.9228202638364));
#30903=CARTESIAN_POINT('Ctrl Pts',(-9.52975153934333,-0.631930674146006,
16.9459741846855));
#30904=CARTESIAN_POINT('Ctrl Pts',(-9.11645200202149,-1.03909168936814,
16.9691281055346));
#30905=CARTESIAN_POINT('Ctrl Pts',(-8.56100534571743,-1.20664947579872,
16.9922820263836));
#30906=CARTESIAN_POINT('Ctrl Pts',(-7.99149152088356,-1.0959670325913,17.0154359472327));
#30907=CARTESIAN_POINT('Ctrl Pts',(-7.53923421433545,-0.732566525601189,
17.0385898680818));
#30908=CARTESIAN_POINT('Ctrl Pts',(-7.30851903555328,-0.200244155294519,
17.0617437889309));
#30909=CARTESIAN_POINT('Ctrl Pts',(-7.35254639402337,0.378252337740153,
17.08489770978));
#30910=CARTESIAN_POINT('Ctrl Pts',(-7.66116405693411,0.869527958352586,
17.1080516306291));
#30911=CARTESIAN_POINT('Ctrl Pts',(-8.16320815912104,1.16029990492959,17.1312055514782));
#30912=CARTESIAN_POINT('Ctrl Pts',(-8.74291278155013,1.18351931778852,17.1543594723273));
#30913=CARTESIAN_POINT('Ctrl Pts',(-9.26660438533401,0.9338320858532,17.1775133931763));
#30914=CARTESIAN_POINT('Ctrl Pts',(-9.61352531414093,0.468813294784797,
17.2006673140254));
#30915=CARTESIAN_POINT('Ctrl Pts',(-9.70367954262425,-0.104308631723075,
17.2238212348745));
#30916=CARTESIAN_POINT('Ctrl Pts',(-9.51627813324814,-0.653378354729435,
17.2469751557236));
#30917=CARTESIAN_POINT('Ctrl Pts',(-9.09453458113444,-1.05178564991833,
17.2701290765727));
#30918=CARTESIAN_POINT('Ctrl Pts',(-8.53569668718994,-1.20766373105264,
17.2932829974218));
#30919=CARTESIAN_POINT('Ctrl Pts',(-7.96863003032785,-1.08506542140731,
17.3164369182709));
#30920=CARTESIAN_POINT('Ctrl Pts',(-7.52408615192877,-0.712268225258007,
17.3395908391199));
#30921=CARTESIAN_POINT('Ctrl Pts',(-7.30458934229389,-0.175219589902312,
17.362744759969));
#30922=CARTESIAN_POINT('Ctrl Pts',(-7.36071646571534,0.402204948063154,
17.3858986808181));
#30923=CARTESIAN_POINT('Ctrl Pts',(-7.67960854065487,0.886924957210982,
17.4090526016672));
#30924=CARTESIAN_POINT('Ctrl Pts',(-8.0182427679175,1.0736106293792,17.4244885488999));
#30925=CARTESIAN_POINT('Ctrl Pts',(-8.19963467333826,1.12216314098434,17.4322065225163));
#30926=CARTESIAN_POINT('Ctrl Pts',(-7.58018086668815,-0.797569598526321,
16.1033804324511));
#30927=CARTESIAN_POINT('Ctrl Pts',(-7.45125783945749,-0.648885562185978,
16.1110984060675));
#30928=CARTESIAN_POINT('Ctrl Pts',(-7.26698877156495,-0.287949612261818,
16.1265343533002));
#30929=CARTESIAN_POINT('Ctrl Pts',(-7.27490865362618,0.32007234829603,16.1496882741493));
#30930=CARTESIAN_POINT('Ctrl Pts',(-7.56534886852848,0.854220376402022,
16.1728421949984));
#30931=CARTESIAN_POINT('Ctrl Pts',(-8.07130432124706,1.1914331757699,16.1959961158475));
#30932=CARTESIAN_POINT('Ctrl Pts',(-8.6761167548453,1.25389862909226,16.2191500366966));
#30933=CARTESIAN_POINT('Ctrl Pts',(-9.24031710111236,1.02723652833138,16.2423039575456));
#30934=CARTESIAN_POINT('Ctrl Pts',(-9.6338092170224,0.563701415719523,16.2654578783947));
#30935=CARTESIAN_POINT('Ctrl Pts',(-9.76585693132658,-0.0298154766930449,
16.2886117992438));
#30936=CARTESIAN_POINT('Ctrl Pts',(-9.60601198986148,-0.616457983927628,
16.3117657200929));
#30937=CARTESIAN_POINT('Ctrl Pts',(-9.19113265245436,-1.06095164978761,
16.334919640942));
#30938=CARTESIAN_POINT('Ctrl Pts',(-8.61688568636888,-1.26080157516723,
16.3580735617911));
#30939=CARTESIAN_POINT('Ctrl Pts',(-8.01568613783619,-1.16992431385386,
16.3812274826402));
#30940=CARTESIAN_POINT('Ctrl Pts',(-7.52616409955547,-0.809275278562791,
16.4043814034892));
#30941=CARTESIAN_POINT('Ctrl Pts',(-7.26119801228416,-0.26201616100183,
16.4275353243383));
#30942=CARTESIAN_POINT('Ctrl Pts',(-7.28188617544855,0.345661023092506,
16.4506892451874));
#30943=CARTESIAN_POINT('Ctrl Pts',(-7.58345812161518,0.873632542466389,
16.4738431660365));
#30944=CARTESIAN_POINT('Ctrl Pts',(-8.09637464490968,1.20015390916439,16.4969970868856));
#30945=CARTESIAN_POINT('Ctrl Pts',(-8.7023627797999,1.24993285374973,16.5201510077347));
#30946=CARTESIAN_POINT('Ctrl Pts',(-9.26168826129643,1.01149089264566,16.5433049285838));
#30947=CARTESIAN_POINT('Ctrl Pts',(-9.64537672384094,0.539810146116103,
16.5664588494329));
#30948=CARTESIAN_POINT('Ctrl Pts',(-9.76495378605776,-0.0563449421030929,
16.5896127702819));
#30949=CARTESIAN_POINT('Ctrl Pts',(-9.59284627947019,-0.639507500190754,
16.612766691131));
#30950=CARTESIAN_POINT('Ctrl Pts',(-9.1687403210034,-1.07520659243964,16.6359206119801));
#30951=CARTESIAN_POINT('Ctrl Pts',(-8.59043012652324,-1.26297475254772,
16.6590745328292));
#30952=CARTESIAN_POINT('Ctrl Pts',(-7.99126772957441,-1.15951468743868,
16.6822284536783));
#30953=CARTESIAN_POINT('Ctrl Pts',(-7.50941345452508,-0.788683161530444,
16.7053823745274));
#30954=CARTESIAN_POINT('Ctrl Pts',(-7.2559776502202,-0.235989886660555,
16.7285362953765));
#30955=CARTESIAN_POINT('Ctrl Pts',(-7.28939985343257,0.371120086345011,
16.7516902162256));
#30956=CARTESIAN_POINT('Ctrl Pts',(-7.60197326804091,0.892653808620445,
16.7748441370746));
#30957=CARTESIAN_POINT('Ctrl Pts',(-8.12162186829395,1.20835128286614,16.7979980579237));
#30958=CARTESIAN_POINT('Ctrl Pts',(-8.72852034550391,1.24541610919772,16.8211519787728));
#30959=CARTESIAN_POINT('Ctrl Pts',(-9.28272451943119,0.995301542266061,
16.8443058996219));
#30960=CARTESIAN_POINT('Ctrl Pts',(-9.65644094238201,0.515681277674482,
16.867459820471));
#30961=CARTESIAN_POINT('Ctrl Pts',(-9.76349467666975,-0.0828494742243546,
16.8906137413201));
#30962=CARTESIAN_POINT('Ctrl Pts',(-9.57920029690692,-0.66227603951712,
16.9137676621692));
#30963=CARTESIAN_POINT('Ctrl Pts',(-9.14605408022473,-1.08898896173995,
16.9369215830183));
#30964=CARTESIAN_POINT('Ctrl Pts',(-8.56393482767032,-1.26459288749884,
16.9600755038673));
#30965=CARTESIAN_POINT('Ctrl Pts',(-7.96707289994234,-1.1485954638407,16.9832294247164));
#30966=CARTESIAN_POINT('Ctrl Pts',(-7.49309815860203,-0.767744433222239,
17.0063833455655));
#30967=CARTESIAN_POINT('Ctrl Pts',(-7.25130401707404,-0.209859896869422,
17.0295372664146));
#30968=CARTESIAN_POINT('Ctrl Pts',(-7.29744557308788,0.396416047559612,
17.0526911872637));
#30969=CARTESIAN_POINT('Ctrl Pts',(-7.62088308273839,0.911282765764439,
17.0758451081128));
#30970=CARTESIAN_POINT('Ctrl Pts',(-8.14703538592992,1.21601760624665,17.0989990289619));
#30971=CARTESIAN_POINT('Ctrl Pts',(-8.75457747423087,1.24035201730987,17.122152949811));
#30972=CARTESIAN_POINT('Ctrl Pts',(-9.30341679390951,0.978674783003138,
17.14530687066));
#30973=CARTESIAN_POINT('Ctrl Pts',(-9.66699689558182,0.491325749557319,
17.1684607915091));
#30974=CARTESIAN_POINT('Ctrl Pts',(-9.76148033787767,-0.10931754119764,
17.1916147123582));
#30975=CARTESIAN_POINT('Ctrl Pts',(-9.56507989669121,-0.68475363956845,
17.2147686332073));
#30976=CARTESIAN_POINT('Ctrl Pts',(-9.12308418289996,-1.1022924873685,17.2379225540564));
#30977=CARTESIAN_POINT('Ctrl Pts',(-8.53741084518169,-1.26565584737736,
17.2610764749055));
#30978=CARTESIAN_POINT('Ctrl Pts',(-7.94311359864215,-1.13717035634921,
17.2842303957546));
#30979=CARTESIAN_POINT('Ctrl Pts',(-7.47722268493459,-0.746471406749234,
17.3073843166036));
#30980=CARTESIAN_POINT('Ctrl Pts',(-7.24718561960605,-0.183633649692887,
17.3305382374527));
#30981=CARTESIAN_POINT('Ctrl Pts',(-7.3060079723258,0.421518864292242,17.3536921583018));
#30982=CARTESIAN_POINT('Ctrl Pts',(-7.64021327215519,0.929515170005604,
17.3768460791509));
#30983=CARTESIAN_POINT('Ctrl Pts',(-7.99510874416169,1.12516550422184,17.3922820263836));
#30984=CARTESIAN_POINT('Ctrl Pts',(-8.18521110449555,1.17604951161381,17.4));
#30985=CARTESIAN_POINT('Ctrl Pts',(-8.18521110449555,1.17604951161381,17.4));
#30986=CARTESIAN_POINT('Ctrl Pts',(-8.13719933141137,1.1596386310925,17.4));
#30987=CARTESIAN_POINT('Ctrl Pts',(-8.09039173307286,1.14022110224332,17.4));
#30988=CARTESIAN_POINT('Ctrl Pts',(-8.04502617402981,1.11798780897205,17.4));
#30989=CARTESIAN_POINT('Ctrl Pts',(-7.99968282249027,1.09576539941849,17.4));
#30990=CARTESIAN_POINT('Ctrl Pts',(-7.95577920066712,1.07072928126397,17.4));
#30991=CARTESIAN_POINT('Ctrl Pts',(-7.91358006184999,1.04302582262482,17.4));
#30992=CARTESIAN_POINT('Ctrl Pts',(-7.87480130346833,1.01756782137131,17.4));
#30993=CARTESIAN_POINT('Ctrl Pts',(-7.83746169262404,0.98985647985361,17.4));
#30994=CARTESIAN_POINT('Ctrl Pts',(-7.80179671782517,0.959979848904726,
17.4));
#30995=CARTESIAN_POINT('Ctrl Pts',(-7.79470096127184,0.954035717413182,
17.4));
#30996=CARTESIAN_POINT('Ctrl Pts',(-7.78766995121509,0.948004356872779,
17.4));
#30997=CARTESIAN_POINT('Ctrl Pts',(-7.78071104889818,0.941891074987019,
17.4));
#30998=CARTESIAN_POINT('Ctrl Pts',(-7.75269283864155,0.917277535461247,
17.4));
#30999=CARTESIAN_POINT('Ctrl Pts',(-7.72591217218802,0.89139923448771,17.4));
#31000=CARTESIAN_POINT('Ctrl Pts',(-7.70047050940558,0.864320484202139,
17.4));
#31001=CARTESIAN_POINT('Ctrl Pts',(-7.66652610990813,0.828191873999045,
17.4));
#31002=CARTESIAN_POINT('Ctrl Pts',(-7.63496332880565,0.789926935722668,
17.4));
#31003=CARTESIAN_POINT('Ctrl Pts',(-7.60593193600345,0.749791972759857,
17.4));
#31004=CARTESIAN_POINT('Ctrl Pts',(-7.58573671276234,0.721872728845864,
17.4));
#31005=CARTESIAN_POINT('Ctrl Pts',(-7.56676729894315,0.693047838849524,
17.4));
#31006=CARTESIAN_POINT('Ctrl Pts',(-7.54908781912516,0.6634012006176,17.4));
#31007=CARTESIAN_POINT('Ctrl Pts',(-7.53965707725517,0.647586833036838,
17.4));
#31008=CARTESIAN_POINT('Ctrl Pts',(-7.53059358194979,0.631538581376815,
17.4));
#31009=CARTESIAN_POINT('Ctrl Pts',(-7.52190851593401,0.615268925347433,
17.4));
#31010=CARTESIAN_POINT('Ctrl Pts',(-7.5174887289744,0.606989378200016,17.4));
#31011=CARTESIAN_POINT('Ctrl Pts',(-7.51316696210323,0.598652491346504,
17.4));
#31012=CARTESIAN_POINT('Ctrl Pts',(-7.5089447953144,0.590259903970057,17.4));
#31013=CARTESIAN_POINT('Ctrl Pts',(-7.50442274498419,0.58127122483559,17.4));
#31014=CARTESIAN_POINT('Ctrl Pts',(-7.50001831617906,0.572225198393919,
17.4));
#31015=CARTESIAN_POINT('Ctrl Pts',(-7.49573624060671,0.563131408297169,
17.4));
#31016=CARTESIAN_POINT('Ctrl Pts',(-7.47506504458002,0.51923224899006,17.4));
#31017=CARTESIAN_POINT('Ctrl Pts',(-7.45721461446443,0.474168760407469,
17.4));
#31018=CARTESIAN_POINT('Ctrl Pts',(-7.44233244334752,0.428188460522925,
17.4));
#31019=CARTESIAN_POINT('Ctrl Pts',(-7.43702154871991,0.411779797719997,
17.4));
#31020=CARTESIAN_POINT('Ctrl Pts',(-7.4320891210697,0.395254227754963,17.4));
#31021=CARTESIAN_POINT('Ctrl Pts',(-7.42754343894325,0.378622633207859,
17.4));
#31022=CARTESIAN_POINT('Ctrl Pts',(-7.41562263365724,0.335007176896464,
17.4));
#31023=CARTESIAN_POINT('Ctrl Pts',(-7.40635878862766,0.290662257255706,
17.4));
#31024=CARTESIAN_POINT('Ctrl Pts',(-7.39978211476199,0.24583513299177,17.4));
#31025=CARTESIAN_POINT('Ctrl Pts',(-7.3970185212721,0.22699826327361,17.4));
#31026=CARTESIAN_POINT('Ctrl Pts',(-7.39472989763131,0.208076295947074,
17.4));
#31027=CARTESIAN_POINT('Ctrl Pts',(-7.39292054511252,0.189088017812139,
17.4));
#31028=CARTESIAN_POINT('Ctrl Pts',(-7.39203065715885,0.179749074849041,
17.4));
#31029=CARTESIAN_POINT('Ctrl Pts',(-7.39125658497907,0.170392126906475,
17.4));
#31030=CARTESIAN_POINT('Ctrl Pts',(-7.3905993784452,0.161025711582129,17.4));
#31031=CARTESIAN_POINT('Ctrl Pts',(-7.38726338063351,0.113481538761262,
17.4));
#31032=CARTESIAN_POINT('Ctrl Pts',(-7.38694615050342,0.0658811286412803,
17.4));
#31033=CARTESIAN_POINT('Ctrl Pts',(-7.3896450240632,0.0185133652028824,
17.4));
#31034=CARTESIAN_POINT('Ctrl Pts',(-7.39231331845235,-0.0283177050974028,
17.4));
#31035=CARTESIAN_POINT('Ctrl Pts',(-7.39792993724915,-0.0749224438741415,
17.4));
#31036=CARTESIAN_POINT('Ctrl Pts',(-7.40654177913599,-0.121012609291369,
17.4));
#31037=CARTESIAN_POINT('Ctrl Pts',(-7.40892366435284,-0.133760344920039,
17.4));
#31038=CARTESIAN_POINT('Ctrl Pts',(-7.41153496349064,-0.146468610849955,
17.4));
#31039=CARTESIAN_POINT('Ctrl Pts',(-7.41437732095262,-0.159131017394972,
17.4));
#31040=CARTESIAN_POINT('Ctrl Pts',(-7.41931603486849,-0.181132473668076,
17.4));
#31041=CARTESIAN_POINT('Ctrl Pts',(-7.4249522210655,-0.202995576069695,
17.4));
#31042=CARTESIAN_POINT('Ctrl Pts',(-7.4312759353939,-0.224688518418572,
17.4));
#31043=CARTESIAN_POINT('Ctrl Pts',(-7.43448590379059,-0.235700030918177,
17.4));
#31044=CARTESIAN_POINT('Ctrl Pts',(-7.43787305827033,-0.246667672522508,
17.4));
#31045=CARTESIAN_POINT('Ctrl Pts',(-7.44143629568122,-0.257587102480944,
17.4));
#31046=CARTESIAN_POINT('Ctrl Pts',(-7.4446648798304,-0.267480997951973,
17.4));
#31047=CARTESIAN_POINT('Ctrl Pts',(-7.44803542440217,-0.277327204922127,
17.4));
#31048=CARTESIAN_POINT('Ctrl Pts',(-7.45154495609234,-0.287118681769737,
17.4));
#31049=CARTESIAN_POINT('Ctrl Pts',(-7.46731965368996,-0.331129564115665,
17.4));
#31050=CARTESIAN_POINT('Ctrl Pts',(-7.48590775064078,-0.374064115176777,
17.4));
#31051=CARTESIAN_POINT('Ctrl Pts',(-7.50719055019682,-0.415647717031525,
17.4));
#31052=CARTESIAN_POINT('Ctrl Pts',(-7.51904291434652,-0.438805572300566,
17.4));
#31053=CARTESIAN_POINT('Ctrl Pts',(-7.53173179424408,-0.461543974053204,
17.4));
#31054=CARTESIAN_POINT('Ctrl Pts',(-7.54524198733332,-0.48381081567099,
17.4));
#31055=CARTESIAN_POINT('Ctrl Pts',(-7.55097571485935,-0.493260865855931,
17.4));
#31056=CARTESIAN_POINT('Ctrl Pts',(-7.55685683761236,-0.502624737244181,
17.4));
#31057=CARTESIAN_POINT('Ctrl Pts',(-7.56287734293596,-0.511888319657218,
17.4));
#31058=CARTESIAN_POINT('Ctrl Pts',(-7.58817043839211,-0.550806095100506,
17.4));
#31059=CARTESIAN_POINT('Ctrl Pts',(-7.61595063019034,-0.588007205459175,
17.4));
#31060=CARTESIAN_POINT('Ctrl Pts',(-7.64611656408827,-0.623204427033219,
17.4));
#31061=CARTESIAN_POINT('Ctrl Pts',(-7.66532319320885,-0.645614473515954,
17.4));
#31062=CARTESIAN_POINT('Ctrl Pts',(-7.68549786483987,-0.667211399547439,
17.4));
#31063=CARTESIAN_POINT('Ctrl Pts',(-7.70658083841843,-0.687941007615962,
17.4));
#31064=CARTESIAN_POINT('Ctrl Pts',(-7.70661869325987,-0.687936125025659,
16.2));
#31065=CARTESIAN_POINT('Ctrl Pts',(-7.67409819941258,-0.655901613373747,
16.2));
#31066=CARTESIAN_POINT('Ctrl Pts',(-7.64381371410258,-0.621807353051285,
16.2));
#31067=CARTESIAN_POINT('Ctrl Pts',(-7.61585565959385,-0.585952756227217,
16.2));
#31068=CARTESIAN_POINT('Ctrl Pts',(-7.58749905195372,-0.549587037935981,
16.2));
#31069=CARTESIAN_POINT('Ctrl Pts',(-7.56153494829612,-0.511409649371158,
16.2));
#31070=CARTESIAN_POINT('Ctrl Pts',(-7.53808804236644,-0.471687753089119,
16.2));
#31071=CARTESIAN_POINT('Ctrl Pts',(-7.51732645863979,-0.436515117607317,
16.2));
#31072=CARTESIAN_POINT('Ctrl Pts',(-7.4985386214165,-0.400130432937881,
16.2));
#31073=CARTESIAN_POINT('Ctrl Pts',(-7.48183756845935,-0.362697997620638,
16.2));
#31074=CARTESIAN_POINT('Ctrl Pts',(-7.47711052305992,-0.352103167365936,
16.2));
#31075=CARTESIAN_POINT('Ctrl Pts',(-7.47254949524406,-0.341420594140401,
16.2));
#31076=CARTESIAN_POINT('Ctrl Pts',(-7.46816743540603,-0.330679560210348,
16.2));
#31077=CARTESIAN_POINT('Ctrl Pts',(-7.45706730558176,-0.303471608818189,
16.2));
#31078=CARTESIAN_POINT('Ctrl Pts',(-7.44710097243911,-0.275859205740836,
16.2));
#31079=CARTESIAN_POINT('Ctrl Pts',(-7.43829583898931,-0.247910972255057,
16.2));
#31080=CARTESIAN_POINT('Ctrl Pts',(-7.42417626257798,-0.203094250224204,
16.2));
#31081=CARTESIAN_POINT('Ctrl Pts',(-7.41303986581868,-0.157415105126112,
16.2));
#31082=CARTESIAN_POINT('Ctrl Pts',(-7.40485132275059,-0.111177022987818,
16.2));
#31083=CARTESIAN_POINT('Ctrl Pts',(-7.39906463642413,-0.0785014572068798,
16.2));
#31084=CARTESIAN_POINT('Ctrl Pts',(-7.39475106098134,-0.0455460201930134,
16.2));
#31085=CARTESIAN_POINT('Ctrl Pts',(-7.3919127668216,-0.0124120211671536,
16.2));
#31086=CARTESIAN_POINT('Ctrl Pts',(-7.39015412848058,0.0081181697852479,
16.2));
#31087=CARTESIAN_POINT('Ctrl Pts',(-7.38896211845984,0.0287169905616347,
16.2));
#31088=CARTESIAN_POINT('Ctrl Pts',(-7.38833968108958,0.049360700311489,
16.2));
#31089=CARTESIAN_POINT('Ctrl Pts',(-7.38797753653769,0.0613715585501746,
16.2));
#31090=CARTESIAN_POINT('Ctrl Pts',(-7.38780840935154,0.0734020382686694,
16.2));
#31091=CARTESIAN_POINT('Ctrl Pts',(-7.38783261787483,0.0854186284205357,
16.2));
#31092=CARTESIAN_POINT('Ctrl Pts',(-7.38793000681716,0.133760404211766,
16.2));
#31093=CARTESIAN_POINT('Ctrl Pts',(-7.39114764392613,0.181958557559603,
16.2));
#31094=CARTESIAN_POINT('Ctrl Pts',(-7.3974533166152,0.229702110452317,16.2));
#31095=CARTESIAN_POINT('Ctrl Pts',(-7.39993002168277,0.248454542623161,
16.2));
#31096=CARTESIAN_POINT('Ctrl Pts',(-7.40288366457642,0.267137030119369,
16.2));
#31097=CARTESIAN_POINT('Ctrl Pts',(-7.40631442558066,0.285731222217819,
16.2));
#31098=CARTESIAN_POINT('Ctrl Pts',(-7.41475452038151,0.33147522591313,16.2));
#31099=CARTESIAN_POINT('Ctrl Pts',(-7.42607900308179,0.376685278391262,
16.2));
#31100=CARTESIAN_POINT('Ctrl Pts',(-7.44015772007498,0.42113138571071,16.2));
#31101=CARTESIAN_POINT('Ctrl Pts',(-7.44619795546194,0.440200236258183,
16.2));
#31102=CARTESIAN_POINT('Ctrl Pts',(-7.45274573481429,0.459128399707979,
16.2));
#31103=CARTESIAN_POINT('Ctrl Pts',(-7.45979327769237,0.477897135727449,
16.2));
#31104=CARTESIAN_POINT('Ctrl Pts',(-7.4642421136194,0.489745098705874,16.2));
#31105=CARTESIAN_POINT('Ctrl Pts',(-7.468892265084,0.501534238264903,16.2));
#31106=CARTESIAN_POINT('Ctrl Pts',(-7.47372969293921,0.513231143469178,
16.2));
#31107=CARTESIAN_POINT('Ctrl Pts',(-7.49246801605267,0.55854042677133,16.2));
#31108=CARTESIAN_POINT('Ctrl Pts',(-7.51403710348823,0.602539209890798,
16.2));
#31109=CARTESIAN_POINT('Ctrl Pts',(-7.53825701358138,0.64497355101848,16.2));
#31110=CARTESIAN_POINT('Ctrl Pts',(-7.56269796362399,0.6877951637992,16.2));
#31111=CARTESIAN_POINT('Ctrl Pts',(-7.58983866618497,0.729024731678887,
16.2));
#31112=CARTESIAN_POINT('Ctrl Pts',(-7.61954508460314,0.768389575096334,
16.2));
#31113=CARTESIAN_POINT('Ctrl Pts',(-7.62494291098869,0.775542392627911,
16.2));
#31114=CARTESIAN_POINT('Ctrl Pts',(-7.63042557616055,0.782633586115029,
16.2));
#31115=CARTESIAN_POINT('Ctrl Pts',(-7.63599244107805,0.789661434383682,
16.2));
#31116=CARTESIAN_POINT('Ctrl Pts',(-7.65116980668403,0.808821989593387,
16.2));
#31117=CARTESIAN_POINT('Ctrl Pts',(-7.66697286226321,0.827511837810756,
16.2));
#31118=CARTESIAN_POINT('Ctrl Pts',(-7.68337336577547,0.845710316113916,
16.2));
#31119=CARTESIAN_POINT('Ctrl Pts',(-7.69112549719668,0.854312307837324,
16.2));
#31120=CARTESIAN_POINT('Ctrl Pts',(-7.69901114804083,0.862804487247497,
16.2));
#31121=CARTESIAN_POINT('Ctrl Pts',(-7.70702751694813,0.871184505187608,
16.2));
#31122=CARTESIAN_POINT('Ctrl Pts',(-7.71445522191538,0.878949155442497,
16.2));
#31123=CARTESIAN_POINT('Ctrl Pts',(-7.72198944448574,0.886611472889222,
16.2));
#31124=CARTESIAN_POINT('Ctrl Pts',(-7.72962359681997,0.894166271565807,
16.2));
#31125=CARTESIAN_POINT('Ctrl Pts',(-7.76528162277488,0.929453648015724,
16.2));
#31126=CARTESIAN_POINT('Ctrl Pts',(-7.80314159744981,0.962424156726079,
16.2));
#31127=CARTESIAN_POINT('Ctrl Pts',(-7.8429321675271,0.99292226510897,16.2));
#31128=CARTESIAN_POINT('Ctrl Pts',(-7.86517997576319,1.00997444771274,16.2));
#31129=CARTESIAN_POINT('Ctrl Pts',(-7.8880321474545,1.02625321846037,16.2));
#31130=CARTESIAN_POINT('Ctrl Pts',(-7.9114465947083,1.04172678059142,16.2));
#31131=CARTESIAN_POINT('Ctrl Pts',(-7.92363396469123,1.04978086893273,16.2));
#31132=CARTESIAN_POINT('Ctrl Pts',(-7.93597595875067,1.05761787570908,16.2));
#31133=CARTESIAN_POINT('Ctrl Pts',(-7.94844653765927,1.06522111773372,16.2));
#31134=CARTESIAN_POINT('Ctrl Pts',(-7.99400655072966,1.09299880219879,16.2));
#31135=CARTESIAN_POINT('Ctrl Pts',(-8.04133366721399,1.11769730011503,16.2));
#31136=CARTESIAN_POINT('Ctrl Pts',(-8.09012860071083,1.13911605908712,16.2));
#31137=CARTESIAN_POINT('Ctrl Pts',(-8.12124378896121,1.15277421311553,16.2));
#31138=CARTESIAN_POINT('Ctrl Pts',(-8.15295679384449,1.16509791067328,16.2));
#31139=CARTESIAN_POINT('Ctrl Pts',(-8.18517792975413,1.17607879646049,16.2));
#31140=CARTESIAN_POINT('Ctrl Pts',(-9.55016499124735,-1.36965953006496E-5,
16.6841069671524));
#31141=CARTESIAN_POINT('Ctrl Pts',(-9.55006230523617,0.154119242885846,
16.6770974504288));
#31142=CARTESIAN_POINT('Ctrl Pts',(-9.51567286587192,0.308296531891891,
16.6700879337053));
#31143=CARTESIAN_POINT('Ctrl Pts',(-9.4499660772856,0.447714115625669,16.6630784169817));
#31144=CARTESIAN_POINT('Ctrl Pts',(-9.37761825635498,0.601222734743451,
16.6553604433654));
#31145=CARTESIAN_POINT('Ctrl Pts',(-9.26730263640673,0.736837325878114,
16.647642469749));
#31146=CARTESIAN_POINT('Ctrl Pts',(-9.13173800779262,0.838922265066044,
16.6399244961327));
#31147=CARTESIAN_POINT('Ctrl Pts',(-8.99617337917851,0.941007204253974,
16.6322065225163));
#31148=CARTESIAN_POINT('Ctrl Pts',(-8.83535974189854,1.00956249149517,16.6244885488999));
#31149=CARTESIAN_POINT('Ctrl Pts',(-8.66783803278417,1.03668407535848,16.6167705752836));
#31150=CARTESIAN_POINT('Ctrl Pts',(-8.5003163236698,1.06380565922179,16.6090526016672));
#31151=CARTESIAN_POINT('Ctrl Pts',(-8.32608654272104,1.04949353970721,16.6013346280508));
#31152=CARTESIAN_POINT('Ctrl Pts',(-8.16523643504245,0.995397826415959,
16.5936166544345));
#31153=CARTESIAN_POINT('Ctrl Pts',(-8.00438632736387,0.941302113124703,
16.5858986808181));
#31154=CARTESIAN_POINT('Ctrl Pts',(-7.85691589295546,0.847422806056768,
16.5781807072018));
#31155=CARTESIAN_POINT('Ctrl Pts',(-7.73982767006045,0.724583677870246,
16.5704627335854));
#31156=CARTESIAN_POINT('Ctrl Pts',(-7.62273944716545,0.601744549683724,
16.562744759969));
#31157=CARTESIAN_POINT('Ctrl Pts',(-7.53603343578385,0.449945600378615,
16.5550267863527));
#31158=CARTESIAN_POINT('Ctrl Pts',(-7.4897063667997,0.286688423011718,16.5473088127363));
#31159=CARTESIAN_POINT('Ctrl Pts',(-7.44337929781555,0.12343124564482,16.5395908391199));
#31160=CARTESIAN_POINT('Ctrl Pts',(-7.43743117122886,-0.0512841597838649,
16.5318728655036));
#31161=CARTESIAN_POINT('Ctrl Pts',(-7.47254777397841,-0.217314059761718,
16.5241548918872));
#31162=CARTESIAN_POINT('Ctrl Pts',(-7.50766437672797,-0.383343959739573,
16.5164369182709));
#31163=CARTESIAN_POINT('Ctrl Pts',(-7.58384570881378,-0.540688354266594,
16.5087189446545));
#31164=CARTESIAN_POINT('Ctrl Pts',(-7.69230847670872,-0.67120628810507,
16.5010009710381));
#31165=CARTESIAN_POINT('Ctrl Pts',(-7.80077124460366,-0.801724221943545,
16.4932829974218));
#31166=CARTESIAN_POINT('Ctrl Pts',(-7.94151544830774,-0.905415695093475,
16.4855650238054));
#31167=CARTESIAN_POINT('Ctrl Pts',(-8.09831404897755,-0.970325652253155,
16.477847050189));
#31168=CARTESIAN_POINT('Ctrl Pts',(-8.25511264964736,-1.03523560941283,
16.4701290765727));
#31169=CARTESIAN_POINT('Ctrl Pts',(-8.4279656472829,-1.06136405058227,16.4624111029563));
#31170=CARTESIAN_POINT('Ctrl Pts',(-8.59694402900981,-1.04569849353872,
16.45469312934));
#31171=CARTESIAN_POINT('Ctrl Pts',(-8.76592241073672,-1.03003293649518,
16.4469751557236));
#31172=CARTESIAN_POINT('Ctrl Pts',(-8.93102617655499,-0.972573381238667,
16.4392571821072));
#31173=CARTESIAN_POINT('Ctrl Pts',(-9.07321976852969,-0.879944634656233,
16.4315392084909));
#31174=CARTESIAN_POINT('Ctrl Pts',(-9.21541336050439,-0.7873158880738,16.4238212348745));
#31175=CARTESIAN_POINT('Ctrl Pts',(-9.33469677863551,-0.659517950165448,
16.4161032612582));
#31176=CARTESIAN_POINT('Ctrl Pts',(-9.41731727848406,-0.511285155476193,
16.4083852876418));
#31177=CARTESIAN_POINT('Ctrl Pts',(-9.49993777833262,-0.363052360786937,
16.4006673140254));
#31178=CARTESIAN_POINT('Ctrl Pts',(-9.54589535989859,-0.194384709316778,
16.3929493404091));
#31179=CARTESIAN_POINT('Ctrl Pts',(-9.54989139919407,-0.0247288185109309,
16.3852313667927));
#31180=CARTESIAN_POINT('Ctrl Pts',(-9.55008545467072,-0.0164899969375102,
16.3848565669126));
#31181=CARTESIAN_POINT('Ctrl Pts',(-9.55018055377881,-0.00824884483545272,
16.3844817670325));
#31182=CARTESIAN_POINT('Ctrl Pts',(-9.55017719779692,-7.61530804432864E-6,
16.3841069671524));
#31183=CARTESIAN_POINT('Ctrl Pts',(-8.81478889550445,1.17604951161381,16.2));
#31184=CARTESIAN_POINT('Ctrl Pts',(-9.00489125583831,1.12516550422184,16.2077179736164));
#31185=CARTESIAN_POINT('Ctrl Pts',(-9.35978667802179,0.929514905730451,
16.2231539208491));
#31186=CARTESIAN_POINT('Ctrl Pts',(-9.69399203697644,0.421518824488713,
16.2463078416982));
#31187=CARTESIAN_POINT('Ctrl Pts',(-9.75281439556121,-0.18363371105277,
16.2694617625473));
#31188=CARTESIAN_POINT('Ctrl Pts',(-9.52277733259636,-0.746471423726082,
16.2926156833963));
#31189=CARTESIAN_POINT('Ctrl Pts',(-9.05688641176464,-1.13717038838356,
16.3157696042454));
#31190=CARTESIAN_POINT('Ctrl Pts',(-8.46258915349396,-1.26565587137657,
16.3389235250945));
#31191=CARTESIAN_POINT('Ctrl Pts',(-7.87691580481983,-1.10229251092252,
16.3620774459436));
#31192=CARTESIAN_POINT('Ctrl Pts',(-7.43492008199845,-0.684753652714294,
16.3852313667927));
#31193=CARTESIAN_POINT('Ctrl Pts',(-7.23851963711968,-0.109317543695422,
16.4083852876418));
#31194=CARTESIAN_POINT('Ctrl Pts',(-7.33300308119116,0.491325759444495,
16.4315392084909));
#31195=CARTESIAN_POINT('Ctrl Pts',(-7.69658319014803,0.978674802377791,
16.45469312934));
#31196=CARTESIAN_POINT('Ctrl Pts',(-8.24542252070005,1.24035204198393,16.477847050189));
#31197=CARTESIAN_POINT('Ctrl Pts',(-8.85296462108838,1.21601763039105,16.5010009710381));
#31198=CARTESIAN_POINT('Ctrl Pts',(-9.37911693472505,0.911282783877038,
16.5241548918872));
#31199=CARTESIAN_POINT('Ctrl Pts',(-9.702554450806,0.396416055432127,16.5473088127363));
#31200=CARTESIAN_POINT('Ctrl Pts',(-9.74869600773439,-0.209859901037287,
16.5704627335854));
#31201=CARTESIAN_POINT('Ctrl Pts',(-9.50690186140351,-0.767744448476627,
16.5936166544345));
#31202=CARTESIAN_POINT('Ctrl Pts',(-9.0329271106457,-1.14859548666069,16.6167705752836));
#31203=CARTESIAN_POINT('Ctrl Pts',(-8.4360651710595,-1.26459291262403,16.6399244961327));
#31204=CARTESIAN_POINT('Ctrl Pts',(-7.85394590693938,-1.08898898337596,
16.6630784169817));
#31205=CARTESIAN_POINT('Ctrl Pts',(-7.42079968165148,-0.662276052675294,
16.6862323378308));
#31206=CARTESIAN_POINT('Ctrl Pts',(-7.23650529822705,-0.0828494758703863,
16.7093862586799));
#31207=CARTESIAN_POINT('Ctrl Pts',(-7.34355903464176,0.515681287920065,
16.732540179529));
#31208=CARTESIAN_POINT('Ctrl Pts',(-7.71727546501759,0.995301562040781,
16.7556941003781));
#31209=CARTESIAN_POINT('Ctrl Pts',(-8.27147964995585,1.24541613394172,16.7788480212272));
#31210=CARTESIAN_POINT('Ctrl Pts',(-8.8783781392237,1.20835130687373,16.8020019420763));
#31211=CARTESIAN_POINT('Ctrl Pts',(-9.39802674980115,0.892653826355733,
16.8251558629254));
#31212=CARTESIAN_POINT('Ctrl Pts',(-9.71060017061972,0.371120093718434,
16.8483097837744));
#31213=CARTESIAN_POINT('Ctrl Pts',(-9.74402237449611,-0.235989891349228,
16.8714637046235));
#31214=CARTESIAN_POINT('Ctrl Pts',(-9.49058656515595,-0.788683177200059,
16.8946176254726));
#31215=CARTESIAN_POINT('Ctrl Pts',(-9.0087322805331,-1.15951471047599,16.9177715463217));
#31216=CARTESIAN_POINT('Ctrl Pts',(-8.40956987168007,-1.26297477764059,
16.9409254671708));
#31217=CARTESIAN_POINT('Ctrl Pts',(-7.83125966571002,-1.07520661380189,
16.9640793880199));
#31218=CARTESIAN_POINT('Ctrl Pts',(-7.40715369881707,-0.639507512896534,
16.987233308869));
#31219=CARTESIAN_POINT('Ctrl Pts',(-7.23504618881006,-0.0563449432224961,
17.010387229718));
#31220=CARTESIAN_POINT('Ctrl Pts',(-7.35462325340267,0.539810156841002,
17.0335411505671));
#31221=CARTESIAN_POINT('Ctrl Pts',(-7.73831172357029,1.01149091274223,17.0566950714162));
#31222=CARTESIAN_POINT('Ctrl Pts',(-8.29763721617962,1.24993287858306,17.0798489922653));
#31223=CARTESIAN_POINT('Ctrl Pts',(-8.90362536310944,1.20015393300998,17.1030029131144));
#31224=CARTESIAN_POINT('Ctrl Pts',(-9.41654189659505,0.873632559821981,
17.1261568339635));
#31225=CARTESIAN_POINT('Ctrl Pts',(-9.71811384875226,0.34566102996382,17.1493107548126));
#31226=CARTESIAN_POINT('Ctrl Pts',(-9.73880201233004,-0.262016166215173,
17.1724646756617));
#31227=CARTESIAN_POINT('Ctrl Pts',(-9.47383591978867,-0.809275294625564,
17.1956185965107));
#31228=CARTESIAN_POINT('Ctrl Pts',(-8.98431387179416,-1.16992433712962,
17.2187725173598));
#31229=CARTESIAN_POINT('Ctrl Pts',(-8.38311431128619,-1.26080160014802,
17.2419264382089));
#31230=CARTESIAN_POINT('Ctrl Pts',(-7.80886733385048,-1.06095167099359,
17.265080359058));
#31231=CARTESIAN_POINT('Ctrl Pts',(-7.39398798803169,-0.616457995871644,
17.2882342799071));
#31232=CARTESIAN_POINT('Ctrl Pts',(-7.23414304365684,-0.0298154777491022,
17.3113882007562));
#31233=CARTESIAN_POINT('Ctrl Pts',(-7.36619075960647,0.563701428344329,
17.3345421216053));
#31234=CARTESIAN_POINT('Ctrl Pts',(-7.75968288434054,1.02723654746506,17.3576960424544));
#31235=CARTESIAN_POINT('Ctrl Pts',(-8.32388323581996,1.25389866145525,17.3808499633034));
#31236=CARTESIAN_POINT('Ctrl Pts',(-8.92869568375729,1.19143319965512,17.4040038841525));
#31237=CARTESIAN_POINT('Ctrl Pts',(-9.43465110964391,0.854220435720086,
17.4271578050016));
#31238=CARTESIAN_POINT('Ctrl Pts',(-9.72509133177006,0.320072386474311,
17.4503117258507));
#31239=CARTESIAN_POINT('Ctrl Pts',(-9.73301103905973,-0.287949421315032,
17.4734656466998));
#31240=CARTESIAN_POINT('Ctrl Pts',(-9.54874216054249,-0.648885562185997,
17.4889015939325));
#31241=CARTESIAN_POINT('Ctrl Pts',(-9.41981913331184,-0.797569598526339,
17.4966195675489));
#31242=CARTESIAN_POINT('Ctrl Pts',(-8.80036532666174,1.12216314098434,16.1677934774837));
#31243=CARTESIAN_POINT('Ctrl Pts',(-8.9817572320825,1.0736106293792,16.1755114511001));
#31244=CARTESIAN_POINT('Ctrl Pts',(-9.32039141180499,0.886924705044866,
16.1909473983328));
#31245=CARTESIAN_POINT('Ctrl Pts',(-9.63928354316068,0.402204910083416,
16.2141013191819));
#31246=CARTESIAN_POINT('Ctrl Pts',(-9.69541067217841,-0.175219648450697,
16.237255240031));
#31247=CARTESIAN_POINT('Ctrl Pts',(-9.47591386479892,-0.712268241456979,
16.26040916088));
#31248=CARTESIAN_POINT('Ctrl Pts',(-9.03136997960212,-1.08506545197385,
16.2835630817291));
#31249=CARTESIAN_POINT('Ctrl Pts',(-8.46430331154639,-1.20766375395221,
16.3067170025782));
#31250=CARTESIAN_POINT('Ctrl Pts',(-7.90546540714803,-1.05178567239311,
16.3298709234273));
#31251=CARTESIAN_POINT('Ctrl Pts',(-7.48372184641795,-0.653378367272938,
16.3530248442764));
#31252=CARTESIAN_POINT('Ctrl Pts',(-7.29632043351871,-0.10430863410641,
16.3761787651255));
#31253=CARTESIAN_POINT('Ctrl Pts',(-7.38647466369631,0.468813304218946,
16.3993326859746));
#31254=CARTESIAN_POINT('Ctrl Pts',(-7.73339559945402,0.93383210434011,16.4224866068237));
#31255=CARTESIAN_POINT('Ctrl Pts',(-8.25708721361307,1.18351934133202,16.4456405276728));
#31256=CARTESIAN_POINT('Ctrl Pts',(-8.83679184757567,1.1602999279677,16.4687944485218));
#31257=CARTESIAN_POINT('Ctrl Pts',(-9.33883595972916,0.869527975635269,
16.4919483693709));
#31258=CARTESIAN_POINT('Ctrl Pts',(-9.6474536287757,0.378252345251951,16.51510229022));
#31259=CARTESIAN_POINT('Ctrl Pts',(-9.69148098811842,-0.200244159271414,
16.5382562110691));
#31260=CARTESIAN_POINT('Ctrl Pts',(-9.46076580475344,-0.732566540156623,
16.5614101319182));
#31261=CARTESIAN_POINT('Ctrl Pts',(-9.00850848921934,-1.09596705436568,
16.5845640527673));
#31262=CARTESIAN_POINT('Ctrl Pts',(-8.43899465307059,-1.20664949977268,
16.6077179736164));
#31263=CARTESIAN_POINT('Ctrl Pts',(-7.88354798573076,-1.03909171001279,
16.6308718944654));
#31264=CARTESIAN_POINT('Ctrl Pts',(-7.47024844019752,-0.631930686701274,
16.6540258153145));
#31265=CARTESIAN_POINT('Ctrl Pts',(-7.29439839126077,-0.0790533282429932,
16.6771797361636));
#31266=CARTESIAN_POINT('Ctrl Pts',(-7.39654694531645,0.492052866894308,
16.7003336570127));
#31267=CARTESIAN_POINT('Ctrl Pts',(-7.75313975812458,0.949697028957279,
16.7234875778618));
#31268=CARTESIAN_POINT('Ctrl Pts',(-8.28195041003631,1.18835139753498,16.7466414987109));
#31269=CARTESIAN_POINT('Ctrl Pts',(-8.86104092302068,1.15298487397291,16.76979541956));
#31270=CARTESIAN_POINT('Ctrl Pts',(-9.3568793305836,0.851752593494524,16.7929493404091));
#31271=CARTESIAN_POINT('Ctrl Pts',(-9.6551306951989,0.354115439815118,16.8161032612581));
#31272=CARTESIAN_POINT('Ctrl Pts',(-9.68702149988882,-0.225176878270719,
16.8392571821072));
#31273=CARTESIAN_POINT('Ctrl Pts',(-9.44519807235574,-0.752545860211153,
16.8624111029563));
#31274=CARTESIAN_POINT('Ctrl Pts',(-8.98542226173774,-1.10638596136976,
16.8855650238054));
#31275=CARTESIAN_POINT('Ctrl Pts',(-8.41371336339756,-1.20510550743424,
16.9087189446545));
#31276=CARTESIAN_POINT('Ctrl Pts',(-7.8619012238694,-1.0259408460579,16.9318728655036));
#31277=CARTESIAN_POINT('Ctrl Pts',(-7.45722771376716,-0.610205397194798,
16.9550267863527));
#31278=CARTESIAN_POINT('Ctrl Pts',(-7.2930061379668,-0.0537632283681462,
16.9781807072018));
#31279=CARTESIAN_POINT('Ctrl Pts',(-7.4071042036246,0.515076155513817,17.0013346280508));
#31280=CARTESIAN_POINT('Ctrl Pts',(-7.77321213920967,0.965144586610446,
17.0244885488999));
#31281=CARTESIAN_POINT('Ctrl Pts',(-8.30690944142428,1.19266118577408,17.047642469749));
#31282=CARTESIAN_POINT('Ctrl Pts',(-8.88513132378781,1.14516310226012,17.0707963905981));
#31283=CARTESIAN_POINT('Ctrl Pts',(-9.37454611678337,0.833602877867565,
17.0939503114472));
#31284=CARTESIAN_POINT('Ctrl Pts',(-9.66230009799215,0.329822905642644,
17.1171042322963));
#31285=CARTESIAN_POINT('Ctrl Pts',(-9.68204033374956,-0.250010634046539,
17.1402581531454));
#31286=CARTESIAN_POINT('Ctrl Pts',(-9.42921493845428,-0.772194450633179,
17.1634120739945));
#31287=CARTESIAN_POINT('Ctrl Pts',(-8.96212269996102,-1.11631862085965,
17.1865659948435));
#31288=CARTESIAN_POINT('Ctrl Pts',(-8.38846999187711,-1.20303190453157,
17.2097199156926));
#31289=CARTESIAN_POINT('Ctrl Pts',(-7.84053490450502,-1.01233906208678,
17.2328738365417));
#31290=CARTESIAN_POINT('Ctrl Pts',(-7.44466525340957,-0.588212004767528,
17.2560277573908));
#31291=CARTESIAN_POINT('Ctrl Pts',(-7.2921443747571,-0.0284493380852384,
17.2791816782399));
#31292=CARTESIAN_POINT('Ctrl Pts',(-7.4181416888383,0.537872733385351,17.302335599089));
#31293=CARTESIAN_POINT('Ctrl Pts',(-7.79360407735479,0.980168759268893,
17.3254895199381));
#31294=CARTESIAN_POINT('Ctrl Pts',(-8.33195287330967,1.19644525721016,17.3486434407872));
#31295=CARTESIAN_POINT('Ctrl Pts',(-8.90905292699061,1.13684195129112,17.3717973616362));
#31296=CARTESIAN_POINT('Ctrl Pts',(-9.39182556904706,0.815080213693786,
17.3949512824853));
#31297=CARTESIAN_POINT('Ctrl Pts',(-9.66895787403142,0.305406729054712,
17.4181052033344));
#31298=CARTESIAN_POINT('Ctrl Pts',(-9.67651470180108,-0.274755632204714,
17.4412591241835));
#31299=CARTESIAN_POINT('Ctrl Pts',(-9.5006889891414,-0.619153746004135,
17.4566950714162));
#31300=CARTESIAN_POINT('Ctrl Pts',(-9.37767319112126,-0.761025107359451,
17.4644130450326));
#31301=CARTESIAN_POINT('Ctrl Pts',(-8.78594175781903,1.06827677035486,16.1355869549674));
#31302=CARTESIAN_POINT('Ctrl Pts',(-8.95862320832669,1.02205575453656,16.1433049285838));
#31303=CARTESIAN_POINT('Ctrl Pts',(-9.28099614558818,0.844334504359283,
16.1587408758165));
#31304=CARTESIAN_POINT('Ctrl Pts',(-9.58457504934491,0.382890995678119,
16.1818947966656));
#31305=CARTESIAN_POINT('Ctrl Pts',(-9.63800694879561,-0.166805585848624,
16.2050487175147));
#31306=CARTESIAN_POINT('Ctrl Pts',(-9.42905039700147,-0.678065059187875,
16.2282026383638));
#31307=CARTESIAN_POINT('Ctrl Pts',(-9.00585354743959,-1.03296051556415,
16.2513565592128));
#31308=CARTESIAN_POINT('Ctrl Pts',(-8.46601746959882,-1.14967163652785,
16.2745104800619));
#31309=CARTESIAN_POINT('Ctrl Pts',(-7.93401500947623,-1.0012788338637,16.297664400911));
#31310=CARTESIAN_POINT('Ctrl Pts',(-7.53252361083745,-0.622003081831582,
16.3208183217601));
#31311=CARTESIAN_POINT('Ctrl Pts',(-7.35412122991775,-0.0992997245173969,
16.3439722426092));
#31312=CARTESIAN_POINT('Ctrl Pts',(-7.43994624620145,0.446300848993395,
16.3671261634583));
#31313=CARTESIAN_POINT('Ctrl Pts',(-7.77020800876001,0.888989406302429,
16.3902800843074));
#31314=CARTESIAN_POINT('Ctrl Pts',(-8.26875190652608,1.12668664068011,16.4134340051565));
#31315=CARTESIAN_POINT('Ctrl Pts',(-8.82061907406296,1.10458222554434,16.4365879260055));
#31316=CARTESIAN_POINT('Ctrl Pts',(-9.29855498473327,0.8277731673935,16.4597418468546));
#31317=CARTESIAN_POINT('Ctrl Pts',(-9.59235280674539,0.360088635071775,
16.4828957677037));
#31318=CARTESIAN_POINT('Ctrl Pts',(-9.63426596850247,-0.190628417505539,
16.5060496885528));
#31319=CARTESIAN_POINT('Ctrl Pts',(-9.41462974810337,-0.697388631836621,
16.5292036094019));
#31320=CARTESIAN_POINT('Ctrl Pts',(-8.98408986779299,-1.04333862207067,
16.552357530251));
#31321=CARTESIAN_POINT('Ctrl Pts',(-8.44192413508167,-1.14870608692133,
16.5755114511001));
#31322=CARTESIAN_POINT('Ctrl Pts',(-7.91315006452214,-0.989194436649623,
16.5986653719491));
#31323=CARTESIAN_POINT('Ctrl Pts',(-7.51969719874356,-0.601585320727254,
16.6218192927982));
#31324=CARTESIAN_POINT('Ctrl Pts',(-7.35229148429449,-0.0752571806156001,
16.6449732136473));
#31325=CARTESIAN_POINT('Ctrl Pts',(-7.44953485599114,0.468424445868551,
16.6681271344964));
#31326=CARTESIAN_POINT('Ctrl Pts',(-7.78900405123157,0.904092495873778,
16.6912810553455));
#31327=CARTESIAN_POINT('Ctrl Pts',(-8.29242117011678,1.13128666112824,16.7144349761946));
#31328=CARTESIAN_POINT('Ctrl Pts',(-8.84370370681767,1.09761844107208,16.7375888970437));
#31329=CARTESIAN_POINT('Ctrl Pts',(-9.31573191136605,0.810851360633317,
16.7607428178928));
#31330=CARTESIAN_POINT('Ctrl Pts',(-9.59966121977809,0.3371107859118,16.7838967387418));
#31331=CARTESIAN_POINT('Ctrl Pts',(-9.63002062528153,-0.21436386519221,
16.8070506595909));
#31332=CARTESIAN_POINT('Ctrl Pts',(-9.39980957955552,-0.716408543222247,
16.83020458044));
#31333=CARTESIAN_POINT('Ctrl Pts',(-8.96211224294239,-1.05325721226352,
16.8533585012891));
#31334=CARTESIAN_POINT('Ctrl Pts',(-8.41785685511504,-1.14723623722789,
16.8765124221382));
#31335=CARTESIAN_POINT('Ctrl Pts',(-7.89254278202879,-0.976675078313916,
16.8996663429873));
#31336=CARTESIAN_POINT('Ctrl Pts',(-7.50730172871725,-0.580903281493062,
16.9228202638364));
#31337=CARTESIAN_POINT('Ctrl Pts',(-7.35096608712355,-0.0511815135137962,
16.9459741846855));
#31338=CARTESIAN_POINT('Ctrl Pts',(-7.45958515384652,0.490342154186633,
16.9691281055345));
#31339=CARTESIAN_POINT('Ctrl Pts',(-7.80811255484906,0.918798260478664,
16.9922820263836));
#31340=CARTESIAN_POINT('Ctrl Pts',(-8.31618166666894,1.1353894929651,17.0154359472327));
#31341=CARTESIAN_POINT('Ctrl Pts',(-8.86663728446618,1.09017227151027,17.0385898680818));
#31342=CARTESIAN_POINT('Ctrl Pts',(-9.3325503369717,0.793573195913151,17.0617437889309));
#31343=CARTESIAN_POINT('Ctrl Pts',(-9.60648634723204,0.313984781321469,
17.08489770978));
#31344=CARTESIAN_POINT('Ctrl Pts',(-9.62527865516907,-0.238005101877905,
17.1080516306291));
#31345=CARTESIAN_POINT('Ctrl Pts',(-9.3845939571199,-0.735113606640794,
17.1312055514782));
#31346=CARTESIAN_POINT('Ctrl Pts',(-8.93993152812788,-1.06271290458967,
17.1543594723272));
#31347=CARTESIAN_POINT('Ctrl Pts',(-8.39382567246804,-1.14526220891511,
17.1775133931763));
#31348=CARTESIAN_POINT('Ctrl Pts',(-7.87220247515956,-0.963726453179972,
17.2006673140254));
#31349=CARTESIAN_POINT('Ctrl Pts',(-7.49534251878745,-0.559966013663411,
17.2238212348745));
#31350=CARTESIAN_POINT('Ctrl Pts',(-7.35014570585736,-0.0270831984213753,
17.2469751557236));
#31351=CARTESIAN_POINT('Ctrl Pts',(-7.47009261807012,0.512044038426373,
17.2701290765727));
#31352=CARTESIAN_POINT('Ctrl Pts',(-7.82752527036905,0.933100971072724,
17.2932829974218));
#31353=CARTESIAN_POINT('Ctrl Pts',(-8.34002251079937,1.13899185296508,17.3164369182709));
#31354=CARTESIAN_POINT('Ctrl Pts',(-8.88941017022393,1.08225070292711,17.3395908391199));
#31355=CARTESIAN_POINT('Ctrl Pts',(-9.34900002845021,0.775939991667486,
17.362744759969));
#31356=CARTESIAN_POINT('Ctrl Pts',(-9.61282441629278,0.290741071635111,
17.3858986808181));
#31357=CARTESIAN_POINT('Ctrl Pts',(-9.62001836454243,-0.261561843094395,
17.4090526016672));
#31358=CARTESIAN_POINT('Ctrl Pts',(-9.4526358177403,-0.589421929822272,
17.4244885488999));
#31359=CARTESIAN_POINT('Ctrl Pts',(-9.33552724893069,-0.724480616192563,
17.4322065225163));
#31360=CARTESIAN_POINT('Ctrl Pts',(-8.77151818897632,1.01439039972538,16.1033804324511));
#31361=CARTESIAN_POINT('Ctrl Pts',(-8.93548918457087,0.970500879693913,
16.1110984060675));
#31362=CARTESIAN_POINT('Ctrl Pts',(-9.24160087937137,0.8017443036737,16.1265343533002));
#31363=CARTESIAN_POINT('Ctrl Pts',(-9.52986655552915,0.363577081272822,
16.1496882741493));
#31364=CARTESIAN_POINT('Ctrl Pts',(-9.58060322541281,-0.158391523246551,
16.1728421949984));
#31365=CARTESIAN_POINT('Ctrl Pts',(-9.38218692920402,-0.643861876918772,
16.1959961158475));
#31366=CARTESIAN_POINT('Ctrl Pts',(-8.98033711527706,-0.980855579154441,
16.2191500366966));
#31367=CARTESIAN_POINT('Ctrl Pts',(-8.46773162765124,-1.09167951910348,
16.2423039575456));
#31368=CARTESIAN_POINT('Ctrl Pts',(-7.96256461180444,-0.950771995334296,
16.2654578783947));
#31369=CARTESIAN_POINT('Ctrl Pts',(-7.58132537525694,-0.590627796390225,
16.2886117992438));
#31370=CARTESIAN_POINT('Ctrl Pts',(-7.41192202631679,-0.0942908149283849,
16.3117657200929));
#31371=CARTESIAN_POINT('Ctrl Pts',(-7.49341782870659,0.423788393767846,
16.334919640942));
#31372=CARTESIAN_POINT('Ctrl Pts',(-7.807020418066,0.844146708264748,16.3580735617911));
#31373=CARTESIAN_POINT('Ctrl Pts',(-8.28041659943909,1.0698539400282,16.3812274826402));
#31374=CARTESIAN_POINT('Ctrl Pts',(-8.80444630055025,1.04886452312099,16.4043814034892));
#31375=CARTESIAN_POINT('Ctrl Pts',(-9.25827400973738,0.786018359151732,
16.4275353243383));
#31376=CARTESIAN_POINT('Ctrl Pts',(-9.53725198471509,0.341924924891599,
16.4506892451874));
#31377=CARTESIAN_POINT('Ctrl Pts',(-9.57705094888651,-0.181012675739665,
16.4738431660365));
#31378=CARTESIAN_POINT('Ctrl Pts',(-9.36849369145331,-0.662210723516617,
16.4969970868856));
#31379=CARTESIAN_POINT('Ctrl Pts',(-8.95967124636663,-0.990710189775668,
16.5201510077347));
#31380=CARTESIAN_POINT('Ctrl Pts',(-8.44485361709276,-1.09076267406997,
16.5433049285838));
#31381=CARTESIAN_POINT('Ctrl Pts',(-7.94275214331352,-0.939297163286455,
16.5664588494329));
#31382=CARTESIAN_POINT('Ctrl Pts',(-7.5691459572896,-0.571239954753235,
16.5896127702819));
#31383=CARTESIAN_POINT('Ctrl Pts',(-7.41018457732821,-0.071461032988207,
16.612766691131));
#31384=CARTESIAN_POINT('Ctrl Pts',(-7.50252276666583,0.444796024842794,
16.6359206119801));
#31385=CARTESIAN_POINT('Ctrl Pts',(-7.82486834433855,0.858487962790278,
16.6590745328292));
#31386=CARTESIAN_POINT('Ctrl Pts',(-8.30289193019724,1.0742219247215,16.6822284536783));
#31387=CARTESIAN_POINT('Ctrl Pts',(-8.82636649061465,1.04225200817126,16.7053823745274));
#31388=CARTESIAN_POINT('Ctrl Pts',(-9.2745844921485,0.769950127772109,16.7285362953765));
#31389=CARTESIAN_POINT('Ctrl Pts',(-9.54419174435727,0.320106132008483,
16.7516902162256));
#31390=CARTESIAN_POINT('Ctrl Pts',(-9.57301975067424,-0.2035508521137,16.7748441370746));
#31391=CARTESIAN_POINT('Ctrl Pts',(-9.35442108675531,-0.680271226233341,
16.7979980579237));
#31392=CARTESIAN_POINT('Ctrl Pts',(-8.93880222414703,-1.00012846315729,
16.8211519787728));
#31393=CARTESIAN_POINT('Ctrl Pts',(-8.42200034683252,-1.08936696702154,
16.8443058996219));
#31394=CARTESIAN_POINT('Ctrl Pts',(-7.92318434018817,-0.92740931056993,
16.867459820471));
#31395=CARTESIAN_POINT('Ctrl Pts',(-7.55737574366735,-0.551601165791326,
16.8906137413201));
#31396=CARTESIAN_POINT('Ctrl Pts',(-7.40892603628029,-0.0485997986594464,
16.9137676621692));
#31397=CARTESIAN_POINT('Ctrl Pts',(-7.51206610406846,0.465608152859449,
16.9369215830182));
#31398=CARTESIAN_POINT('Ctrl Pts',(-7.84301297048845,0.872451934346883,
16.9600755038674));
#31399=CARTESIAN_POINT('Ctrl Pts',(-8.3254538919136,1.07811780015612,16.9832294247164));
#31400=CARTESIAN_POINT('Ctrl Pts',(-8.84814324514455,1.03518144076042,17.0063833455655));
#31401=CARTESIAN_POINT('Ctrl Pts',(-9.29055455716002,0.753543513958735,
17.0295372664146));
#31402=CARTESIAN_POINT('Ctrl Pts',(-9.55067259647192,0.298146657000293,
17.0526911872637));
#31403=CARTESIAN_POINT('Ctrl Pts',(-9.56851697658858,-0.225999569709272,
17.0758451081128));
#31404=CARTESIAN_POINT('Ctrl Pts',(-9.33997297578552,-0.698032762648408,
17.0989990289619));
#31405=CARTESIAN_POINT('Ctrl Pts',(-8.91774035629475,-1.0091071883197,17.122152949811));
#31406=CARTESIAN_POINT('Ctrl Pts',(-8.39918135305896,-1.08749251329865,
17.14530687066));
#31407=CARTESIAN_POINT('Ctrl Pts',(-7.90387004581411,-0.915113844273164,
17.1684607915091));
#31408=CARTESIAN_POINT('Ctrl Pts',(-7.54601978416533,-0.531720022559295,
17.1916147123582));
#31409=CARTESIAN_POINT('Ctrl Pts',(-7.40814703695762,-0.0257170587575114,
17.2147686332073));
#31410=CARTESIAN_POINT('Ctrl Pts',(-7.52204354730195,0.486215343467395,
17.2379225540564));
#31411=CARTESIAN_POINT('Ctrl Pts',(-7.8614464633833,0.886033182876555,17.2610764749055));
#31412=CARTESIAN_POINT('Ctrl Pts',(-8.34809214828908,1.08153844871999,17.2842303957546));
#31413=CARTESIAN_POINT('Ctrl Pts',(-8.86976741345725,1.0276594545631,17.3073843166036));
#31414=CARTESIAN_POINT('Ctrl Pts',(-9.30617448785336,0.736799769641186,
17.3305382374527));
#31415=CARTESIAN_POINT('Ctrl Pts',(-9.55669095855414,0.276075414215511,
17.3536921583018));
#31416=CARTESIAN_POINT('Ctrl Pts',(-9.56352202728377,-0.248368053984077,
17.3768460791509));
#31417=CARTESIAN_POINT('Ctrl Pts',(-9.40458264633921,-0.559690113640409,
17.3922820263836));
#31418=CARTESIAN_POINT('Ctrl Pts',(-9.29338130674012,-0.687936125025675,
17.4));
#31419=CARTESIAN_POINT('Ctrl Pts',(-9.29338130674012,-0.687936125025675,
17.4));
#31420=CARTESIAN_POINT('Ctrl Pts',(-9.32590176996881,-0.655901643534808,
17.4));
#31421=CARTESIAN_POINT('Ctrl Pts',(-9.35618622301351,-0.62180741134238,
17.4));
#31422=CARTESIAN_POINT('Ctrl Pts',(-9.38414424671855,-0.585952842595447,
17.4));
#31423=CARTESIAN_POINT('Ctrl Pts',(-9.4125008379239,-0.549587133791166,
17.4));
#31424=CARTESIAN_POINT('Ctrl Pts',(-9.43846492414375,-0.511409752766397,
17.4));
#31425=CARTESIAN_POINT('Ctrl Pts',(-9.46191181465167,-0.47168786456472,
17.4));
#31426=CARTESIAN_POINT('Ctrl Pts',(-9.48267340922677,-0.436515194725088,
17.4));
#31427=CARTESIAN_POINT('Ctrl Pts',(-9.50146125422009,-0.400130473259426,
17.4));
#31428=CARTESIAN_POINT('Ctrl Pts',(-9.51816231358404,-0.362698001012095,
17.4));
#31429=CARTESIAN_POINT('Ctrl Pts',(-9.5228893675798,-0.35210314510194,17.4));
#31430=CARTESIAN_POINT('Ctrl Pts',(-9.52745040342208,-0.341420545917971,
17.4));
#31431=CARTESIAN_POINT('Ctrl Pts',(-9.53183247069625,-0.330679485922838,
17.4));
#31432=CARTESIAN_POINT('Ctrl Pts',(-9.54293259714113,-0.303471522959637,
17.4));
#31433=CARTESIAN_POINT('Ctrl Pts',(-9.55289892765706,-0.275859109257066,
17.4));
#31434=CARTESIAN_POINT('Ctrl Pts',(-9.56170405990825,-0.247910866813315,
17.4));
#31435=CARTESIAN_POINT('Ctrl Pts',(-9.57582363811113,-0.203094118630554,
17.4));
#31436=CARTESIAN_POINT('Ctrl Pts',(-9.5869600387577,-0.157414951204697,
17.4));
#31437=CARTESIAN_POINT('Ctrl Pts',(-9.59514858605679,-0.11117684925936,
17.4));
#31438=CARTESIAN_POINT('Ctrl Pts',(-9.60093527178937,-0.0785012897179607,
17.4));
#31439=CARTESIAN_POINT('Ctrl Pts',(-9.60524884863469,-0.0455458605504793,
17.4));
#31440=CARTESIAN_POINT('Ctrl Pts',(-9.60808714557939,-0.0124118703443701,
17.4));
#31441=CARTESIAN_POINT('Ctrl Pts',(-9.60984578868126,0.00811835057634134,
17.4));
#31442=CARTESIAN_POINT('Ctrl Pts',(-9.61103780203869,0.0287172011838359,
17.4));
#31443=CARTESIAN_POINT('Ctrl Pts',(-9.61166024116134,0.0493609406537205,
17.4));
#31444=CARTESIAN_POINT('Ctrl Pts',(-9.61202238478416,0.0613717515557251,
17.4));
#31445=CARTESIAN_POINT('Ctrl Pts',(-9.61219151258125,0.0734021836547561,
17.4));
#31446=CARTESIAN_POINT('Ctrl Pts',(-9.61216730618328,0.0854187262189934,
17.4));
#31447=CARTESIAN_POINT('Ctrl Pts',(-9.61206992538845,0.133760510359393,
17.4));
#31448=CARTESIAN_POINT('Ctrl Pts',(-9.60885229506756,0.181958671365902,
17.4));
#31449=CARTESIAN_POINT('Ctrl Pts',(-9.60254662600539,0.229702232680448,
17.4));
#31450=CARTESIAN_POINT('Ctrl Pts',(-9.60006992548072,0.24845464454845,17.4));
#31451=CARTESIAN_POINT('Ctrl Pts',(-9.5971162878431,0.267137112035182,17.4));
#31452=CARTESIAN_POINT('Ctrl Pts',(-9.59368553269945,0.285731284573432,
17.4));
#31453=CARTESIAN_POINT('Ctrl Pts',(-9.5852454443577,0.331475283283206,17.4));
#31454=CARTESIAN_POINT('Ctrl Pts',(-9.57392096633328,0.376685332484621,
17.4));
#31455=CARTESIAN_POINT('Ctrl Pts',(-9.55984225277605,0.421131437658512,
17.4));
#31456=CARTESIAN_POINT('Ctrl Pts',(-9.55380201884681,0.440200287337304,
17.4));
#31457=CARTESIAN_POINT('Ctrl Pts',(-9.54725424072087,0.459128450126187,
17.4));
#31458=CARTESIAN_POINT('Ctrl Pts',(-9.54020669887975,0.477897185647727,
17.4));
#31459=CARTESIAN_POINT('Ctrl Pts',(-9.53575786357977,0.489745148385171,
17.4));
#31460=CARTESIAN_POINT('Ctrl Pts',(-9.53110771266445,0.501534287767251,
17.4));
#31461=CARTESIAN_POINT('Ctrl Pts',(-9.52627028529036,0.513231192847217,
17.4));
#31462=CARTESIAN_POINT('Ctrl Pts',(-9.50753196688913,0.55854046878,17.4));
#31463=CARTESIAN_POINT('Ctrl Pts',(-9.48596288400885,0.602539245716482,
17.4));
#31464=CARTESIAN_POINT('Ctrl Pts',(-9.4617429788619,0.644973581298068,17.4));
#31465=CARTESIAN_POINT('Ctrl Pts',(-9.43730203087857,0.68779519361917,17.4));
#31466=CARTESIAN_POINT('Ctrl Pts',(-9.41016133012676,0.729024761307237,
17.4));
#31467=CARTESIAN_POINT('Ctrl Pts',(-9.38045491388209,0.768389604166219,
17.4));
#31468=CARTESIAN_POINT('Ctrl Pts',(-9.37505708296658,0.775542428122443,
17.4));
#31469=CARTESIAN_POINT('Ctrl Pts',(-9.36957441312197,0.782633627909684,
17.4));
#31470=CARTESIAN_POINT('Ctrl Pts',(-9.36400754339436,0.789661482345399,
17.4));
#31471=CARTESIAN_POINT('Ctrl Pts',(-9.34883017800262,0.808822037542452,
17.4));
#31472=CARTESIAN_POINT('Ctrl Pts',(-9.33302712271578,0.827511885585166,
17.4));
#31473=CARTESIAN_POINT('Ctrl Pts',(-9.31662661954985,0.845710363584338,
17.4));
#31474=CARTESIAN_POINT('Ctrl Pts',(-9.30887448664654,0.854312356990281,
17.4));
#31475=CARTESIAN_POINT('Ctrl Pts',(-9.30098883427567,0.862804538007458,
17.4));
#31476=CARTESIAN_POINT('Ctrl Pts',(-9.29297246379625,0.871184557480965,
17.4));
#31477=CARTESIAN_POINT('Ctrl Pts',(-9.2855447605525,0.878949205832212,17.4));
#31478=CARTESIAN_POINT('Ctrl Pts',(-9.27801053976762,0.886611521389777,
17.4));
#31479=CARTESIAN_POINT('Ctrl Pts',(-9.27037638926497,0.894166318207978,
17.4));
#31480=CARTESIAN_POINT('Ctrl Pts',(-9.23471836479337,0.92945369297585,17.4));
#31481=CARTESIAN_POINT('Ctrl Pts',(-9.19685839181085,0.962424199673336,
17.4));
#31482=CARTESIAN_POINT('Ctrl Pts',(-9.15706782341478,0.992922306002667,
17.4));
#31483=CARTESIAN_POINT('Ctrl Pts',(-9.1348200157453,1.00997448774444,17.4));
#31484=CARTESIAN_POINT('Ctrl Pts',(-9.11196784459699,1.02625325759119,17.4));
#31485=CARTESIAN_POINT('Ctrl Pts',(-9.08855339782672,1.04172681883086,17.4));
#31486=CARTESIAN_POINT('Ctrl Pts',(-9.07636602844239,1.04978090647893,17.4));
#31487=CARTESIAN_POINT('Ctrl Pts',(-9.06402403497495,1.05761791257647,17.4));
#31488=CARTESIAN_POINT('Ctrl Pts',(-9.05155345664447,1.06522115394551,17.4));
#31489=CARTESIAN_POINT('Ctrl Pts',(-9.00599344516773,1.09299883633154,17.4));
#31490=CARTESIAN_POINT('Ctrl Pts',(-8.95866633005178,1.11769733240675,17.4));
#31491=CARTESIAN_POINT('Ctrl Pts',(-8.90987139744227,1.13911609011303,17.4));
#31492=CARTESIAN_POINT('Ctrl Pts',(-8.87875620954714,1.15277424342671,17.4));
#31493=CARTESIAN_POINT('Ctrl Pts',(-8.84704320481553,1.16509794048545,17.4));
#31494=CARTESIAN_POINT('Ctrl Pts',(-8.81482206889638,1.17607882593351,17.4));
#31495=CARTESIAN_POINT('Ctrl Pts',(-9.55005247215833,-1.9100347204657E-5,
16.4658930328476));
#31496=CARTESIAN_POINT('Ctrl Pts',(-9.55009316010148,-0.0583092136036194,
16.4685430772439));
#31497=CARTESIAN_POINT('Ctrl Pts',(-9.54531572343602,-0.116592726407586,
16.4711931216402));
#31498=CARTESIAN_POINT('Ctrl Pts',(-9.53565824528574,-0.174056083597285,
16.4738431660365));
#31499=CARTESIAN_POINT('Ctrl Pts',(-9.50753186307544,-0.341412024998651,
16.4815611396529));
#31500=CARTESIAN_POINT('Ctrl Pts',(-9.43801277726438,-0.501811374257632,
16.4892791132692));
#31501=CARTESIAN_POINT('Ctrl Pts',(-9.33511616017773,-0.636760959930297,
16.4969970868856));
#31502=CARTESIAN_POINT('Ctrl Pts',(-9.23221954309108,-0.771710545602965,
16.504715060502));
#31503=CARTESIAN_POINT('Ctrl Pts',(-9.09594539472886,-0.881210367689316,
16.5124330341183));
#31504=CARTESIAN_POINT('Ctrl Pts',(-8.94200538233543,-0.952635692781543,
16.5201510077347));
#31505=CARTESIAN_POINT('Ctrl Pts',(-8.78806536994201,-1.02406101787377,
16.527868981351));
#31506=CARTESIAN_POINT('Ctrl Pts',(-8.61645949351738,-1.05741184597187,
16.5355869549674));
#31507=CARTESIAN_POINT('Ctrl Pts',(-8.44697297634186,-1.04884300822367,
16.5433049285838));
#31508=CARTESIAN_POINT('Ctrl Pts',(-8.27748645916635,-1.04027417047547,
16.5510229022001));
#31509=CARTESIAN_POINT('Ctrl Pts',(-8.11011930123993,-0.98978566688096,
16.5587408758165));
#31510=CARTESIAN_POINT('Ctrl Pts',(-7.96416802460607,-0.903198546994836,
16.5664588494329));
#31511=CARTESIAN_POINT('Ctrl Pts',(-7.81821674797221,-0.816611427108713,
16.5741768230492));
#31512=CARTESIAN_POINT('Ctrl Pts',(-7.6936813526309,-0.693925690930975,
16.5818947966656));
#31513=CARTESIAN_POINT('Ctrl Pts',(-7.60492009163335,-0.549286335881268,
16.5896127702819));
#31514=CARTESIAN_POINT('Ctrl Pts',(-7.5161588306358,-0.404646980831559,
16.5973307438983));
#31515=CARTESIAN_POINT('Ctrl Pts',(-7.463171703982,-0.238054006909883,16.6050487175147));
#31516=CARTESIAN_POINT('Ctrl Pts',(-7.45206783887804,-0.0687146769772104,
16.612766691131));
#31517=CARTESIAN_POINT('Ctrl Pts',(-7.44096397377408,0.100624652955459,
16.6204846647474));
#31518=CARTESIAN_POINT('Ctrl Pts',(-7.47174337021995,0.272710338899125,
16.6282026383638));
#31519=CARTESIAN_POINT('Ctrl Pts',(-7.54085733138834,0.427701838195537,
16.6359206119801));
#31520=CARTESIAN_POINT('Ctrl Pts',(-7.60997129255673,0.582693337491953,
16.6436385855965));
#31521=CARTESIAN_POINT('Ctrl Pts',(-7.71741981844764,0.720590650141115,
16.6513565592128));
#31522=CARTESIAN_POINT('Ctrl Pts',(-7.85081467903621,0.825494966787567,
16.6590745328292));
#31523=CARTESIAN_POINT('Ctrl Pts',(-7.98420953962478,0.930399283434019,
16.6667925064456));
#31524=CARTESIAN_POINT('Ctrl Pts',(-8.14355073491101,1.00231060407776,16.6745104800619));
#31525=CARTESIAN_POINT('Ctrl Pts',(-8.3104670926237,1.03293794497459,16.6822284536783));
#31526=CARTESIAN_POINT('Ctrl Pts',(-8.47738345033638,1.06356528587142,16.6899464272947));
#31527=CARTESIAN_POINT('Ctrl Pts',(-8.65187497047551,1.05290864702134,16.697664400911));
#31528=CARTESIAN_POINT('Ctrl Pts',(-8.81382373080072,1.00219668086311,16.7053823745274));
#31529=CARTESIAN_POINT('Ctrl Pts',(-8.97577249112593,0.951484714704877,
16.7131003481437));
#31530=CARTESIAN_POINT('Ctrl Pts',(-9.12517849163721,0.860717421238493,
16.7208183217601));
#31531=CARTESIAN_POINT('Ctrl Pts',(-9.24481603392765,0.740359775211364,
16.7285362953765));
#31532=CARTESIAN_POINT('Ctrl Pts',(-9.36445357621809,0.620002129184234,
16.7362542689928));
#31533=CARTESIAN_POINT('Ctrl Pts',(-9.45432266028768,0.470054130596359,
16.7439722426092));
#31534=CARTESIAN_POINT('Ctrl Pts',(-9.50406187004197,0.307803967282058,
16.7516902162256));
#31535=CARTESIAN_POINT('Ctrl Pts',(-9.5345723343245,0.208278304588784,16.7564244884329));
#31536=CARTESIAN_POINT('Ctrl Pts',(-9.54998312115351,0.104123703417168,
16.7611587606403));
#31537=CARTESIAN_POINT('Ctrl Pts',(-9.55003851802847,-1.48519297202892E-5,
16.7658930328476));
#31538=CARTESIAN_POINT('Ctrl Pts',(-8.81478889550445,1.17604951161381,16.2));
#31539=CARTESIAN_POINT('Ctrl Pts',(-8.86280065303638,1.1596386364084,16.2));
#31540=CARTESIAN_POINT('Ctrl Pts',(-8.90960823495586,1.14022110609085,16.2));
#31541=CARTESIAN_POINT('Ctrl Pts',(-8.9549737777663,1.11798780847924,16.2));
#31542=CARTESIAN_POINT('Ctrl Pts',(-9.00031713849028,1.09576538213465,16.2));
#31543=CARTESIAN_POINT('Ctrl Pts',(-9.04422076807012,1.07072924115979,16.2));
#31544=CARTESIAN_POINT('Ctrl Pts',(-9.08641991384138,1.04302575780302,16.2));
#31545=CARTESIAN_POINT('Ctrl Pts',(-9.1251986712936,1.01756773864081,16.2));
#31546=CARTESIAN_POINT('Ctrl Pts',(-9.16253828107189,0.989856378454144,
16.2));
#31547=CARTESIAN_POINT('Ctrl Pts',(-9.19820325527869,0.959979731284522,
16.2));
#31548=CARTESIAN_POINT('Ctrl Pts',(-9.20529901205526,0.954035596280082,
16.2));
#31549=CARTESIAN_POINT('Ctrl Pts',(-9.21233002234639,0.948004232316305,
16.2));
#31550=CARTESIAN_POINT('Ctrl Pts',(-9.2192889249183,0.941890947120833,16.2));
#31551=CARTESIAN_POINT('Ctrl Pts',(-9.24730713452057,0.917277395746144,
16.2));
#31552=CARTESIAN_POINT('Ctrl Pts',(-9.27408780072704,0.891399085013077,
16.2));
#31553=CARTESIAN_POINT('Ctrl Pts',(-9.29952946398766,0.864320328704408,
16.2));
#31554=CARTESIAN_POINT('Ctrl Pts',(-9.33347386455,0.828191710010907,16.2));
#31555=CARTESIAN_POINT('Ctrl Pts',(-9.36503664794811,0.789926769837996,
16.2));
#31556=CARTESIAN_POINT('Ctrl Pts',(-9.39406804371783,0.749791809119003,
16.2));
#31557=CARTESIAN_POINT('Ctrl Pts',(-9.41426326769662,0.7218725685999,16.2));
#31558=CARTESIAN_POINT('Ctrl Pts',(-9.43323268273991,0.693047684123375,
16.2));
#31559=CARTESIAN_POINT('Ctrl Pts',(-9.45091216409187,0.663401052699072,
16.2));
#31560=CARTESIAN_POINT('Ctrl Pts',(-9.46034291018765,0.647586683035633,
16.2));
#31561=CARTESIAN_POINT('Ctrl Pts',(-9.46940640954167,0.631538429490315,
16.2));
#31562=CARTESIAN_POINT('Ctrl Pts',(-9.47809147938961,0.615268771658106,
16.2));
#31563=CARTESIAN_POINT('Ctrl Pts',(-9.48251125162093,0.606989254836849,
16.2));
#31564=CARTESIAN_POINT('Ctrl Pts',(-9.48683300444743,0.598652398763581,
16.2));
#31565=CARTESIAN_POINT('Ctrl Pts',(-9.49105515788789,0.590259842587576,
16.2));
#31566=CARTESIAN_POINT('Ctrl Pts',(-9.49557721907162,0.581271146877932,
16.2));
#31567=CARTESIAN_POINT('Ctrl Pts',(-9.49998165828265,0.572225103576722,
16.2));
#31568=CARTESIAN_POINT('Ctrl Pts',(-9.50426374372789,0.563131296471702,
16.2));
#31569=CARTESIAN_POINT('Ctrl Pts',(-9.52493494242546,0.519232150602404,
16.2));
#31570=CARTESIAN_POINT('Ctrl Pts',(-9.54278537558293,0.474168676113686,
16.2));
#31571=CARTESIAN_POINT('Ctrl Pts',(-9.55766754962425,0.428188388568034,
16.2));
#31572=CARTESIAN_POINT('Ctrl Pts',(-9.56297844699411,0.411779724920264,
16.2));
#31573=CARTESIAN_POINT('Ctrl Pts',(-9.56791087712962,0.395254153812105,
16.2));
#31574=CARTESIAN_POINT('Ctrl Pts',(-9.57245656145425,0.378622557723441,
16.2));
#31575=CARTESIAN_POINT('Ctrl Pts',(-9.58437736922181,0.335007109381333,
16.2));
#31576=CARTESIAN_POINT('Ctrl Pts',(-9.59364121622314,0.290662195371642,
16.2));
#31577=CARTESIAN_POINT('Ctrl Pts',(-9.6002178916675,0.24583507512556,16.2));
#31578=CARTESIAN_POINT('Ctrl Pts',(-9.60298148599042,0.22699820593944,16.2));
#31579=CARTESIAN_POINT('Ctrl Pts',(-9.6052701103365,0.208076238849532,16.2));
#31580=CARTESIAN_POINT('Ctrl Pts',(-9.60707946344055,0.189087960713112,
16.2));
#31581=CARTESIAN_POINT('Ctrl Pts',(-9.6079693515963,0.179749018649314,16.2));
#31582=CARTESIAN_POINT('Ctrl Pts',(-9.60874342397162,0.170392071550278,
16.2));
#31583=CARTESIAN_POINT('Ctrl Pts',(-9.60940063069509,0.161025657024326,
16.2));
#31584=CARTESIAN_POINT('Ctrl Pts',(-9.61273662950675,0.113481487721126,
16.2));
#31585=CARTESIAN_POINT('Ctrl Pts',(-9.61305386042052,0.0658810798401326,
16.2));
#31586=CARTESIAN_POINT('Ctrl Pts',(-9.6103549875713,0.0185133182208896,
16.2));
#31587=CARTESIAN_POINT('Ctrl Pts',(-9.60768669390768,-0.0283177498764049,
16.2));
#31588=CARTESIAN_POINT('Ctrl Pts',(-9.60207007581538,-0.0749224868667112,
16.2));
#31589=CARTESIAN_POINT('Ctrl Pts',(-9.59345823475354,-0.121012650095075,
16.2));
#31590=CARTESIAN_POINT('Ctrl Pts',(-9.59107634935637,-0.133760387304665,
16.2));
#31591=CARTESIAN_POINT('Ctrl Pts',(-9.58846504996881,-0.146468654771097,
16.2));
#31592=CARTESIAN_POINT('Ctrl Pts',(-9.58562269218988,-0.159131062787288,
16.2));
#31593=CARTESIAN_POINT('Ctrl Pts',(-9.58068397833975,-0.181132518870406,
16.2));
#31594=CARTESIAN_POINT('Ctrl Pts',(-9.57504779217974,-0.202995620919267,
16.2));
#31595=CARTESIAN_POINT('Ctrl Pts',(-9.56872407785818,-0.22468856278884,
16.2));
#31596=CARTESIAN_POINT('Ctrl Pts',(-9.56551410869643,-0.235700077681537,
16.2));
#31597=CARTESIAN_POINT('Ctrl Pts',(-9.56212695335901,-0.246667721625346,
16.2));
#31598=CARTESIAN_POINT('Ctrl Pts',(-9.55856371499839,-0.257587153871304,
16.2));
#31599=CARTESIAN_POINT('Ctrl Pts',(-9.55533513157818,-0.267481046544088,
16.2));
#31600=CARTESIAN_POINT('Ctrl Pts',(-9.55196458780484,-0.277327250705073,
16.2));
#31601=CARTESIAN_POINT('Ctrl Pts',(-9.54845505697522,-0.287118724757319,
16.2));
#31602=CARTESIAN_POINT('Ctrl Pts',(-9.53268035933277,-0.331129605455121,
16.2));
#31603=CARTESIAN_POINT('Ctrl Pts',(-9.51409226223222,-0.374064154494532,
16.2));
#31604=CARTESIAN_POINT('Ctrl Pts',(-9.4928094624077,-0.415647754292589,
16.2));
#31605=CARTESIAN_POINT('Ctrl Pts',(-9.48095709789152,-0.438805608840179,
16.2));
#31606=CARTESIAN_POINT('Ctrl Pts',(-9.46826821755998,-0.461544009845136,
16.2));
#31607=CARTESIAN_POINT('Ctrl Pts',(-9.45475802396731,-0.483810850745379,
16.2));
#31608=CARTESIAN_POINT('Ctrl Pts',(-9.44902429640731,-0.493260900329658,
16.2));
#31609=CARTESIAN_POINT('Ctrl Pts',(-9.44314317361927,-0.502624771124578,
16.2));
#31610=CARTESIAN_POINT('Ctrl Pts',(-9.43712266825694,-0.511888352961157,
16.2));
#31611=CARTESIAN_POINT('Ctrl Pts',(-9.41182957357249,-0.550806124544883,
16.2));
#31612=CARTESIAN_POINT('Ctrl Pts',(-9.38404938266935,-0.588007231454378,
16.2));
#31613=CARTESIAN_POINT('Ctrl Pts',(-9.35388344975981,-0.623204450374551,
16.2));
#31614=CARTESIAN_POINT('Ctrl Pts',(-9.33467682049038,-0.645614496075499,
16.2));
#31615=CARTESIAN_POINT('Ctrl Pts',(-9.31450214867004,-0.667211421582346,
16.2));
#31616=CARTESIAN_POINT('Ctrl Pts',(-9.29341917486498,-0.68794102932241,
16.2));
#31617=CARTESIAN_POINT('Origin',(-8.5,0.,17.4));
#31618=CARTESIAN_POINT('',(-7.46076951545867,-1.8,17.4));
#31619=CARTESIAN_POINT('',(-6.42153903091735,0.,17.4));
#31620=CARTESIAN_POINT('',(-7.46076951545867,-1.8,17.4));
#31621=CARTESIAN_POINT('',(-7.46076951545867,1.8,17.4));
#31622=CARTESIAN_POINT('',(-6.42153903091735,0.,17.4));
#31623=CARTESIAN_POINT('',(-9.53923048454133,1.8,17.4));
#31624=CARTESIAN_POINT('',(-7.46076951545867,1.8,17.4));
#31625=CARTESIAN_POINT('',(-10.5784609690827,2.22044604925031E-16,17.4));
#31626=CARTESIAN_POINT('',(-9.53923048454133,1.8,17.4));
#31627=CARTESIAN_POINT('',(-9.53923048454133,-1.8,17.4));
#31628=CARTESIAN_POINT('',(-10.5784609690827,2.54538057293978E-16,17.4));
#31629=CARTESIAN_POINT('',(-9.53923048454133,-1.8,17.4));
#31630=CARTESIAN_POINT('Origin',(-8.5,0.,16.1));
#31631=CARTESIAN_POINT('Origin',(-9.53923048454133,-1.8,16.2));
#31632=CARTESIAN_POINT('',(-9.53923048454133,-1.8,16.2));
#31633=CARTESIAN_POINT('',(-7.46076951545867,-1.8,16.2));
#31634=CARTESIAN_POINT('',(-9.53923048454133,-1.8,16.2));
#31635=CARTESIAN_POINT('',(-7.46076951545867,-1.8,16.2));
#31636=CARTESIAN_POINT('',(-9.53923048454133,-1.8,16.2));
#31637=CARTESIAN_POINT('Origin',(-10.5784609690827,2.54538057293978E-16,
16.2));
#31638=CARTESIAN_POINT('',(-10.5784609690827,2.54538057293978E-16,16.2));
#31639=CARTESIAN_POINT('',(-10.5784609690827,2.54538057293978E-16,16.2));
#31640=CARTESIAN_POINT('',(-10.5784609690827,2.54538057293978E-16,16.2));
#31641=CARTESIAN_POINT('Origin',(-9.53923048454133,1.8,16.2));
#31642=CARTESIAN_POINT('',(-9.53923048454133,1.8,16.2));
#31643=CARTESIAN_POINT('',(-9.53923048454133,1.8,16.2));
#31644=CARTESIAN_POINT('',(-9.53923048454133,1.8,16.2));
#31645=CARTESIAN_POINT('Origin',(-7.46076951545867,1.8,16.2));
#31646=CARTESIAN_POINT('',(-7.46076951545867,1.8,16.2));
#31647=CARTESIAN_POINT('',(-7.46076951545867,1.8,16.2));
#31648=CARTESIAN_POINT('',(-7.46076951545867,1.8,16.2));
#31649=CARTESIAN_POINT('Origin',(-6.42153903091735,0.,16.2));
#31650=CARTESIAN_POINT('',(-6.42153903091735,0.,16.2));
#31651=CARTESIAN_POINT('',(-6.42153903091735,0.,16.2));
#31652=CARTESIAN_POINT('',(-6.42153903091735,0.,16.2));
#31653=CARTESIAN_POINT('Origin',(-7.46076951545867,-1.8,16.2));
#31654=CARTESIAN_POINT('',(-7.46076951545867,-1.8,16.2));
#31655=CARTESIAN_POINT('Origin',(-8.5,0.,16.2));
#31656=CARTESIAN_POINT('',(0.,0.,0.));
#31657=CARTESIAN_POINT('',(0.,0.,0.));
#31658=CARTESIAN_POINT('',(0.,0.,0.));
#31659=CARTESIAN_POINT('Origin',(-8.5,0.,22.7));
#31660=CARTESIAN_POINT('',(-9.55012850889018,-2.18470748328814E-5,23.8841069671524));
#31661=CARTESIAN_POINT('',(-9.55000870253874,1.05562245468413E-6,23.9658930328476));
#31662=CARTESIAN_POINT('',(-9.5501,-1.28600160378464E-16,22.7));
#31663=CARTESIAN_POINT('',(-9.29338130674011,-0.687936125025682,24.));
#31664=CARTESIAN_POINT('Ctrl Pts',(-9.55000870253874,1.05562245468413E-6,
23.9658930328476));
#31665=CARTESIAN_POINT('Ctrl Pts',(-9.55001614030791,-0.0803132194169134,
23.9695440482821));
#31666=CARTESIAN_POINT('Ctrl Pts',(-9.54090449002282,-0.160622529114386,
23.9731950637165));
#31667=CARTESIAN_POINT('Ctrl Pts',(-9.52264652698618,-0.238789064503808,
23.9768460791509));
#31668=CARTESIAN_POINT('Ctrl Pts',(-9.48405055840263,-0.404027275257131,
23.9845640527673));
#31669=CARTESIAN_POINT('Ctrl Pts',(-9.4045826463392,-0.559690113640418,
23.9922820263836));
#31670=CARTESIAN_POINT('Ctrl Pts',(-9.29338130674012,-0.687936125025676,
24.));
#31671=CARTESIAN_POINT('',(-7.70658052800239,-0.687941579884198,24.));
#31672=CARTESIAN_POINT('Origin',(-8.5,0.,24.));
#31673=CARTESIAN_POINT('Ctrl Pts',(-7.70658052800239,-0.687941579884198,
24.));
#31674=CARTESIAN_POINT('Ctrl Pts',(-7.79864121713694,-0.793916118632762,
23.9936166544345));
#31675=CARTESIAN_POINT('Ctrl Pts',(-7.91206802406805,-0.881431367900445,
23.987233308869));
#31676=CARTESIAN_POINT('Ctrl Pts',(-8.03812197772265,-0.94316120005307,
23.9808499633034));
#31677=CARTESIAN_POINT('Ctrl Pts',(-8.19053125567241,-1.01779748771859,
23.9731319896871));
#31678=CARTESIAN_POINT('Ctrl Pts',(-8.36139982794667,-1.05473875098712,
23.9654140160707));
#31679=CARTESIAN_POINT('Ctrl Pts',(-8.53102865307542,-1.04972479101945,
23.9576960424544));
#31680=CARTESIAN_POINT('Ctrl Pts',(-8.70065747820416,-1.04471083105178,
23.949978068838));
#31681=CARTESIAN_POINT('Ctrl Pts',(-8.86904655618739,-0.997741647847902,
23.9422600952216));
#31682=CARTESIAN_POINT('Ctrl Pts',(-9.01678099765897,-0.914232989059095,
23.9345421216053));
#31683=CARTESIAN_POINT('Ctrl Pts',(-9.16451543913055,-0.830724330270285,
23.9268241479889));
#31684=CARTESIAN_POINT('Ctrl Pts',(-9.29159524409048,-0.710676195896543,
23.9191061743725));
#31685=CARTESIAN_POINT('Ctrl Pts',(-9.38336905036905,-0.567929262511223,
23.9113882007562));
#31686=CARTESIAN_POINT('Ctrl Pts',(-9.47514285664761,-0.425182329125902,
23.9036702271398));
#31687=CARTESIAN_POINT('Ctrl Pts',(-9.53161066424481,-0.259736596729006,
23.8959522535235));
#31688=CARTESIAN_POINT('Ctrl Pts',(-9.54626192835179,-0.090667154812442,
23.8882342799071));
#31689=CARTESIAN_POINT('Ctrl Pts',(-9.54887359613867,-0.0605296040881374,
23.8868585089889));
#31690=CARTESIAN_POINT('Ctrl Pts',(-9.5501565429157,-0.0302769099643429,
23.8854827380706));
#31691=CARTESIAN_POINT('Ctrl Pts',(-9.55012850889018,-2.18470748328814E-5,
23.8841069671524));
#31692=CARTESIAN_POINT('Origin',(-8.5,0.,22.7));
#31693=CARTESIAN_POINT('',(-9.55014846165012,-1.85392301343956E-5,23.5841069671524));
#31694=CARTESIAN_POINT('',(-9.55002911984723,-9.63121900339139E-6,23.6658930328476));
#31695=CARTESIAN_POINT('',(-9.5501,-1.28600160378464E-16,22.7));
#31696=CARTESIAN_POINT('Ctrl Pts',(-9.55002911984723,-9.63121900339139E-6,
23.6658930328476));
#31697=CARTESIAN_POINT('Ctrl Pts',(-9.55005395760937,-0.0729827112292251,
23.6692103912693));
#31698=CARTESIAN_POINT('Ctrl Pts',(-9.54254664910082,-0.14595075200247,
23.6725277496911));
#31699=CARTESIAN_POINT('Ctrl Pts',(-9.52745273693827,-0.21731416785282,
23.6758451081128));
#31700=CARTESIAN_POINT('Ctrl Pts',(-9.49233611671553,-0.383344150353556,
23.6835630817291));
#31701=CARTESIAN_POINT('Ctrl Pts',(-9.41615474671242,-0.540688622979868,
23.6912810553455));
#31702=CARTESIAN_POINT('Ctrl Pts',(-9.30769192489819,-0.671206621789361,
23.6989990289619));
#31703=CARTESIAN_POINT('Ctrl Pts',(-9.19922910308395,-0.801724620598853,
23.7067170025782));
#31704=CARTESIAN_POINT('Ctrl Pts',(-9.0584848294586,-0.905416145591528,
23.7144349761946));
#31705=CARTESIAN_POINT('Ctrl Pts',(-8.90168615075291,-0.970326134859246,
23.722152949811));
#31706=CARTESIAN_POINT('Ctrl Pts',(-8.74488747204723,-1.03523612412696,
23.7298709234273));
#31707=CARTESIAN_POINT('Ctrl Pts',(-8.57203438826122,-1.06136457766973,
23.7375888970437));
#31708=CARTESIAN_POINT('Ctrl Pts',(-8.40305592256279,-1.04569901309732,
23.74530687066));
#31709=CARTESIAN_POINT('Ctrl Pts',(-8.23407745686436,-1.03003344852491,
23.7530248442764));
#31710=CARTESIAN_POINT('Ctrl Pts',(-8.06897360925351,-0.972573865837326,
23.7607428178928));
#31711=CARTESIAN_POINT('Ctrl Pts',(-7.926779946155,-0.879945072400683,23.7684607915091));
#31712=CARTESIAN_POINT('Ctrl Pts',(-7.7845862830565,-0.78731627896404,23.7761787651255));
#31713=CARTESIAN_POINT('Ctrl Pts',(-7.66530280447034,-0.659518274778334,
23.7838967387419));
#31714=CARTESIAN_POINT('Ctrl Pts',(-7.5826822635998,-0.511285407188883,
23.7916147123582));
#31715=CARTESIAN_POINT('Ctrl Pts',(-7.50006172272926,-0.363052539599431,
23.7993326859746));
#31716=CARTESIAN_POINT('Ctrl Pts',(-7.45410411957434,-0.194384808606232,
23.8070506595909));
#31717=CARTESIAN_POINT('Ctrl Pts',(-7.45010807549069,-0.0247288294128955,
23.8147686332073));
#31718=CARTESIAN_POINT('Ctrl Pts',(-7.44611203140704,0.144927149780442,
23.8224866068237));
#31719=CARTESIAN_POINT('Ctrl Pts',(-7.48407754639465,0.315571377173915,
23.83020458044));
#31720=CARTESIAN_POINT('Ctrl Pts',(-7.55962748533197,0.467529822444092,
23.8379225540564));
#31721=CARTESIAN_POINT('Ctrl Pts',(-7.63517742426929,0.619488267714268,
23.8456405276727));
#31722=CARTESIAN_POINT('Ctrl Pts',(-7.7483117871563,0.752760930861145,23.8533585012891));
#31723=CARTESIAN_POINT('Ctrl Pts',(-7.88598660108357,0.851981517213941,
23.8610764749055));
#31724=CARTESIAN_POINT('Ctrl Pts',(-8.02366141501085,0.951202103566738,
23.8687944485218));
#31725=CARTESIAN_POINT('Ctrl Pts',(-8.18587667997837,1.01637061312545,23.8765124221382));
#31726=CARTESIAN_POINT('Ctrl Pts',(-8.35393023216907,1.03997501555327,23.8842303957546));
#31727=CARTESIAN_POINT('Ctrl Pts',(-8.52198378435977,1.06357941798109,23.8919483693709));
#31728=CARTESIAN_POINT('Ctrl Pts',(-8.69587562377364,1.04561971327801,23.8996663429873));
#31729=CARTESIAN_POINT('Ctrl Pts',(-8.85555596986305,0.988163359218205,
23.9073843166037));
#31730=CARTESIAN_POINT('Ctrl Pts',(-9.01523631595246,0.930707005158396,
23.91510229022));
#31731=CARTESIAN_POINT('Ctrl Pts',(-9.1607051687174,0.833754001741858,23.9228202638364));
#31732=CARTESIAN_POINT('Ctrl Pts',(-9.27519234914899,0.708490052395413,
23.9305382374527));
#31733=CARTESIAN_POINT('Ctrl Pts',(-9.38967952958059,0.583226103048967,
23.9382562110691));
#31734=CARTESIAN_POINT('Ctrl Pts',(-9.47318503767883,0.429651207772614,
23.9459741846855));
#31735=CARTESIAN_POINT('Ctrl Pts',(-9.51607577917611,0.265456968572753,
23.9536921583018));
#31736=CARTESIAN_POINT('Ctrl Pts',(-9.53867689972046,0.178935410229467,
23.9577591164838));
#31737=CARTESIAN_POINT('Ctrl Pts',(-9.55000041742005,0.0894651523548535,
23.9618260746657));
#31738=CARTESIAN_POINT('Ctrl Pts',(-9.55000870253874,1.05562245468413E-6,
23.9658930328476));
#31739=CARTESIAN_POINT('Ctrl Pts',(-9.55012850889018,-2.18470748328814E-5,
23.8841069671524));
#31740=CARTESIAN_POINT('Ctrl Pts',(-9.54999927409541,0.139451766551989,
23.8777647644543));
#31741=CARTESIAN_POINT('Ctrl Pts',(-9.52200983360965,0.278975719817604,
23.8714225617561));
#31742=CARTESIAN_POINT('Ctrl Pts',(-9.46789815100873,0.407501764958256,
23.865080359058));
#31743=CARTESIAN_POINT('Ctrl Pts',(-9.40204838894191,0.563908091376159,
23.8573623854417));
#31744=CARTESIAN_POINT('Ctrl Pts',(-9.2975141441915,0.704027592775735,23.8496444118253));
#31745=CARTESIAN_POINT('Ctrl Pts',(-9.1663476221531,0.811705232975747,23.8419264382089));
#31746=CARTESIAN_POINT('Ctrl Pts',(-9.03518110011469,0.919382873175757,
23.8342084645926));
#31747=CARTESIAN_POINT('Ctrl Pts',(-8.8773823007883,0.994618652176204,23.8264904909762));
#31748=CARTESIAN_POINT('Ctrl Pts',(-8.71114457750307,1.02873830379683,23.8187725173598));
#31749=CARTESIAN_POINT('Ctrl Pts',(-8.54490685421784,1.06285795541745,23.8110545437435));
#31750=CARTESIAN_POINT('Ctrl Pts',(-8.37023020697377,1.05586147965824,23.8033365701271));
#31751=CARTESIAN_POINT('Ctrl Pts',(-8.20725389715392,1.00855552775547,23.7956185965107));
#31752=CARTESIAN_POINT('Ctrl Pts',(-8.04427758733408,0.961249575852697,
23.7879006228944));
#31753=CARTESIAN_POINT('Ctrl Pts',(-7.89300161493846,0.873634147806356,
23.780182649278));
#31754=CARTESIAN_POINT('Ctrl Pts',(-7.77086727824076,0.755810827431719,
23.7724646756617));
#31755=CARTESIAN_POINT('Ctrl Pts',(-7.64873294154307,0.63798750705708,23.7647467020453));
#31756=CARTESIAN_POINT('Ctrl Pts',(-7.5557402405433,0.489956294354147,23.7570287284289));
#31757=CARTESIAN_POINT('Ctrl Pts',(-7.50261072631204,0.328784381272252,
23.7493107548126));
#31758=CARTESIAN_POINT('Ctrl Pts',(-7.44948121208079,0.167612468190361,
23.7415927811962));
#31759=CARTESIAN_POINT('Ctrl Pts',(-7.43621488461805,-0.00670014527048846,
23.7338748075799));
#31760=CARTESIAN_POINT('Ctrl Pts',(-7.464341279731,-0.174056163419163,23.7261568339635));
#31761=CARTESIAN_POINT('Ctrl Pts',(-7.49246767484396,-0.34141218156784,
23.7184388603471));
#31762=CARTESIAN_POINT('Ctrl Pts',(-7.5619867925326,-0.501811604404344,
23.7107208867308));
#31763=CARTESIAN_POINT('Ctrl Pts',(-7.66488345680942,-0.63676125197269,
23.7030029131144));
#31764=CARTESIAN_POINT('Ctrl Pts',(-7.76778012108624,-0.771710899541037,
23.695284939498));
#31765=CARTESIAN_POINT('Ctrl Pts',(-7.90405433195122,-0.881210771841228,
23.6875669658817));
#31766=CARTESIAN_POINT('Ctrl Pts',(-8.05799441494728,-0.952636129689753,
23.6798489922653));
#31767=CARTESIAN_POINT('Ctrl Pts',(-8.21193449794334,-1.02406148753828,
23.672131018649));
#31768=CARTESIAN_POINT('Ctrl Pts',(-8.38354045307049,-1.05741233093514,
23.6644130450326));
#31769=CARTESIAN_POINT('Ctrl Pts',(-8.55302704797763,-1.04884348925778,
23.6566950714162));
#31770=CARTESIAN_POINT('Ctrl Pts',(-8.72251364288478,-1.04027464758041,
23.6489770977999));
#31771=CARTESIAN_POINT('Ctrl Pts',(-8.88988087757193,-0.989786120828835,
23.6412591241835));
#31772=CARTESIAN_POINT('Ctrl Pts',(-9.03583222114397,-0.903198961230685,
23.6335411505671));
#31773=CARTESIAN_POINT('Ctrl Pts',(-9.18178356471601,-0.816611801632534,
23.6258231769508));
#31774=CARTESIAN_POINT('Ctrl Pts',(-9.30631901717293,-0.693926009187812,
23.6181052033344));
#31775=CARTESIAN_POINT('Ctrl Pts',(-9.39508031887919,-0.549286587801987,
23.6103872297181));
#31776=CARTESIAN_POINT('Ctrl Pts',(-9.48384162058545,-0.404647166416162,
23.6026692561017));
#31777=CARTESIAN_POINT('Ctrl Pts',(-9.53682877154105,-0.238054116089234,
23.5949512824853));
#31778=CARTESIAN_POINT('Ctrl Pts',(-9.54793264173766,-0.0687147084919738,
23.587233308869));
#31779=CARTESIAN_POINT('Ctrl Pts',(-9.54943193392396,-0.0458497752616798,
23.5861911949634));
#31780=CARTESIAN_POINT('Ctrl Pts',(-9.55016762861391,-0.0229347716572958,
23.5851490810579));
#31781=CARTESIAN_POINT('Ctrl Pts',(-9.55014846165012,-1.85392301343956E-5,
23.5841069671524));
#31782=CARTESIAN_POINT('Origin',(-8.5,0.,22.7));
#31783=CARTESIAN_POINT('',(-9.55016549375182,-1.36966017015294E-5,23.2841069671524));
#31784=CARTESIAN_POINT('',(-9.55003901931283,-1.48519368357603E-5,23.3658930328476));
#31785=CARTESIAN_POINT('',(-9.5501,-1.28600160378464E-16,22.7));
#31786=CARTESIAN_POINT('Ctrl Pts',(-9.55003901931283,-1.48519368357603E-5,
23.3658930328476));
#31787=CARTESIAN_POINT('Ctrl Pts',(-9.55007393234815,-0.0656465877237161,
23.3688767342566));
#31788=CARTESIAN_POINT('Ctrl Pts',(-9.54400975139509,-0.131271950178925,
23.3718604356656));
#31789=CARTESIAN_POINT('Ctrl Pts',(-9.53178246487035,-0.195728177219803,
23.3748441370746));
#31790=CARTESIAN_POINT('Ctrl Pts',(-9.50015400683739,-0.36245781652283,
23.382562110691));
#31791=CARTESIAN_POINT('Ctrl Pts',(-9.42728775074502,-0.521364683757543,
23.3902800843074));
#31792=CARTESIAN_POINT('Ctrl Pts',(-9.32158477919497,-0.654127682311983,
23.3979980579237));
#31793=CARTESIAN_POINT('Ctrl Pts',(-9.21588180764493,-0.786890680866422,
23.4057160315401));
#31794=CARTESIAN_POINT('Ctrl Pts',(-9.07734212063722,-0.893509810740587,
23.4134340051565));
#31795=CARTESIAN_POINT('Ctrl Pts',(-8.92193858979441,-0.961692466755417,
23.4211519787728));
#31796=CARTESIAN_POINT('Ctrl Pts',(-8.76653505895159,-1.02987512277025,
23.4288699523892));
#31797=CARTESIAN_POINT('Ctrl Pts',(-8.59426768427367,-1.05962130492574,
23.4365879260056));
#31798=CARTESIAN_POINT('Ctrl Pts',(-8.42499795613852,-1.04750144037518,
23.4443058996219));
#31799=CARTESIAN_POINT('Ctrl Pts',(-8.25572822800336,-1.03538157582462,
23.4520238732383));
#31800=CARTESIAN_POINT('Ctrl Pts',(-8.08945614641095,-0.981395664568007,
23.4597418468546));
#31801=CARTESIAN_POINT('Ctrl Pts',(-7.94535197708869,-0.891767988241791,
23.467459820471));
#31802=CARTESIAN_POINT('Ctrl Pts',(-7.80124780776642,-0.802140311915576,
23.4751777940874));
#31803=CARTESIAN_POINT('Ctrl Pts',(-7.67931155071428,-0.676870870519757,
23.4828957677037));
#31804=CARTESIAN_POINT('Ctrl Pts',(-7.59360179247881,-0.530402548611195,
23.4906137413201));
#31805=CARTESIAN_POINT('Ctrl Pts',(-7.50789203424333,-0.383934226702632,
23.4983317149364));
#31806=CARTESIAN_POINT('Ctrl Pts',(-7.45840877482451,-0.216267024281328,
23.5060496885528));
#31807=CARTESIAN_POINT('Ctrl Pts',(-7.45085716461962,-0.0467320569044314,
23.5137676621692));
#31808=CARTESIAN_POINT('Ctrl Pts',(-7.44330555441472,0.122802910472465,
23.5214856357855));
#31809=CARTESIAN_POINT('Ctrl Pts',(-7.47768559342375,0.294205642804954,
23.5292036094019));
#31810=CARTESIAN_POINT('Ctrl Pts',(-7.5500334503303,0.44771433825753,23.5369215830183));
#31811=CARTESIAN_POINT('Ctrl Pts',(-7.62238130723685,0.601223033710108,
23.5446395566346));
#31812=CARTESIAN_POINT('Ctrl Pts',(-7.73269698204091,0.736837692282775,
23.552357530251));
#31813=CARTESIAN_POINT('Ctrl Pts',(-7.8682616780666,0.838922682232956,23.5600755038673));
#31814=CARTESIAN_POINT('Ctrl Pts',(-8.00382637409228,0.941007672183136,
23.5677934774837));
#31815=CARTESIAN_POINT('Ctrl Pts',(-8.1646400913396,1.00956299351083,23.5755114511001));
#31816=CARTESIAN_POINT('Ctrl Pts',(-8.33216188375618,1.0366845908627,23.5832294247164));
#31817=CARTESIAN_POINT('Ctrl Pts',(-8.49968367617277,1.06380618821457,23.5909473983328));
#31818=CARTESIAN_POINT('Ctrl Pts',(-8.67391354375863,1.04949406159062,23.5986653719492));
#31819=CARTESIAN_POINT('Ctrl Pts',(-8.83476373142291,0.995398321395473,
23.6063833455655));
#31820=CARTESIAN_POINT('Ctrl Pts',(-8.99561391908718,0.94130258120033,23.6141013191819));
#31821=CARTESIAN_POINT('Ctrl Pts',(-9.14308442682988,0.847423227433994,
23.6218192927983));
#31822=CARTESIAN_POINT('Ctrl Pts',(-9.26017270794676,0.724584038172587,
23.6295372664146));
#31823=CARTESIAN_POINT('Ctrl Pts',(-9.37726098906364,0.601744848911179,
23.637255240031));
#31824=CARTESIAN_POINT('Ctrl Pts',(-9.4639670435547,0.449945824154699,23.6449732136473));
#31825=CARTESIAN_POINT('Ctrl Pts',(-9.51029413557904,0.286688565588882,
23.6526911872637));
#31826=CARTESIAN_POINT('Ctrl Pts',(-9.53670880285049,0.193602943845163,
23.6570918024583));
#31827=CARTESIAN_POINT('Ctrl Pts',(-9.54999617151317,0.0967922225061255,
23.661492417653));
#31828=CARTESIAN_POINT('Ctrl Pts',(-9.55002911984723,-9.63121900339139E-6,
23.6658930328476));
#31829=CARTESIAN_POINT('Ctrl Pts',(-9.55014846165012,-1.85392301343956E-5,
23.5841069671524));
#31830=CARTESIAN_POINT('Ctrl Pts',(-9.5500256766449,0.146784561633176,23.5774311074415));
#31831=CARTESIAN_POINT('Ctrl Pts',(-9.51892503357627,0.293638090674144,
23.5707552477307));
#31832=CARTESIAN_POINT('Ctrl Pts',(-9.45914310850558,0.427702034353384,
23.5640793880199));
#31833=CARTESIAN_POINT('Ctrl Pts',(-9.39002911563927,0.582693604733889,
23.5563614144035));
#31834=CARTESIAN_POINT('Ctrl Pts',(-9.28258054046903,0.720590980627308,
23.5486434407872));
#31835=CARTESIAN_POINT('Ctrl Pts',(-9.14918561870127,0.825495345386306,
23.5409254671708));
#31836=CARTESIAN_POINT('Ctrl Pts',(-9.01579069693351,0.930399710145303,
23.5332074935544));
#31837=CARTESIAN_POINT('Ctrl Pts',(-8.85644942856823,1.00231106376988,23.5254895199381));
#31838=CARTESIAN_POINT('Ctrl Pts',(-8.68953299430229,1.0329384187134,23.5177715463217));
#31839=CARTESIAN_POINT('Ctrl Pts',(-8.52261656003635,1.06356577365693,23.5100535727053));
#31840=CARTESIAN_POINT('Ctrl Pts',(-8.34812495986976,1.05290912991939,23.502335599089));
#31841=CARTESIAN_POINT('Ctrl Pts',(-8.1861761252696,1.00219714050302,23.4946176254726));
#31842=CARTESIAN_POINT('Ctrl Pts',(-8.02422729066943,0.951485151086648,
23.4868996518563));
#31843=CARTESIAN_POINT('Ctrl Pts',(-7.87482122163571,0.860717815991441,
23.4791816782399));
#31844=CARTESIAN_POINT('Ctrl Pts',(-7.75518362447561,0.740360114764396,
23.4714637046235));
#31845=CARTESIAN_POINT('Ctrl Pts',(-7.63554602731551,0.620002413537354,
23.4637457310072));
#31846=CARTESIAN_POINT('Ctrl Pts',(-7.54567690202903,0.470054346178473,
23.4560277573908));
#31847=CARTESIAN_POINT('Ctrl Pts',(-7.49593766946272,0.307804108450993,
23.4483097837744));
#31848=CARTESIAN_POINT('Ctrl Pts',(-7.44619843689641,0.145553870723511,
23.4405918101581));
#31849=CARTESIAN_POINT('Ctrl Pts',(-7.43658909705025,-0.0289985373725711,
23.4328738365417));
#31850=CARTESIAN_POINT('Ctrl Pts',(-7.46821755448973,-0.195728173547128,
23.4251558629254));
#31851=CARTESIAN_POINT('Ctrl Pts',(-7.49984601192921,-0.362457809721686,
23.417437889309));
#31852=CARTESIAN_POINT('Ctrl Pts',(-7.57271226665433,-0.521364673974718,
23.4097199156926));
#31853=CARTESIAN_POINT('Ctrl Pts',(-7.67841523622097,-0.654127670038036,
23.4020019420763));
#31854=CARTESIAN_POINT('Ctrl Pts',(-7.78411820578762,-0.786890666101354,
23.3942839684599));
#31855=CARTESIAN_POINT('Ctrl Pts',(-7.92265789019581,-0.893509793974957,
23.3865659948436));
#31856=CARTESIAN_POINT('Ctrl Pts',(-8.07806141812267,-0.961692448710438,
23.3788480212272));
#31857=CARTESIAN_POINT('Ctrl Pts',(-8.23346494604952,-1.02987510344592,
23.3711300476108));
#31858=CARTESIAN_POINT('Ctrl Pts',(-8.40573231749505,-1.05962128504328,
23.3634120739945));
#31859=CARTESIAN_POINT('Ctrl Pts',(-8.57500204245408,-1.04750142072014,
23.3556941003781));
#31860=CARTESIAN_POINT('Ctrl Pts',(-8.7442717674131,-1.03538155639701,23.3479761267617));
#31861=CARTESIAN_POINT('Ctrl Pts',(-8.91054384588563,-0.981395646153393,
23.3402581531454));
#31862=CARTESIAN_POINT('Ctrl Pts',(-9.05464801250397,-0.89176797150894,
23.332540179529));
#31863=CARTESIAN_POINT('Ctrl Pts',(-9.19875217912231,-0.802140296864486,
23.3248222059126));
#31864=CARTESIAN_POINT('Ctrl Pts',(-9.32068843388647,-0.676870857819196,
23.3171042322963));
#31865=CARTESIAN_POINT('Ctrl Pts',(-9.40639819051372,-0.530402538658936,
23.3093862586799));
#31866=CARTESIAN_POINT('Ctrl Pts',(-9.49210794714098,-0.383934219498677,
23.3016682850636));
#31867=CARTESIAN_POINT('Ctrl Pts',(-9.54159120563132,-0.216267020223448,
23.2939503114472));
#31868=CARTESIAN_POINT('Ctrl Pts',(-9.54914281569454,-0.0467320560276536,
23.2862323378308));
#31869=CARTESIAN_POINT('Ctrl Pts',(-9.54983600155745,-0.0311699123966164,
23.285523880938));
#31870=CARTESIAN_POINT('Ctrl Pts',(-9.55017587230574,-0.0155920310208985,
23.2848154240452));
#31871=CARTESIAN_POINT('Ctrl Pts',(-9.55016549375182,-1.36966017015294E-5,
23.2841069671524));
#31872=CARTESIAN_POINT('Origin',(-8.5,0.,22.7));
#31873=CARTESIAN_POINT('',(-9.5501777037735,-7.61342713928581E-6,22.9841069671524));
#31874=CARTESIAN_POINT('',(-9.55005297345142,-1.9100363332081E-5,23.0658930328476));
#31875=CARTESIAN_POINT('',(-9.5501,-1.28600160378464E-16,22.7));
#31876=CARTESIAN_POINT('',(-7.70661869325983,-0.687936125025621,22.8));
#31877=CARTESIAN_POINT('Ctrl Pts',(-9.5501777037735,-7.61342713928581E-6,
22.9841069671524));
#31878=CARTESIAN_POINT('Ctrl Pts',(-9.55011195539345,0.161456714688093,
22.9767637934161));
#31879=CARTESIAN_POINT('Ctrl Pts',(-9.5122535813712,0.322950769429109,22.9694206196799));
#31880=CARTESIAN_POINT('Ctrl Pts',(-9.44037249633203,0.46752981291848,22.9620774459436));
#31881=CARTESIAN_POINT('Ctrl Pts',(-9.36482255869282,0.619488255304342,
22.9543594723273));
#31882=CARTESIAN_POINT('Ctrl Pts',(-9.25168819794997,0.75276091631997,22.9466414987109));
#31883=CARTESIAN_POINT('Ctrl Pts',(-9.11401338581573,0.851981499935064,
22.9389235250945));
#31884=CARTESIAN_POINT('Ctrl Pts',(-8.9763385736815,0.951202083550158,22.9312055514782));
#31885=CARTESIAN_POINT('Ctrl Pts',(-8.8141233101559,1.01637058976472,22.9234875778618));
#31886=CARTESIAN_POINT('Ctrl Pts',(-8.64606976010883,1.03997499101187,22.9157696042454));
#31887=CARTESIAN_POINT('Ctrl Pts',(-8.47801621006176,1.06357939225902,22.9080516306291));
#31888=CARTESIAN_POINT('Ctrl Pts',(-8.30412437349322,1.04561968853876,22.9003336570127));
#31889=CARTESIAN_POINT('Ctrl Pts',(-8.1444440256564,0.988163330864678,22.8926156833964));
#31890=CARTESIAN_POINT('Ctrl Pts',(-7.98476367781957,0.930706973190595,
22.88489770978));
#31891=CARTESIAN_POINT('Ctrl Pts',(-7.83929481871444,0.833753961562689,
22.8771797361636));
#31892=CARTESIAN_POINT('Ctrl Pts',(-7.72480763500893,0.708490009755435,
22.8694617625473));
#31893=CARTESIAN_POINT('Ctrl Pts',(-7.61032045130341,0.583226057948181,
22.8617437889309));
#31894=CARTESIAN_POINT('Ctrl Pts',(-7.52681494299751,0.429651165961579,
22.8540258153145));
#31895=CARTESIAN_POINT('Ctrl Pts',(-7.48392418333634,0.265456912966516,
22.8463078416982));
#31896=CARTESIAN_POINT('Ctrl Pts',(-7.44103342367517,0.101262659971452,
22.8385898680818));
#31897=CARTESIAN_POINT('Ctrl Pts',(-7.43875741265874,-0.0735509540320737,
22.8308718944655));
#31898=CARTESIAN_POINT('Ctrl Pts',(-7.47735339515514,-0.238789147435026,
22.8231539208491));
#31899=CARTESIAN_POINT('Ctrl Pts',(-7.51594937765153,-0.404027340837977,
22.8154359472327));
#31900=CARTESIAN_POINT('Ctrl Pts',(-7.59541735366076,-0.559690113640355,
22.8077179736164));
#31901=CARTESIAN_POINT('Ctrl Pts',(-7.70661869325984,-0.687936125025627,
22.8));
#31902=CARTESIAN_POINT('',(-9.29341948377034,-0.687941604344792,22.8));
#31903=CARTESIAN_POINT('Origin',(-8.5,0.,22.8));
#31904=CARTESIAN_POINT('Ctrl Pts',(-9.29341948377034,-0.687941604344792,
22.8));
#31905=CARTESIAN_POINT('Ctrl Pts',(-9.20135879382107,-0.793916141421131,
22.8063833455655));
#31906=CARTESIAN_POINT('Ctrl Pts',(-9.08793198530623,-0.881431392368405,
22.812766691131));
#31907=CARTESIAN_POINT('Ctrl Pts',(-8.961878029636,-0.943161224705925,22.8191500366966));
#31908=CARTESIAN_POINT('Ctrl Pts',(-8.80946874924919,-1.017797512595,22.8268680103129));
#31909=CARTESIAN_POINT('Ctrl Pts',(-8.63860017390651,-1.05473877390202,
22.8345859839293));
#31910=CARTESIAN_POINT('Ctrl Pts',(-8.46897134575844,-1.04972481267189,
22.8423039575456));
#31911=CARTESIAN_POINT('Ctrl Pts',(-8.29934251761038,-1.04471085144175,
22.850021931162));
#31912=CARTESIAN_POINT('Ctrl Pts',(-8.13095343665695,-0.997741667674461,
22.8577399047784));
#31913=CARTESIAN_POINT('Ctrl Pts',(-7.98321899249379,-0.914233007224389,
22.8654578783947));
#31914=CARTESIAN_POINT('Ctrl Pts',(-7.83548454833064,-0.830724346774318,
22.8731758520111));
#31915=CARTESIAN_POINT('Ctrl Pts',(-7.70840474095778,-0.710676209641467,
22.8808938256275));
#31916=CARTESIAN_POINT('Ctrl Pts',(-7.61663093296774,-0.567929273382309,
22.8886117992438));
#31917=CARTESIAN_POINT('Ctrl Pts',(-7.52485712497771,-0.425182337123151,
22.8963297728602));
#31918=CARTESIAN_POINT('Ctrl Pts',(-7.4683893163705,-0.259736601737684,
22.9040477464765));
#31919=CARTESIAN_POINT('Ctrl Pts',(-7.4537380520049,-0.0906671566566106,
22.9117657200929));
#31920=CARTESIAN_POINT('Ctrl Pts',(-7.43908678763931,0.0784022884244615,
22.9194836937093));
#31921=CARTESIAN_POINT('Ctrl Pts',(-7.46625206751533,0.251095443201141,
22.9272016673256));
#31922=CARTESIAN_POINT('Ctrl Pts',(-7.53210183081577,0.407501772587699,
22.934919640942));
#31923=CARTESIAN_POINT('Ctrl Pts',(-7.5979515941162,0.563908101974257,22.9426376145584));
#31924=CARTESIAN_POINT('Ctrl Pts',(-7.70248584084105,0.704027605970695,
22.9503555881747));
#31925=CARTESIAN_POINT('Ctrl Pts',(-7.83365236534431,0.811705248185335,
22.9580735617911));
#31926=CARTESIAN_POINT('Ctrl Pts',(-7.96481888984757,0.919382890399975,
22.9657915354074));
#31927=CARTESIAN_POINT('Ctrl Pts',(-8.12261769212924,0.994618670832817,
22.9735095090238));
#31928=CARTESIAN_POINT('Ctrl Pts',(-8.28885541853258,1.02873832309996,22.9812274826402));
#31929=CARTESIAN_POINT('Ctrl Pts',(-8.45509314493592,1.06285797536711,22.9889454562565));
#31930=CARTESIAN_POINT('Ctrl Pts',(-8.62976979546093,1.05586149946856,22.9966634298729));
#31931=CARTESIAN_POINT('Ctrl Pts',(-8.79274610833971,1.00855554667633,23.0043814034893));
#31932=CARTESIAN_POINT('Ctrl Pts',(-8.95572242121848,0.961249593884094,
23.0120993771056));
#31933=CARTESIAN_POINT('Ctrl Pts',(-9.10699839645102,0.873634164198181,
23.019817350722));
#31934=CARTESIAN_POINT('Ctrl Pts',(-9.22913273544003,0.755810841613994,
23.0275353243383));
#31935=CARTESIAN_POINT('Ctrl Pts',(-9.35126707442905,0.637987519029806,
23.0352532979547));
#31936=CARTESIAN_POINT('Ctrl Pts',(-9.44425977717454,0.489956303547343,
23.0429712715711));
#31937=CARTESIAN_POINT('Ctrl Pts',(-9.49738929240291,0.328784387440792,
23.0506892451874));
#31938=CARTESIAN_POINT('Ctrl Pts',(-9.53227625056806,0.222952480817186,
23.0557571744075));
#31939=CARTESIAN_POINT('Ctrl Pts',(-9.54997516203667,0.111454620464842,
23.0608251036276));
#31940=CARTESIAN_POINT('Ctrl Pts',(-9.55005297345142,-1.9100363332081E-5,
23.0658930328476));
#31941=CARTESIAN_POINT('Origin',(-8.5,0.,22.1374873996035));
#31942=CARTESIAN_POINT('',(-9.71736782397678,-1.11661056032553E-5,23.7625126003965));
#31943=CARTESIAN_POINT('',(-9.71748305223155,-2.5328750760409E-5,23.7874873996035));
#31944=CARTESIAN_POINT('',(-9.71745,-6.10603367124078E-16,22.1374873996035));
#31945=CARTESIAN_POINT('',(-8.18521110449559,1.17604951161383,24.));
#31946=CARTESIAN_POINT('Ctrl Pts',(-9.71748305223155,-2.53287507604727E-5,
23.7874873996035));
#31947=CARTESIAN_POINT('Ctrl Pts',(-9.71751555392126,-0.0351020131759212,
23.7888631705217));
#31948=CARTESIAN_POINT('Ctrl Pts',(-9.70768391907026,-0.266938163521721,
23.7979569150563));
#31949=CARTESIAN_POINT('Ctrl Pts',(-9.56508040992899,-0.684753960099927,
23.8147686332073));
#31950=CARTESIAN_POINT('Ctrl Pts',(-9.12308448035522,-1.10229305502416,
23.8379225540564));
#31951=CARTESIAN_POINT('Ctrl Pts',(-8.53741087882009,-1.26565644543905,
23.8610764749055));
#31952=CARTESIAN_POINT('Ctrl Pts',(-7.94311335482628,-1.13717113651722,
23.8842303957546));
#31953=CARTESIAN_POINT('Ctrl Pts',(-7.47722227522078,-0.746471900623929,
23.9073843166037));
#31954=CARTESIAN_POINT('Ctrl Pts',(-7.24718526716919,-0.183635135086069,
23.9305382374527));
#31955=CARTESIAN_POINT('Ctrl Pts',(-7.30600778196775,0.421517743452463,
23.9536921583018));
#31956=CARTESIAN_POINT('Ctrl Pts',(-7.64021434930425,0.929509330617972,
23.9768460791509));
#31957=CARTESIAN_POINT('Ctrl Pts',(-7.99510874416175,1.12516550422187,23.9922820263836));
#31958=CARTESIAN_POINT('Ctrl Pts',(-8.18521110449561,1.17604951161383,24.));
#31959=CARTESIAN_POINT('',(-8.81478889550438,1.17604951161383,24.));
#31960=CARTESIAN_POINT('Origin',(-8.5,0.,24.));
#31961=CARTESIAN_POINT('Ctrl Pts',(-9.71736782397678,-1.116610560329E-5,
23.7625126003965));
#31962=CARTESIAN_POINT('Ctrl Pts',(-9.71739662002813,-0.0846136575430615,
23.7658299588182));
#31963=CARTESIAN_POINT('Ctrl Pts',(-9.68844334159764,-0.366027961834239,
23.7768652908563));
#31964=CARTESIAN_POINT('Ctrl Pts',(-9.47383638460599,-0.809275680645407,
23.7956185965108));
#31965=CARTESIAN_POINT('Ctrl Pts',(-8.98431410313225,-1.16992489625058,
23.8187725173598));
#31966=CARTESIAN_POINT('Ctrl Pts',(-8.38311425495986,-1.2608022005996,23.8419264382089));
#31967=CARTESIAN_POINT('Ctrl Pts',(-7.80886700439182,-1.06095217981207,
23.865080359058));
#31968=CARTESIAN_POINT('Ctrl Pts',(-7.39398745671621,-0.616458283433,23.8882342799071));
#31969=CARTESIAN_POINT('Ctrl Pts',(-7.23414244016268,-0.0298154996095495,
23.9113882007562));
#31970=CARTESIAN_POINT('Ctrl Pts',(-7.36619019624783,0.563701731054729,
23.9345421216053));
#31971=CARTESIAN_POINT('Ctrl Pts',(-7.75968252106489,1.02723702411681,23.9576960424544));
#31972=CARTESIAN_POINT('Ctrl Pts',(-8.29136160594112,1.24083426807448,23.9795153352526));
#31973=CARTESIAN_POINT('Ctrl Pts',(-8.657569202316,1.21801597484871,23.9936166544345));
#31974=CARTESIAN_POINT('Ctrl Pts',(-8.81482199187077,1.17607957877116,24.));
#31975=CARTESIAN_POINT('Origin',(-8.5,0.,22.1374873996035));
#31976=CARTESIAN_POINT('',(-9.71737930107838,-1.72188272680729E-5,23.4625126003965));
#31977=CARTESIAN_POINT('',(-9.71750618477853,-2.14937489025574E-5,23.4874873996035));
#31978=CARTESIAN_POINT('',(-9.71745,-6.10603367124078E-16,22.1374873996035));
#31979=CARTESIAN_POINT('Ctrl Pts',(-9.71750618477853,-2.1493748902545E-5,
23.4874873996035));
#31980=CARTESIAN_POINT('Ctrl Pts',(-9.71752840630035,-0.0265897893097531,
23.488529513509));
#31981=CARTESIAN_POINT('Ctrl Pts',(-9.71035853514721,-0.249912895433259,
23.4972896010309));
#31982=CARTESIAN_POINT('Ctrl Pts',(-9.57920081330433,-0.662276356417367,
23.5137676621692));
#31983=CARTESIAN_POINT('Ctrl Pts',(-9.14605438936275,-1.08898948282007,
23.5369215830183));
#31984=CARTESIAN_POINT('Ctrl Pts',(-8.56393485826131,-1.26459349261069,
23.5600755038673));
#31985=CARTESIAN_POINT('Ctrl Pts',(-7.96707264494009,-1.14859601343679,
23.5832294247164));
#31986=CARTESIAN_POINT('Ctrl Pts',(-7.49309767679161,-0.767744800604105,
23.6063833455655));
#31987=CARTESIAN_POINT('Ctrl Pts',(-7.2513034195874,-0.209859997254996,
23.6295372664146));
#31988=CARTESIAN_POINT('Ctrl Pts',(-7.29744499763571,0.396416237173858,
23.6526911872637));
#31989=CARTESIAN_POINT('Ctrl Pts',(-7.62088266214053,0.91128320195394,23.6758451081128));
#31990=CARTESIAN_POINT('Ctrl Pts',(-8.14703521692498,1.21601818778867,23.6989990289619));
#31991=CARTESIAN_POINT('Ctrl Pts',(-8.75457759628112,1.24035261140464,23.722152949811));
#31992=CARTESIAN_POINT('Ctrl Pts',(-9.30341717795882,0.978675249789286,
23.74530687066));
#31993=CARTESIAN_POINT('Ctrl Pts',(-9.64539406535925,0.52028354219972,23.7670850205909));
#31994=CARTESIAN_POINT('Ctrl Pts',(-9.71733322183359,0.161675605360226,
23.7811451969054));
#31995=CARTESIAN_POINT('Ctrl Pts',(-9.71748305223155,-2.53287507604727E-5,
23.7874873996035));
#31996=CARTESIAN_POINT('Ctrl Pts',(-9.71737930107839,-1.72188272682325E-5,
23.4625126003965));
#31997=CARTESIAN_POINT('Ctrl Pts',(-9.71741977805662,-0.0761084070319482,
23.4654963018055));
#31998=CARTESIAN_POINT('Ctrl Pts',(-9.69220303304603,-0.348999015684658,
23.4761979768309));
#31999=CARTESIAN_POINT('Ctrl Pts',(-9.49058703805816,-0.788683553714432,
23.4946176254726));
#32000=CARTESIAN_POINT('Ctrl Pts',(-9.0087325233999,-1.15951526402384,23.5177715463217));
#32001=CARTESIAN_POINT('Ctrl Pts',(-8.40956982850905,-1.26297538057999,
23.5409254671708));
#32002=CARTESIAN_POINT('Ctrl Pts',(-7.8312593464559,-1.07520712710119,23.5640793880199));
#32003=CARTESIAN_POINT('Ctrl Pts',(-7.40715317709645,-0.639507818195355,
23.587233308869));
#32004=CARTESIAN_POINT('Ctrl Pts',(-7.23504558492588,-0.0563449701204428,
23.6103872297181));
#32005=CARTESIAN_POINT('Ctrl Pts',(-7.35462270660441,0.539810414542498,
23.6335411505671));
#32006=CARTESIAN_POINT('Ctrl Pts',(-7.73831135994277,1.011491395628,23.6566950714162));
#32007=CARTESIAN_POINT('Ctrl Pts',(-8.2976371195735,1.24993347528822,23.6798489922653));
#32008=CARTESIAN_POINT('Ctrl Pts',(-8.90362555579596,1.20015450597578,23.7030029131144));
#32009=CARTESIAN_POINT('Ctrl Pts',(-9.41654233415426,0.873632976856196,
23.7261568339635));
#32010=CARTESIAN_POINT('Ctrl Pts',(-9.67490694331657,0.421305905434982,
23.7459933963909));
#32011=CARTESIAN_POINT('Ctrl Pts',(-9.71732962480593,0.112217590029651,
23.7581119852019));
#32012=CARTESIAN_POINT('Ctrl Pts',(-9.71736782397678,-1.116610560329E-5,
23.7625126003965));
#32013=CARTESIAN_POINT('Origin',(-8.5,0.,22.1374873996035));
#32014=CARTESIAN_POINT('',(-9.71739547902908,-2.21443075443251E-5,23.1625126003965));
#32015=CARTESIAN_POINT('',(-9.71752593121431,-1.5879371246656E-5,23.1874873996035));
#32016=CARTESIAN_POINT('',(-9.71745,-6.10603367124078E-16,22.1374873996035));
#32017=CARTESIAN_POINT('Ctrl Pts',(-9.71752593121431,-1.5879371246693E-5,
23.1874873996035));
#32018=CARTESIAN_POINT('Ctrl Pts',(-9.71753796375452,-0.0180768671235083,
23.1881958564963));
#32019=CARTESIAN_POINT('Ctrl Pts',(-9.71285129265438,-0.232889135646274,
23.1966222870055));
#32020=CARTESIAN_POINT('Ctrl Pts',(-9.5928468023976,-0.639507806195877,
23.212766691131));
#32021=CARTESIAN_POINT('Ctrl Pts',(-9.16874064099593,-1.07520710692634,
23.2359206119801));
#32022=CARTESIAN_POINT('Ctrl Pts',(-8.59043016979403,-1.26297535688186,
23.2590745328292));
#32023=CARTESIAN_POINT('Ctrl Pts',(-7.99126748614572,-1.15951524226696,
23.2822284536783));
#32024=CARTESIAN_POINT('Ctrl Pts',(-7.5094129805289,-0.788683538915698,
23.3053823745274));
#32025=CARTESIAN_POINT('Ctrl Pts',(-7.25597705495489,-0.235989999581765,
23.3285362953765));
#32026=CARTESIAN_POINT('Ctrl Pts',(-7.28939927415983,0.371120263926209,
23.3516902162256));
#32027=CARTESIAN_POINT('Ctrl Pts',(-7.60197283833471,0.892654235755761,
23.3748441370746));
#32028=CARTESIAN_POINT('Ctrl Pts',(-8.1216216872399,1.20835186106285,23.3979980579237));
#32029=CARTESIAN_POINT('Ctrl Pts',(-8.72852045485104,1.24541670512988,23.4211519787728));
#32030=CARTESIAN_POINT('Ctrl Pts',(-9.28272489396535,0.99530201851838,23.4443058996219));
#32031=CARTESIAN_POINT('Ctrl Pts',(-9.63962122283735,0.537268329942552,
23.4664177065655));
#32032=CARTESIAN_POINT('Ctrl Pts',(-9.71736383204584,0.170176997010107,
23.4808115398927));
#32033=CARTESIAN_POINT('Ctrl Pts',(-9.71750618477853,-2.1493748902545E-5,
23.4874873996035));
#32034=CARTESIAN_POINT('Ctrl Pts',(-9.71739547902908,-2.21443075442973E-5,
23.1625126003965));
#32035=CARTESIAN_POINT('Ctrl Pts',(-9.71744265125785,-0.0676017388760646,
23.1651626447928));
#32036=CARTESIAN_POINT('Ctrl Pts',(-9.69577268601838,-0.331969805738998,
23.1755306628055));
#32037=CARTESIAN_POINT('Ctrl Pts',(-9.50690234210182,-0.767744815010462,
23.1936166544345));
#32038=CARTESIAN_POINT('Ctrl Pts',(-9.03292736505941,-1.14859603498855,
23.2167705752836));
#32039=CARTESIAN_POINT('Ctrl Pts',(-8.436065140539,-1.2645935163393,23.2399244961327));
#32040=CARTESIAN_POINT('Ctrl Pts',(-7.85394559851473,-1.08898950325348,
23.2630784169817));
#32041=CARTESIAN_POINT('Ctrl Pts',(-7.42079916644579,-0.662276368844085,
23.2862323378308));
#32042=CARTESIAN_POINT('Ctrl Pts',(-7.23650469503931,-0.0828495154220059,
23.3093862586799));
#32043=CARTESIAN_POINT('Ctrl Pts',(-7.34355848256139,0.515681534104197,
23.332540179529));
#32044=CARTESIAN_POINT('Ctrl Pts',(-7.71727509134788,0.995302037194035,
23.3556941003781));
#32045=CARTESIAN_POINT('Ctrl Pts',(-8.27147954086117,1.24541672849857,23.3788480212272));
#32046=CARTESIAN_POINT('Ctrl Pts',(-8.87837831986,1.20835188373602,23.4020019420763));
#32047=CARTESIAN_POINT('Ctrl Pts',(-9.39802717851571,0.892654252505216,
23.4251558629254));
#32048=CARTESIAN_POINT('Ctrl Pts',(-9.67032134156336,0.438327103198321,
23.4453260823654));
#32049=CARTESIAN_POINT('Ctrl Pts',(-9.71731507580687,0.120717515705654,
23.4577783281892));
#32050=CARTESIAN_POINT('Ctrl Pts',(-9.71737930107839,-1.72188272682325E-5,
23.4625126003965));
#32051=CARTESIAN_POINT('Origin',(-8.5,0.,22.1374873996035));
#32052=CARTESIAN_POINT('',(-9.71741556519039,-3.134158932111E-5,22.8625126003965));
#32053=CARTESIAN_POINT('',(-9.71754008709556,-8.82674686203209E-6,22.8874873996035));
#32054=CARTESIAN_POINT('',(-9.71745,-6.10603367124078E-16,22.1374873996035));
#32055=CARTESIAN_POINT('',(-8.8147888955045,1.1760495116138,22.8));
#32056=CARTESIAN_POINT('Ctrl Pts',(-8.81478889550448,1.17604951161381,22.8));
#32057=CARTESIAN_POINT('Ctrl Pts',(-9.00489125583834,1.12516550422183,22.8077179736164));
#32058=CARTESIAN_POINT('Ctrl Pts',(-9.35978561312172,0.929509121580238,
22.8231539208491));
#32059=CARTESIAN_POINT('Ctrl Pts',(-9.66055719692335,0.472338673167377,
22.8439914543146));
#32060=CARTESIAN_POINT('Ctrl Pts',(-9.71730336395768,0.137706364168718,
22.8571110141637));
#32061=CARTESIAN_POINT('Ctrl Pts',(-9.71741556519039,-3.13415893210822E-5,
22.8625126003965));
#32062=CARTESIAN_POINT('',(-8.18517800353966,1.17607954763525,22.8));
#32063=CARTESIAN_POINT('Origin',(-8.5,0.,22.8));
#32064=CARTESIAN_POINT('Ctrl Pts',(-8.18517800353966,1.17607954763525,22.8));
#32065=CARTESIAN_POINT('Ctrl Pts',(-8.34243079339873,1.2180159458478,22.8063833455655));
#32066=CARTESIAN_POINT('Ctrl Pts',(-8.70863838400351,1.24083423778419,22.8204846647474));
#32067=CARTESIAN_POINT('Ctrl Pts',(-9.24031746415369,1.02723700478738,22.8423039575456));
#32068=CARTESIAN_POINT('Ctrl Pts',(-9.62744019623509,0.57120511221857,22.8650830785146));
#32069=CARTESIAN_POINT('Ctrl Pts',(-9.71746386067399,0.187187389102954,
22.8801442258672));
#32070=CARTESIAN_POINT('Ctrl Pts',(-9.71754008709556,-8.82674686206349E-6,
22.8874873996035));
#32071=CARTESIAN_POINT('Origin',(-8.5,0.,22.1374873996035));
#32072=CARTESIAN_POINT('Ctrl Pts',(-9.71754008709556,-8.82674686206349E-6,
22.8874873996035));
#32073=CARTESIAN_POINT('Ctrl Pts',(-9.71754397773668,-0.0095634310334148,
22.8878621994836));
#32074=CARTESIAN_POINT('Ctrl Pts',(-9.71516332688261,-0.215866916824623,
22.8959549729801));
#32075=CARTESIAN_POINT('Ctrl Pts',(-9.6060125223886,-0.616458272121094,
22.9117657200929));
#32076=CARTESIAN_POINT('Ctrl Pts',(-9.19113298264395,-1.06095215983846,
22.934919640942));
#32077=CARTESIAN_POINT('Ctrl Pts',(-8.61688574282532,-1.26080217699431,
22.9580735617911));
#32078=CARTESIAN_POINT('Ctrl Pts',(-8.01568590595785,-1.16992487427985,
22.9812274826402));
#32079=CARTESIAN_POINT('Ctrl Pts',(-7.52616363366338,-0.809275665471485,
23.0043814034893));
#32080=CARTESIAN_POINT('Ctrl Pts',(-7.26119741948789,-0.262016286526366,
23.0275353243383));
#32081=CARTESIAN_POINT('Ctrl Pts',(-7.28188559259607,0.345661188566822,
23.0506892451874));
#32082=CARTESIAN_POINT('Ctrl Pts',(-7.58345768304373,0.873632960464764,
23.0738431660365));
#32083=CARTESIAN_POINT('Ctrl Pts',(-8.09637445177758,1.20015448345588,23.0969970868856));
#32084=CARTESIAN_POINT('Ctrl Pts',(-8.70236287662956,1.24993345183503,23.1201510077347));
#32085=CARTESIAN_POINT('Ctrl Pts',(-9.26168862576517,1.01149137664845,23.1433049285838));
#32086=CARTESIAN_POINT('Ctrl Pts',(-9.63363727901798,0.554242760737588,
23.1657503925401));
#32087=CARTESIAN_POINT('Ctrl Pts',(-9.7174068805104,0.178680660921264,23.18047788288));
#32088=CARTESIAN_POINT('Ctrl Pts',(-9.71752593121431,-1.5879371246693E-5,
23.1874873996035));
#32089=CARTESIAN_POINT('Ctrl Pts',(-9.71741556519039,-3.13415893210822E-5,
22.8625126003965));
#32090=CARTESIAN_POINT('Ctrl Pts',(-9.71746368096762,-0.0590980435010754,
22.8648289877801));
#32091=CARTESIAN_POINT('Ctrl Pts',(-9.69914933317854,-0.314939569855699,
22.87486334878));
#32092=CARTESIAN_POINT('Ctrl Pts',(-9.5227777403229,-0.746471923361528,
22.8926156833964));
#32093=CARTESIAN_POINT('Ctrl Pts',(-9.05688665443706,-1.13717116763217,
22.9157696042454));
#32094=CARTESIAN_POINT('Ctrl Pts',(-8.46258911977101,-1.2656564697317,22.9389235250945));
#32095=CARTESIAN_POINT('Ctrl Pts',(-7.87691550790518,-1.10229307735719,
22.9620774459436));
#32096=CARTESIAN_POINT('Ctrl Pts',(-7.43491956993902,-0.684753972836506,
22.9852313667927));
#32097=CARTESIAN_POINT('Ctrl Pts',(-7.23851903592649,-0.109317603314454,
23.0083852876418));
#32098=CARTESIAN_POINT('Ctrl Pts',(-7.33300252317075,0.49132599619855,23.0315392084909));
#32099=CARTESIAN_POINT('Ctrl Pts',(-7.69658280697753,0.978675268097788,
23.05469312934));
#32100=CARTESIAN_POINT('Ctrl Pts',(-8.24542239893397,1.24035263469515,23.077847050189));
#32101=CARTESIAN_POINT('Ctrl Pts',(-8.85296478970154,1.21601821059452,23.1010009710381));
#32102=CARTESIAN_POINT('Ctrl Pts',(-9.37911735435305,0.911283219057196,
23.1241548918872));
#32103=CARTESIAN_POINT('Ctrl Pts',(-9.66553649178147,0.455344507747716,
23.14465876834));
#32104=CARTESIAN_POINT('Ctrl Pts',(-9.71730526713794,0.129216672397783,
23.1574446711764));
#32105=CARTESIAN_POINT('Ctrl Pts',(-9.71739547902908,-2.21443075442973E-5,
23.1625126003965));
#32106=CARTESIAN_POINT('Ctrl Pts',(-7.70661869325984,-0.687936125025627,
22.8));
#32107=CARTESIAN_POINT('Ctrl Pts',(-7.59541735366076,-0.559690113640355,
22.8077179736164));
#32108=CARTESIAN_POINT('Ctrl Pts',(-7.43648140164231,-0.248364568035598,
22.8231539208491));
#32109=CARTESIAN_POINT('Ctrl Pts',(-7.4433094346916,0.276076273974975,22.8463078416982));
#32110=CARTESIAN_POINT('Ctrl Pts',(-7.69382595960932,0.736800949934783,
22.8694617625473));
#32111=CARTESIAN_POINT('Ctrl Pts',(-8.13023253692469,1.0276599848185,22.8926156833964));
#32112=CARTESIAN_POINT('Ctrl Pts',(-8.65190804663029,1.08153909597928,22.9157696042454));
#32113=CARTESIAN_POINT('Ctrl Pts',(-9.13855383720711,0.886033577335599,
22.9389235250945));
#32114=CARTESIAN_POINT('Ctrl Pts',(-9.47795691943568,0.486215594288713,
22.9620774459436));
#32115=CARTESIAN_POINT('Ctrl Pts',(-9.59185346304236,-0.0257170769795772,
22.9852313667927));
#32116=CARTESIAN_POINT('Ctrl Pts',(-9.45398065609287,-0.531720260835648,
23.0083852876418));
#32117=CARTESIAN_POINT('Ctrl Pts',(-9.09613022717517,-0.915114265921696,
23.0315392084909));
#32118=CARTESIAN_POINT('Ctrl Pts',(-8.60081869361441,-1.08749301085197,
23.05469312934));
#32119=CARTESIAN_POINT('Ctrl Pts',(-8.08225945200734,-1.00910765163355,
23.077847050189));
#32120=CARTESIAN_POINT('Ctrl Pts',(-7.66002663904875,-0.698033082518055,
23.1010009710381));
#32121=CARTESIAN_POINT('Ctrl Pts',(-7.43148253333133,-0.225999673482555,
23.1241548918872));
#32122=CARTESIAN_POINT('Ctrl Pts',(-7.44932692166836,0.298146793801815,
23.1473088127363));
#32123=CARTESIAN_POINT('Ctrl Pts',(-7.70944508026138,0.753543859529384,
23.1704627335854));
#32124=CARTESIAN_POINT('Ctrl Pts',(-8.15185659518801,1.03518191554233,23.1936166544345));
#32125=CARTESIAN_POINT('Ctrl Pts',(-8.67454618813808,1.0781182946092,23.2167705752836));
#32126=CARTESIAN_POINT('Ctrl Pts',(-9.15698733082756,0.87245233448481,23.2399244961327));
#32127=CARTESIAN_POINT('Ctrl Pts',(-9.48793434902992,0.465608366400854,
23.2630784169817));
#32128=CARTESIAN_POINT('Ctrl Pts',(-9.59107446412167,-0.0485998209482193,
23.2862323378308));
#32129=CARTESIAN_POINT('Ctrl Pts',(-9.44262468865063,-0.551601418773905,
23.3093862586799));
#32130=CARTESIAN_POINT('Ctrl Pts',(-9.07681592435815,-0.927409735909772,
23.332540179529));
#32131=CARTESIAN_POINT('Ctrl Pts',(-8.57799968894059,-1.08936746664063,
23.3556941003781));
#32132=CARTESIAN_POINT('Ctrl Pts',(-8.06119757460399,-1.00012892184856,
23.3788480212272));
#32133=CARTESIAN_POINT('Ctrl Pts',(-7.64557852137944,-0.680271538227749,
23.4020019420763));
#32134=CARTESIAN_POINT('Ctrl Pts',(-7.4269797572041,-0.203550945468653,
23.4251558629254));
#32135=CARTESIAN_POINT('Ctrl Pts',(-7.45580777674256,0.320106278819592,
23.4483097837744));
#32136=CARTESIAN_POINT('Ctrl Pts',(-7.72541515260198,0.769950480896237,
23.4714637046235));
#32137=CARTESIAN_POINT('Ctrl Pts',(-8.17363335970316,1.04225248618185,23.4946176254726));
#32138=CARTESIAN_POINT('Ctrl Pts',(-8.69710816020295,1.07422241739446,23.5177715463217));
#32139=CARTESIAN_POINT('Ctrl Pts',(-9.17513196529879,0.85848835652072,23.5409254671708));
#32140=CARTESIAN_POINT('Ctrl Pts',(-9.49747769080951,0.444796228840474,
23.5640793880199));
#32141=CARTESIAN_POINT('Ctrl Pts',(-9.58981592249665,-0.0714610657623065,
23.587233308869));
#32142=CARTESIAN_POINT('Ctrl Pts',(-9.43085446962986,-0.571240216743092,
23.6103872297181));
#32143=CARTESIAN_POINT('Ctrl Pts',(-9.05724811225909,-0.939297594077255,
23.6335411505671));
#32144=CARTESIAN_POINT('Ctrl Pts',(-8.55514640819762,-1.090763174332,23.6566950714162));
#32145=CARTESIAN_POINT('Ctrl Pts',(-8.0403285428162,-0.990710644141418,
23.6798489922653));
#32146=CARTESIAN_POINT('Ctrl Pts',(-7.63150591022126,-0.662211027240847,
23.7030029131144));
#32147=CARTESIAN_POINT('Ctrl Pts',(-7.42294855715531,-0.181012758731342,
23.7261568339635));
#32148=CARTESIAN_POINT('Ctrl Pts',(-7.46274753954353,0.341925081651212,
23.7493107548126));
#32149=CARTESIAN_POINT('Ctrl Pts',(-7.74172564254284,0.786018719760016,
23.7724646756617));
#32150=CARTESIAN_POINT('Ctrl Pts',(-8.19555355972969,1.04886500389904,23.7956185965107));
#32151=CARTESIAN_POINT('Ctrl Pts',(-8.71958350146191,1.06985443117665,23.8187725173598));
#32152=CARTESIAN_POINT('Ctrl Pts',(-9.19297989944109,0.844147094175308,
23.8419264382089));
#32153=CARTESIAN_POINT('Ctrl Pts',(-9.50658263369233,0.423788589976583,
23.865080359058));
#32154=CARTESIAN_POINT('Ctrl Pts',(-9.588078471842,-0.0942908643321087,
23.8882342799071));
#32155=CARTESIAN_POINT('Ctrl Pts',(-9.41867504905042,-0.5906280615228,23.9113882007562));
#32156=CARTESIAN_POINT('Ctrl Pts',(-9.03743563417062,-0.950772464644027,
23.9345421216053));
#32157=CARTESIAN_POINT('Ctrl Pts',(-8.53226840022093,-1.09168001425565,
23.9576960424544));
#32158=CARTESIAN_POINT('Ctrl Pts',(-8.01966268339815,-0.980856224450063,
23.9808499633034));
#32159=CARTESIAN_POINT('Ctrl Pts',(-7.61781273252235,-0.643862288262505,
24.0040038841525));
#32160=CARTESIAN_POINT('Ctrl Pts',(-7.41939648367848,-0.158392751533025,
24.0271578050016));
#32161=CARTESIAN_POINT('Ctrl Pts',(-7.47013328830288,0.363576148835214,
24.0503117258507));
#32162=CARTESIAN_POINT('Ctrl Pts',(-7.758400006739,0.801739494913083,24.0734656466998));
#32163=CARTESIAN_POINT('Ctrl Pts',(-8.06451081542918,0.970500879693935,
24.0889015939325));
#32164=CARTESIAN_POINT('Ctrl Pts',(-8.22848181102373,1.0143903997254,24.0966195675489));
#32165=CARTESIAN_POINT('Ctrl Pts',(-7.66447275106926,-0.724480616192512,
22.7677934774837));
#32166=CARTESIAN_POINT('Ctrl Pts',(-7.54736418225966,-0.589421929822215,
22.7755114511001));
#32167=CARTESIAN_POINT('Ctrl Pts',(-7.37998524653481,-0.261558171965623,
22.7909473983328));
#32168=CARTESIAN_POINT('Ctrl Pts',(-7.38717599784293,0.290741977066652,
22.8141013191819));
#32169=CARTESIAN_POINT('Ctrl Pts',(-7.65100044278255,0.775941234660551,
22.837255240031));
#32170=CARTESIAN_POINT('Ctrl Pts',(-8.11058977752221,1.0822512613507,22.8604091608801));
#32171=CARTESIAN_POINT('Ctrl Pts',(-8.65997769447449,1.13899253460802,22.8835630817292));
#32172=CARTESIAN_POINT('Ctrl Pts',(-9.1724750461893,0.933101386486192,22.9067170025782));
#32173=CARTESIAN_POINT('Ctrl Pts',(-9.52990787346151,0.512044302571802,
22.9298709234273));
#32174=CARTESIAN_POINT('Ctrl Pts',(-9.64985482070358,-0.0270832176114321,
22.9530248442764));
#32175=CARTESIAN_POINT('Ctrl Pts',(-9.50465794485812,-0.559966264597463,
22.9761787651255));
#32176=CARTESIAN_POINT('Ctrl Pts',(-9.12779781233143,-0.963726897227285,
22.9993326859746));
#32177=CARTESIAN_POINT('Ctrl Pts',(-8.60617437668471,-1.14526273289942,
23.0224866068237));
#32178=CARTESIAN_POINT('Ctrl Pts',(-8.06006826999085,-1.06271339251565,
23.0456405276728));
#32179=CARTESIAN_POINT('Ctrl Pts',(-7.61540563725363,-0.735113943502532,
23.0687944485218));
#32180=CARTESIAN_POINT('Ctrl Pts',(-7.37472082871686,-0.238005211163826,
23.0919483693709));
#32181=CARTESIAN_POINT('Ctrl Pts',(-7.39351314531093,0.313984925390151,
23.11510229022));
#32182=CARTESIAN_POINT('Ctrl Pts',(-7.66744928118883,0.793573559841177,
23.1382562110691));
#32183=CARTESIAN_POINT('Ctrl Pts',(-8.13336254738453,1.09017277151351,23.1614101319182));
#32184=CARTESIAN_POINT('Ctrl Pts',(-8.68381841763523,1.13539001368448,23.1845640527673));
#32185=CARTESIAN_POINT('Ctrl Pts',(-9.19188776247343,0.918798681872689,
23.2077179736164));
#32186=CARTESIAN_POINT('Ctrl Pts',(-9.54041532332131,0.490342379071769,
23.2308718944654));
#32187=CARTESIAN_POINT('Ctrl Pts',(-9.64903443986073,-0.0511815369865916,
23.2540258153145));
#32188=CARTESIAN_POINT('Ctrl Pts',(-9.49269872656629,-0.580903547914563,
23.2771797361636));
#32189=CARTESIAN_POINT('Ctrl Pts',(-9.10745749657075,-0.976675526248629,
23.3003336570127));
#32190=CARTESIAN_POINT('Ctrl Pts',(-8.58214318255841,-1.14723676338771,
23.3234875778618));
#32191=CARTESIAN_POINT('Ctrl Pts',(-8.0378875451179,-1.05325769532136,23.3466414987109));
#32192=CARTESIAN_POINT('Ctrl Pts',(-7.60019000776259,-0.716408871790399,
23.36979541956));
#32193=CARTESIAN_POINT('Ctrl Pts',(-7.36997885645436,-0.214363963506357,
23.3929493404091));
#32194=CARTESIAN_POINT('Ctrl Pts',(-7.40033827588165,0.337110940521798,
23.4161032612582));
#32195=CARTESIAN_POINT('Ctrl Pts',(-7.68426771451289,0.810851732516078,
23.4392571821072));
#32196=CARTESIAN_POINT('Ctrl Pts',(-8.15629613554874,1.09761894447552,23.4624111029563));
#32197=CARTESIAN_POINT('Ctrl Pts',(-8.70757892508565,1.13128717997293,23.4855650238054));
#32198=CARTESIAN_POINT('Ctrl Pts',(-9.21099627485431,0.90409291051994,23.5087189446545));
#32199=CARTESIAN_POINT('Ctrl Pts',(-9.55046562578617,0.468424660702981,
23.5318728655036));
#32200=CARTESIAN_POINT('Ctrl Pts',(-9.64770904208202,-0.075257215130723,
23.5550267863527));
#32201=CARTESIAN_POINT('Ctrl Pts',(-9.48030325085468,-0.601585596634517,
23.5781807072018));
#32202=CARTESIAN_POINT('Ctrl Pts',(-9.08685020462698,-0.989194890324859,
23.6013346280509));
#32203=CARTESIAN_POINT('Ctrl Pts',(-8.55807589155219,-1.14870661375823,
23.6244885488999));
#32204=CARTESIAN_POINT('Ctrl Pts',(-8.01590991019083,-1.04333910057321,
23.647642469749));
#32205=CARTESIAN_POINT('Ctrl Pts',(-7.58536983241137,-0.697388951695266,
23.6707963905981));
#32206=CARTESIAN_POINT('Ctrl Pts',(-7.36573351129933,-0.190628504905893,
23.6939503114472));
#32207=CARTESIAN_POINT('Ctrl Pts',(-7.40764669224092,0.360088800158761,
23.7171042322963));
#32208=CARTESIAN_POINT('Ctrl Pts',(-7.7014446490754,0.82777354715799,23.7402581531454));
#32209=CARTESIAN_POINT('Ctrl Pts',(-8.17938077879479,1.10458273186225,23.7634120739945));
#32210=CARTESIAN_POINT('Ctrl Pts',(-8.73124819973498,1.12668715791932,23.7865659948435));
#32211=CARTESIAN_POINT('Ctrl Pts',(-9.22979232561366,0.888989812713301,
23.8097199156926));
#32212=CARTESIAN_POINT('Ctrl Pts',(-9.560054240761,0.446301055625118,23.8328738365417));
#32213=CARTESIAN_POINT('Ctrl Pts',(-9.64587929470419,-0.0992997765455415,
23.8560277573908));
#32214=CARTESIAN_POINT('Ctrl Pts',(-9.46747683600994,-0.622003361048509,
23.8791816782399));
#32215=CARTESIAN_POINT('Ctrl Pts',(-9.06598524956549,-1.00127932810407,
23.902335599089));
#32216=CARTESIAN_POINT('Ctrl Pts',(-8.53398255975398,-1.14967215798345,
23.9254895199381));
#32217=CARTESIAN_POINT('Ctrl Pts',(-7.99414624054086,-1.03296119513911,
23.9486434407871));
#32218=CARTESIAN_POINT('Ctrl Pts',(-7.57094924675516,-0.67806549238298,
23.9717973616362));
#32219=CARTESIAN_POINT('Ctrl Pts',(-7.36199274484205,-0.166806879384039,
23.9949512824853));
#32220=CARTESIAN_POINT('Ctrl Pts',(-7.41542478619117,0.382890013707631,
24.0181052033344));
#32221=CARTESIAN_POINT('Ctrl Pts',(-7.71900478759408,0.844329440148046,
24.0412591241835));
#32222=CARTESIAN_POINT('Ctrl Pts',(-8.04137679167337,1.02205575453658,24.0566950714162));
#32223=CARTESIAN_POINT('Ctrl Pts',(-8.21405824218102,1.06827677035487,24.0644130450326));
#32224=CARTESIAN_POINT('Ctrl Pts',(-7.62232680887869,-0.761025107359397,
22.7355869549674));
#32225=CARTESIAN_POINT('Ctrl Pts',(-7.49931101085856,-0.619153746004075,
22.7433049285838));
#32226=CARTESIAN_POINT('Ctrl Pts',(-7.32348909142731,-0.274751775895648,
22.7587408758165));
#32227=CARTESIAN_POINT('Ctrl Pts',(-7.33104256099426,0.305407680158331,
22.7818947966656));
#32228=CARTESIAN_POINT('Ctrl Pts',(-7.60817492595577,0.815081519386318,
22.8050487175147));
#32229=CARTESIAN_POINT('Ctrl Pts',(-8.09094701811972,1.13684253788289,22.8282026383638));
#32230=CARTESIAN_POINT('Ctrl Pts',(-8.66804734231868,1.19644597323676,22.8513565592128));
#32231=CARTESIAN_POINT('Ctrl Pts',(-9.2063962551715,0.980169195636786,22.8745104800619));
#32232=CARTESIAN_POINT('Ctrl Pts',(-9.58185882748734,0.537873010854892,
22.897664400911));
#32233=CARTESIAN_POINT('Ctrl Pts',(-9.70785617836479,-0.0284493582432865,
22.9208183217601));
#32234=CARTESIAN_POINT('Ctrl Pts',(-9.55533523362336,-0.588212268359279,
22.9439722426092));
#32235=CARTESIAN_POINT('Ctrl Pts',(-9.15946539748769,-1.01233952853287,
22.9671261634583));
#32236=CARTESIAN_POINT('Ctrl Pts',(-8.61153005975502,-1.20303245494687,
22.9902800843074));
#32237=CARTESIAN_POINT('Ctrl Pts',(-8.03787708797435,-1.11631913339775,
23.0134340051565));
#32238=CARTESIAN_POINT('Ctrl Pts',(-7.5707846354585,-0.772194804487008,
23.0365879260055));
#32239=CARTESIAN_POINT('Ctrl Pts',(-7.31795912410237,-0.250010748845096,
23.0597418468546));
#32240=CARTESIAN_POINT('Ctrl Pts',(-7.3376993689535,0.329823056978487,23.0828957677037));
#32241=CARTESIAN_POINT('Ctrl Pts',(-7.62545348211628,0.83360326015297,23.1060496885528));
#32242=CARTESIAN_POINT('Ctrl Pts',(-8.11486849958106,1.1451636274847,23.1292036094019));
#32243=CARTESIAN_POINT('Ctrl Pts',(-8.69309064713239,1.19266173275976,23.152357530251));
#32244=CARTESIAN_POINT('Ctrl Pts',(-9.2267881941193,0.965145029260567,23.1755114511001));
#32245=CARTESIAN_POINT('Ctrl Pts',(-9.59289629761269,0.515076391742683,
23.1986653719492));
#32246=CARTESIAN_POINT('Ctrl Pts',(-9.70699441559979,-0.0537632530249641,
23.2218192927982));
#32247=CARTESIAN_POINT('Ctrl Pts',(-9.54277276448194,-0.61020567705522,
23.2449732136473));
#32248=CARTESIAN_POINT('Ctrl Pts',(-9.13809906878334,-1.02594131658749,
23.2681271344964));
#32249=CARTESIAN_POINT('Ctrl Pts',(-8.58628667617622,-1.20510606013478,
23.2912810553455));
#32250=CARTESIAN_POINT('Ctrl Pts',(-8.01457751563181,-1.10638646879416,
23.3144349761946));
#32251=CARTESIAN_POINT('Ctrl Pts',(-7.55480149414575,-0.752546205353048,
23.3375888970437));
#32252=CARTESIAN_POINT('Ctrl Pts',(-7.31297795570463,-0.225176981544062,
23.3607428178928));
#32253=CARTESIAN_POINT('Ctrl Pts',(-7.34486877502074,0.354115602224003,
23.3838967387419));
#32254=CARTESIAN_POINT('Ctrl Pts',(-7.6431202764238,0.85175298413592,23.4070506595909));
#32255=CARTESIAN_POINT('Ctrl Pts',(-8.13895891139432,1.15298540276918,23.43020458044));
#32256=CARTESIAN_POINT('Ctrl Pts',(-8.71804968996834,1.18835194255141,23.4533585012891));
#32257=CARTESIAN_POINT('Ctrl Pts',(-9.24686058440983,0.94969746451916,23.4765124221382));
#32258=CARTESIAN_POINT('Ctrl Pts',(-9.60345356076283,0.492053092565487,
23.4996663429873));
#32259=CARTESIAN_POINT('Ctrl Pts',(-9.7056021616674,-0.079053364499139,
23.5228202638364));
#32260=CARTESIAN_POINT('Ctrl Pts',(-9.52975203207951,-0.631930976525942,
23.5459741846855));
#32261=CARTESIAN_POINT('Ctrl Pts',(-9.11645229699486,-1.03909218657246,
23.5691281055346));
#32262=CARTESIAN_POINT('Ctrl Pts',(-8.56100537490675,-1.20665005318446,
23.5922820263836));
#32263=CARTESIAN_POINT('Ctrl Pts',(-7.99149127756545,-1.095967557005,23.6154359472327));
#32264=CARTESIAN_POINT('Ctrl Pts',(-7.53923375460149,-0.732566876149685,
23.6385898680818));
#32265=CARTESIAN_POINT('Ctrl Pts',(-7.30851846544336,-0.200244251080445,
23.6617437889309));
#32266=CARTESIAN_POINT('Ctrl Pts',(-7.35254584493832,0.37825251866631,23.68489770978));
#32267=CARTESIAN_POINT('Ctrl Pts',(-7.66116365560797,0.869528374555965,
23.7080516306291));
#32268=CARTESIAN_POINT('Ctrl Pts',(-8.16320799785988,1.16030045982546,23.7312055514782));
#32269=CARTESIAN_POINT('Ctrl Pts',(-8.74291289800805,1.18351988466198,23.7543594723273));
#32270=CARTESIAN_POINT('Ctrl Pts',(-9.26660475178623,0.933832531251294,
23.7775133931763));
#32271=CARTESIAN_POINT('Ctrl Pts',(-9.61352584782966,0.468813521273654,
23.8006673140254));
#32272=CARTESIAN_POINT('Ctrl Pts',(-9.70368011756638,-0.104308688758975,
23.8238212348745));
#32273=CARTESIAN_POINT('Ctrl Pts',(-9.51627862296947,-0.653378660574218,
23.8469751557236));
#32274=CARTESIAN_POINT('Ctrl Pts',(-9.09453486496036,-1.05178619156412,
23.8701290765727));
#32275=CARTESIAN_POINT('Ctrl Pts',(-8.53569671928704,-1.20766430171125,
23.8932829974218));
#32276=CARTESIAN_POINT('Ctrl Pts',(-7.96862979768357,-1.08506616582817,
23.9164369182709));
#32277=CARTESIAN_POINT('Ctrl Pts',(-7.52408576098797,-0.712268696503455,
23.93959083912));
#32278=CARTESIAN_POINT('Ctrl Pts',(-7.30458900600562,-0.175221007235054,
23.962744759969));
#32279=CARTESIAN_POINT('Ctrl Pts',(-7.36071628407946,0.402203878580047,
23.9858986808181));
#32280=CARTESIAN_POINT('Ctrl Pts',(-7.67960956844917,0.886919385383009,
24.0090526016672));
#32281=CARTESIAN_POINT('Ctrl Pts',(-8.01824276791756,1.07361062937922,24.0244885488999));
#32282=CARTESIAN_POINT('Ctrl Pts',(-8.19963467333832,1.12216314098435,24.0322065225163));
#32283=CARTESIAN_POINT('Ctrl Pts',(-7.58018086668812,-0.797569598526283,
22.7033804324511));
#32284=CARTESIAN_POINT('Ctrl Pts',(-7.45125783945747,-0.648885562185935,
22.7110984060675));
#32285=CARTESIAN_POINT('Ctrl Pts',(-7.26699293631981,-0.287945379825673,
22.7265343533002));
#32286=CARTESIAN_POINT('Ctrl Pts',(-7.27490912414559,0.320073383250008,
22.7496882741493));
#32287=CARTESIAN_POINT('Ctrl Pts',(-7.565349409129,0.854221804112086,22.7728421949984));
#32288=CARTESIAN_POINT('Ctrl Pts',(-8.07130425871723,1.19143381441509,22.7959961158475));
#32289=CARTESIAN_POINT('Ctrl Pts',(-8.67611699016288,1.25389941186551,22.8191500366966));
#32290=CARTESIAN_POINT('Ctrl Pts',(-9.24031746415369,1.02723700478738,22.8423039575456));
#32291=CARTESIAN_POINT('Ctrl Pts',(-9.63380978151316,0.563701719137981,
22.8654578783947));
#32292=CARTESIAN_POINT('Ctrl Pts',(-9.76585753602602,-0.0298154988751415,
22.8886117992438));
#32293=CARTESIAN_POINT('Ctrl Pts',(-9.6060125223886,-0.616458272121094,
22.9117657200929));
#32294=CARTESIAN_POINT('Ctrl Pts',(-9.19113298264395,-1.06095215983846,
22.934919640942));
#32295=CARTESIAN_POINT('Ctrl Pts',(-8.61688574282532,-1.26080217699431,
22.9580735617911));
#32296=CARTESIAN_POINT('Ctrl Pts',(-8.01568590595785,-1.16992487427985,
22.9812274826402));
#32297=CARTESIAN_POINT('Ctrl Pts',(-7.52616363366338,-0.809275665471485,
23.0043814034893));
#32298=CARTESIAN_POINT('Ctrl Pts',(-7.26119741948789,-0.262016286526366,
23.0275353243383));
#32299=CARTESIAN_POINT('Ctrl Pts',(-7.28188559259607,0.345661188566822,
23.0506892451874));
#32300=CARTESIAN_POINT('Ctrl Pts',(-7.58345768304373,0.873632960464764,
23.0738431660365));
#32301=CARTESIAN_POINT('Ctrl Pts',(-8.09637445177758,1.20015448345588,23.0969970868856));
#32302=CARTESIAN_POINT('Ctrl Pts',(-8.70236287662956,1.24993345183503,23.1201510077347));
#32303=CARTESIAN_POINT('Ctrl Pts',(-9.26168862576517,1.01149137664845,23.1433049285838));
#32304=CARTESIAN_POINT('Ctrl Pts',(-9.64537727190408,0.539810404413598,
23.1664588494329));
#32305=CARTESIAN_POINT('Ctrl Pts',(-9.76495439133885,-0.0563449690633367,
23.189612770282));
#32306=CARTESIAN_POINT('Ctrl Pts',(-9.5928468023976,-0.639507806195877,
23.212766691131));
#32307=CARTESIAN_POINT('Ctrl Pts',(-9.16874064099593,-1.07520710692634,
23.2359206119801));
#32308=CARTESIAN_POINT('Ctrl Pts',(-8.59043016979403,-1.26297535688186,
23.2590745328292));
#32309=CARTESIAN_POINT('Ctrl Pts',(-7.99126748614572,-1.15951524226696,
23.2822284536783));
#32310=CARTESIAN_POINT('Ctrl Pts',(-7.5094129805289,-0.788683538915698,
23.3053823745274));
#32311=CARTESIAN_POINT('Ctrl Pts',(-7.25597705495489,-0.235989999581765,
23.3285362953765));
#32312=CARTESIAN_POINT('Ctrl Pts',(-7.28939927415983,0.371120263926209,
23.3516902162256));
#32313=CARTESIAN_POINT('Ctrl Pts',(-7.60197283833471,0.892654235755761,
23.3748441370746));
#32314=CARTESIAN_POINT('Ctrl Pts',(-8.1216216872399,1.20835186106285,23.3979980579237));
#32315=CARTESIAN_POINT('Ctrl Pts',(-8.72852045485104,1.24541670512988,23.4211519787728));
#32316=CARTESIAN_POINT('Ctrl Pts',(-9.28272489396535,0.99530201851838,23.4443058996219));
#32317=CARTESIAN_POINT('Ctrl Pts',(-9.65644149573949,0.515681524427994,
23.467459820471));
#32318=CARTESIAN_POINT('Ctrl Pts',(-9.76349528125278,-0.0828495138675556,
23.4906137413201));
#32319=CARTESIAN_POINT('Ctrl Pts',(-9.57920081330433,-0.662276356417367,
23.5137676621692));
#32320=CARTESIAN_POINT('Ctrl Pts',(-9.14605438936275,-1.08898948282007,
23.5369215830183));
#32321=CARTESIAN_POINT('Ctrl Pts',(-8.56393485826131,-1.26459349261069,
23.5600755038673));
#32322=CARTESIAN_POINT('Ctrl Pts',(-7.96707264494009,-1.14859601343679,
23.5832294247164));
#32323=CARTESIAN_POINT('Ctrl Pts',(-7.49309767679161,-0.767744800604105,
23.6063833455655));
#32324=CARTESIAN_POINT('Ctrl Pts',(-7.2513034195874,-0.209859997254996,
23.6295372664146));
#32325=CARTESIAN_POINT('Ctrl Pts',(-7.29744499763571,0.396416237173858,
23.6526911872637));
#32326=CARTESIAN_POINT('Ctrl Pts',(-7.62088266214053,0.91128320195394,23.6758451081128));
#32327=CARTESIAN_POINT('Ctrl Pts',(-8.14703521692498,1.21601818778867,23.6989990289619));
#32328=CARTESIAN_POINT('Ctrl Pts',(-8.75457759628112,1.24035261140464,23.722152949811));
#32329=CARTESIAN_POINT('Ctrl Pts',(-9.30341717795882,0.978675249789286,
23.74530687066));
#32330=CARTESIAN_POINT('Ctrl Pts',(-9.66699745489832,0.491325986922189,
23.7684607915091));
#32331=CARTESIAN_POINT('Ctrl Pts',(-9.76148094042856,-0.109317600972408,
23.7916147123582));
#32332=CARTESIAN_POINT('Ctrl Pts',(-9.56508040992899,-0.684753960099927,
23.8147686332073));
#32333=CARTESIAN_POINT('Ctrl Pts',(-9.12308448035522,-1.10229305502416,
23.8379225540564));
#32334=CARTESIAN_POINT('Ctrl Pts',(-8.53741087882009,-1.26565644543905,
23.8610764749055));
#32335=CARTESIAN_POINT('Ctrl Pts',(-7.94311335482628,-1.13717113651722,
23.8842303957546));
#32336=CARTESIAN_POINT('Ctrl Pts',(-7.47722227522078,-0.746471900623929,
23.9073843166037));
#32337=CARTESIAN_POINT('Ctrl Pts',(-7.24718526716919,-0.183635135086069,
23.9305382374527));
#32338=CARTESIAN_POINT('Ctrl Pts',(-7.30600778196775,0.421517743452463,
23.9536921583018));
#32339=CARTESIAN_POINT('Ctrl Pts',(-7.64021434930425,0.929509330617972,
23.9768460791509));
#32340=CARTESIAN_POINT('Ctrl Pts',(-7.99510874416175,1.12516550422187,23.9922820263836));
#32341=CARTESIAN_POINT('Ctrl Pts',(-8.18521110449561,1.17604951161383,24.));
#32342=CARTESIAN_POINT('Ctrl Pts',(-8.18521110449561,1.17604951161383,24.));
#32343=CARTESIAN_POINT('Ctrl Pts',(-8.13719967674948,1.15963874913234,24.));
#32344=CARTESIAN_POINT('Ctrl Pts',(-8.09039244203195,1.14022118863296,24.));
#32345=CARTESIAN_POINT('Ctrl Pts',(-8.0450272420164,1.11798779976491,24.));
#32346=CARTESIAN_POINT('Ctrl Pts',(-7.99968369246786,1.09576502174509,24.));
#32347=CARTESIAN_POINT('Ctrl Pts',(-7.95577990341876,1.07072840198051,24.));
#32348=CARTESIAN_POINT('Ctrl Pts',(-7.91358061464719,1.04302439914058,24.));
#32349=CARTESIAN_POINT('Ctrl Pts',(-7.87480187129976,1.01756599813196,24.));
#32350=CARTESIAN_POINT('Ctrl Pts',(-7.83746227877575,0.989854238462992,
24.));
#32351=CARTESIAN_POINT('Ctrl Pts',(-7.80179731248717,0.959977241321462,
24.));
#32352=CARTESIAN_POINT('Ctrl Pts',(-7.7947015489235,0.954033029682695,24.));
#32353=CARTESIAN_POINT('Ctrl Pts',(-7.78767053166018,0.948001590861504,
24.));
#32354=CARTESIAN_POINT('Ctrl Pts',(-7.78071162172877,0.941888233085706,
24.));
#32355=CARTESIAN_POINT('Ctrl Pts',(-7.75269342371654,0.917274425697755,
24.));
#32356=CARTESIAN_POINT('Ctrl Pts',(-7.72591276091907,0.891395901731505,
24.));
#32357=CARTESIAN_POINT('Ctrl Pts',(-7.70047108636338,0.864317009446147,
24.));
#32358=CARTESIAN_POINT('Ctrl Pts',(-7.66652666178374,0.828188199808707,
24.));
#32359=CARTESIAN_POINT('Ctrl Pts',(-7.63496382945612,0.789923205013932,
24.));
#32360=CARTESIAN_POINT('Ctrl Pts',(-7.60593237124235,0.749788275952098,
24.));
#32361=CARTESIAN_POINT('Ctrl Pts',(-7.58573713320593,0.72186909807236,24.));
#32362=CARTESIAN_POINT('Ctrl Pts',(-7.56676769399393,0.693044320670178,
24.));
#32363=CARTESIAN_POINT('Ctrl Pts',(-7.54908818194333,0.663397823661222,
24.));
#32364=CARTESIAN_POINT('Ctrl Pts',(-7.53965734716309,0.647583404445125,
24.));
#32365=CARTESIAN_POINT('Ctrl Pts',(-7.53059376289677,0.631535105539703,
24.));
#32366=CARTESIAN_POINT('Ctrl Pts',(-7.52190861271761,0.615265404204942,
24.));
#32367=CARTESIAN_POINT('Ctrl Pts',(-7.51748915437742,0.606986529830519,
24.));
#32368=CARTESIAN_POINT('Ctrl Pts',(-7.51316770089473,0.59865032588924,24.));
#32369=CARTESIAN_POINT('Ctrl Pts',(-7.50894583197787,0.590258430824365,
24.));
#32370=CARTESIAN_POINT('Ctrl Pts',(-7.50442354109893,0.581269380890268,
24.));
#32371=CARTESIAN_POINT('Ctrl Pts',(-7.50001888167444,0.572222977380615,
24.));
#32372=CARTESIAN_POINT('Ctrl Pts',(-7.49573658730706,0.563128806983175,
24.));
#32373=CARTESIAN_POINT('Ctrl Pts',(-7.47506533165207,0.519229928221484,
24.));
#32374=CARTESIAN_POINT('Ctrl Pts',(-7.45721483404256,0.474166736055567,
24.));
#32375=CARTESIAN_POINT('Ctrl Pts',(-7.44233259800518,0.428186696862096,
24.));
#32376=CARTESIAN_POINT('Ctrl Pts',(-7.43702164425509,0.411778016004576,
24.));
#32377=CARTESIAN_POINT('Ctrl Pts',(-7.43208916293203,0.395252421852314,
24.));
#32378=CARTESIAN_POINT('Ctrl Pts',(-7.42754343322645,0.378620794841048,
24.));
#32379=CARTESIAN_POINT('Ctrl Pts',(-7.4156225733453,0.335005510158975,24.));
#32380=CARTESIAN_POINT('Ctrl Pts',(-7.40635868431464,0.290660713814978,
24.));
#32381=CARTESIAN_POINT('Ctrl Pts',(-7.39978197468916,0.245833679491224,
24.));
#32382=CARTESIAN_POINT('Ctrl Pts',(-7.39701836248096,0.226996822404678,
24.));
#32383=CARTESIAN_POINT('Ctrl Pts',(-7.39472972284664,0.208074861590042,
24.));
#32384=CARTESIAN_POINT('Ctrl Pts',(-7.39292035690482,0.189086585034831,
24.));
#32385=CARTESIAN_POINT('Ctrl Pts',(-7.392030464189,0.17974766215474,24.));
#32386=CARTESIAN_POINT('Ctrl Pts',(-7.39125638738652,0.170390733140474,
24.));
#32387=CARTESIAN_POINT('Ctrl Pts',(-7.39059917635802,0.161024335815622,
24.));
#32388=CARTESIAN_POINT('Ctrl Pts',(-7.3872631549861,0.113480243737833,24.));
#32389=CARTESIAN_POINT('Ctrl Pts',(-7.38694590585192,0.0658798878746482,
24.));
#32390=CARTESIAN_POINT('Ctrl Pts',(-7.38964476207475,0.0185121699340391,
24.));
#32391=CARTESIAN_POINT('Ctrl Pts',(-7.39231303882574,-0.0283188466494503,
24.));
#32392=CARTESIAN_POINT('Ctrl Pts',(-7.39792964052343,-0.0749235404025428,
24.));
#32393=CARTESIAN_POINT('Ctrl Pts',(-7.4065414629921,-0.121013652593743,
24.));
#32394=CARTESIAN_POINT('Ctrl Pts',(-7.40892335149359,-0.133761419824211,
24.));
#32395=CARTESIAN_POINT('Ctrl Pts',(-7.41153465540497,-0.146469716439907,
24.));
#32396=CARTESIAN_POINT('Ctrl Pts',(-7.41437701908526,-0.159132152321132,
24.));
#32397=CARTESIAN_POINT('Ctrl Pts',(-7.41931573092333,-0.18113360217748,
24.));
#32398=CARTESIAN_POINT('Ctrl Pts',(-7.42495191576504,-0.202996694808475,
24.));
#32399=CARTESIAN_POINT('Ctrl Pts',(-7.43127562948781,-0.224689624790342,
24.));
#32400=CARTESIAN_POINT('Ctrl Pts',(-7.43448561573921,-0.235701193315895,
24.));
#32401=CARTESIAN_POINT('Ctrl Pts',(-7.43787279027184,-0.246668889780893,
24.));
#32402=CARTESIAN_POINT('Ctrl Pts',(-7.44143604991943,-0.25758837346045,
24.));
#32403=CARTESIAN_POINT('Ctrl Pts',(-7.44466461678404,-0.267482202895614,
24.));
#32404=CARTESIAN_POINT('Ctrl Pts',(-7.44803514244817,-0.277328343641491,
24.));
#32405=CARTESIAN_POINT('Ctrl Pts',(-7.45154465378086,-0.287119754649393,
24.));
#32406=CARTESIAN_POINT('Ctrl Pts',(-7.46731935144868,-0.331130596544133,
24.));
#32407=CARTESIAN_POINT('Ctrl Pts',(-7.48590745098904,-0.37406509962981,
24.));
#32408=CARTESIAN_POINT('Ctrl Pts',(-7.50719025592286,-0.415648653082733,
24.));
#32409=CARTESIAN_POINT('Ctrl Pts',(-7.51904262814917,-0.438806491325817,
24.));
#32410=CARTESIAN_POINT('Ctrl Pts',(-7.53173151770624,-0.461544875560217,
24.));
#32411=CARTESIAN_POINT('Ctrl Pts',(-7.545241722074,-0.483811700343089,24.));
#32412=CARTESIAN_POINT('Ctrl Pts',(-7.55097545041931,-0.493261736844557,
24.));
#32413=CARTESIAN_POINT('Ctrl Pts',(-7.55685657402864,-0.502625594711996,
24.));
#32414=CARTESIAN_POINT('Ctrl Pts',(-7.56287708030514,-0.511889163975369,
24.));
#32415=CARTESIAN_POINT('Ctrl Pts',(-7.5881701579766,-0.550806850650343,
24.));
#32416=CARTESIAN_POINT('Ctrl Pts',(-7.61595032929573,-0.588007881425946,
24.));
#32417=CARTESIAN_POINT('Ctrl Pts',(-7.64611624065442,-0.623205040740634,
24.));
#32418=CARTESIAN_POINT('Ctrl Pts',(-7.66532287318705,-0.645615068308218,
24.));
#32419=CARTESIAN_POINT('Ctrl Pts',(-7.68549754918253,-0.667211980957074,
24.));
#32420=CARTESIAN_POINT('Ctrl Pts',(-7.7065805280024,-0.687941579884204,
24.));
#32421=CARTESIAN_POINT('Ctrl Pts',(-7.70661869325984,-0.687936125025627,
22.8));
#32422=CARTESIAN_POINT('Ctrl Pts',(-7.67409887424617,-0.655902278122709,
22.8));
#32423=CARTESIAN_POINT('Ctrl Pts',(-7.64381509977965,-0.621808637047501,
22.8));
#32424=CARTESIAN_POINT('Ctrl Pts',(-7.61585772416164,-0.585954657403442,
22.8));
#32425=CARTESIAN_POINT('Ctrl Pts',(-7.58750148055764,-0.549589148893234,
22.8));
#32426=CARTESIAN_POINT('Ctrl Pts',(-7.5615377630002,-0.511411926505863,
22.8));
#32427=CARTESIAN_POINT('Ctrl Pts',(-7.53809119922464,-0.471690207387441,
22.8));
#32428=CARTESIAN_POINT('Ctrl Pts',(-7.51732937629883,-0.436516810273061,
22.8));
#32429=CARTESIAN_POINT('Ctrl Pts',(-7.49854136850491,-0.400131309259636,
22.8));
#32430=CARTESIAN_POINT('Ctrl Pts',(-7.48184017620086,-0.362698053565758,
22.8));
#32431=CARTESIAN_POINT('Ctrl Pts',(-7.47711294155032,-0.352102655334479,
22.8));
#32432=CARTESIAN_POINT('Ctrl Pts',(-7.4725517371607,-0.341419507353799,
22.8));
#32433=CARTESIAN_POINT('Ctrl Pts',(-7.46816951388458,-0.330677896224689,
22.8));
#32434=CARTESIAN_POINT('Ctrl Pts',(-7.45706946072126,-0.303469685442133,
22.8));
#32435=CARTESIAN_POINT('Ctrl Pts',(-7.44710318825052,-0.275857043294133,
22.8));
#32436=CARTESIAN_POINT('Ctrl Pts',(-7.43829808473137,-0.247908606918607,
22.8));
#32437=CARTESIAN_POINT('Ctrl Pts',(-7.42417847687612,-0.203091307390929,
22.8));
#32438=CARTESIAN_POINT('Ctrl Pts',(-7.41304200334992,-0.157411667924642,
22.8));
#32439=CARTESIAN_POINT('Ctrl Pts',(-7.40485337567042,-0.111173146702142,
22.8));
#32440=CARTESIAN_POINT('Ctrl Pts',(-7.3990667072828,-0.0784977095566693,
22.8));
#32441=CARTESIAN_POINT('Ctrl Pts',(-7.39475310628434,-0.0455424363337794,
22.8));
#32442=CARTESIAN_POINT('Ctrl Pts',(-7.39191475620744,-0.0124086226667018,
22.8));
#32443=CARTESIAN_POINT('Ctrl Pts',(-7.39015601726076,0.00812222341272933,
22.8));
#32444=CARTESIAN_POINT('Ctrl Pts',(-7.38896393745883,0.028721696174667,
22.8));
#32445=CARTESIAN_POINT('Ctrl Pts',(-7.38834146456221,0.0493660552932196,
22.8));
#32446=CARTESIAN_POINT('Ctrl Pts',(-7.38797934168981,0.0613758868268767,
22.8));
#32447=CARTESIAN_POINT('Ctrl Pts',(-7.38781020265733,0.0734053336283251,
22.8));
#32448=CARTESIAN_POINT('Ctrl Pts',(-7.38783436635261,0.0854208914751402,
22.8));
#32449=CARTESIAN_POINT('Ctrl Pts',(-7.38793158368919,0.133762857296808,
22.8));
#32450=CARTESIAN_POINT('Ctrl Pts',(-7.39114907770623,0.181961184367851,
22.8));
#32451=CARTESIAN_POINT('Ctrl Pts',(-7.39745467436063,0.229704925733033,
22.8));
#32452=CARTESIAN_POINT('Ctrl Pts',(-7.3999312816523,0.248456917729558,22.8));
#32453=CARTESIAN_POINT('Ctrl Pts',(-7.40288481096348,0.267138971151595,
22.8));
#32454=CARTESIAN_POINT('Ctrl Pts',(-7.40631544490045,0.285732738634787,
22.8));
#32455=CARTESIAN_POINT('Ctrl Pts',(-7.41475540033853,0.33147663666289,22.8));
#32456=CARTESIAN_POINT('Ctrl Pts',(-7.42607978052882,0.37668661873272,22.8));
#32457=CARTESIAN_POINT('Ctrl Pts',(-7.44015842069487,0.421132678936863,
22.8));
#32458=CARTESIAN_POINT('Ctrl Pts',(-7.44619862362351,0.440201510858501,
22.8));
#32459=CARTESIAN_POINT('Ctrl Pts',(-7.45274637533637,0.459129659953141,
22.8));
#32460=CARTESIAN_POINT('Ctrl Pts',(-7.45979389453231,0.477898384958879,
22.8));
#32461=CARTESIAN_POINT('Ctrl Pts',(-7.46424271571329,0.489746341526856,
22.8));
#32462=CARTESIAN_POINT('Ctrl Pts',(-7.4688928540224,0.501535475997375,22.8));
#32463=CARTESIAN_POINT('Ctrl Pts',(-7.47373027012052,0.513232377204913,
22.8));
#32464=CARTESIAN_POINT('Ctrl Pts',(-7.49246848990274,0.558541505291551,
22.8));
#32465=CARTESIAN_POINT('Ctrl Pts',(-7.51403747741391,0.602540157612762,
22.8));
#32466=CARTESIAN_POINT('Ctrl Pts',(-7.53825727973114,0.64497438097173,22.8));
#32467=CARTESIAN_POINT('Ctrl Pts',(-7.56269818112947,0.687795980233644,
22.8));
#32468=CARTESIAN_POINT('Ctrl Pts',(-7.58983884034064,0.729025540060729,
22.8));
#32469=CARTESIAN_POINT('Ctrl Pts',(-7.61954520807962,0.768390367753865,
22.8));
#32470=CARTESIAN_POINT('Ctrl Pts',(-7.624943127649,0.775543318111749,22.8));
#32471=CARTESIAN_POINT('Ctrl Pts',(-7.63042588898144,0.78263464183452,22.8));
#32472=CARTESIAN_POINT('Ctrl Pts',(-7.6359928529246,0.789662617571405,22.8));
#32473=CARTESIAN_POINT('Ctrl Pts',(-7.65117021204093,0.808823171278727,
22.8));
#32474=CARTESIAN_POINT('Ctrl Pts',(-7.66697325962642,0.827513014577617,
22.8));
#32475=CARTESIAN_POINT('Ctrl Pts',(-7.68337375414277,0.845711485231679,
22.8));
#32476=CARTESIAN_POINT('Ctrl Pts',(-7.69112592074004,0.854313517090244,
22.8));
#32477=CARTESIAN_POINT('Ctrl Pts',(-7.69901160789439,0.862805734908379,
22.8));
#32478=CARTESIAN_POINT('Ctrl Pts',(-7.70702801425658,0.871185789564867,
22.8));
#32479=CARTESIAN_POINT('Ctrl Pts',(-7.71445567795972,0.878950394425205,
22.8));
#32480=CARTESIAN_POINT('Ctrl Pts',(-7.72198985783713,0.886612666880794,
22.8));
#32481=CARTESIAN_POINT('Ctrl Pts',(-7.72962396642253,0.894167421350373,
22.8));
#32482=CARTESIAN_POINT('Ctrl Pts',(-7.76528195653565,0.929454758066893,
22.8));
#32483=CARTESIAN_POINT('Ctrl Pts',(-7.80314189130454,0.962425220262479,
22.8));
#32484=CARTESIAN_POINT('Ctrl Pts',(-7.84293242203276,0.992923281459069,
22.8));
#32485=CARTESIAN_POINT('Ctrl Pts',(-7.86518021716756,1.00997544450119,22.8));
#32486=CARTESIAN_POINT('Ctrl Pts',(-7.88803237641158,1.02625419485435,22.8));
#32487=CARTESIAN_POINT('Ctrl Pts',(-7.91144681261877,1.041727736773,22.8));
#32488=CARTESIAN_POINT('Ctrl Pts',(-7.92363416860997,1.04978180914692,22.8));
#32489=CARTESIAN_POINT('Ctrl Pts',(-7.9359761488319,1.05761880028698,22.8));
#32490=CARTESIAN_POINT('Ctrl Pts',(-7.94844671421418,1.06522202719557,22.8));
#32491=CARTESIAN_POINT('Ctrl Pts',(-7.99400669055524,1.09299966417129,22.8));
#32492=CARTESIAN_POINT('Ctrl Pts',(-8.04133377544581,1.11769811978497,22.8));
#32493=CARTESIAN_POINT('Ctrl Pts',(-8.09012868784477,1.13911684874061,22.8));
#32494=CARTESIAN_POINT('Ctrl Pts',(-8.12124386749461,1.15277498575861,22.8));
#32495=CARTESIAN_POINT('Ctrl Pts',(-8.15295686822968,1.16509867088334,22.8));
#32496=CARTESIAN_POINT('Ctrl Pts',(-8.18517800353954,1.17607954763522,22.8));
#32497=CARTESIAN_POINT('Ctrl Pts',(-9.55016549375182,-1.36966017015294E-5,
23.2841069671524));
#32498=CARTESIAN_POINT('Ctrl Pts',(-9.55006280769147,0.154119316631831,
23.2770974504288));
#32499=CARTESIAN_POINT('Ctrl Pts',(-9.5156733518718,0.308296679411134,23.2700879337053));
#32500=CARTESIAN_POINT('Ctrl Pts',(-9.44996653184482,0.447714329856668,
23.2630784169817));
#32501=CARTESIAN_POINT('Ctrl Pts',(-9.3776186762958,0.601223022428839,23.2553604433654));
#32502=CARTESIAN_POINT('Ctrl Pts',(-9.26730300356168,0.736837678456824,
23.247642469749));
#32503=CARTESIAN_POINT('Ctrl Pts',(-9.1317383100797,0.838922666491548,23.2399244961327));
#32504=CARTESIAN_POINT('Ctrl Pts',(-8.99617361659773,0.941007654526272,
23.2322065225163));
#32505=CARTESIAN_POINT('Ctrl Pts',(-8.8353599023679,1.00956297456774,23.2244885488999));
#32506=CARTESIAN_POINT('Ctrl Pts',(-8.66783811309464,1.03668457141066,23.2167705752836));
#32507=CARTESIAN_POINT('Ctrl Pts',(-8.50031632382139,1.06380616825358,23.2090526016672));
#32508=CARTESIAN_POINT('Ctrl Pts',(-8.3260864595047,1.04949404189796,23.2013346280508));
#32509=CARTESIAN_POINT('Ctrl Pts',(-8.16523627485858,0.995398302717987,
23.1936166544345));
#32510=CARTESIAN_POINT('Ctrl Pts',(-8.00438609021247,0.941302563538019,
23.1858986808181));
#32511=CARTESIAN_POINT('Ctrl Pts',(-7.85691558523692,0.8474232115337,23.1781807072018));
#32512=CARTESIAN_POINT('Ctrl Pts',(-7.73982730631698,0.724584024576948,
23.1704627335854));
#32513=CARTESIAN_POINT('Ctrl Pts',(-7.62273902739704,0.601744837620195,
23.162744759969));
#32514=CARTESIAN_POINT('Ctrl Pts',(-7.5360329745327,0.449945815711004,23.1550267863527));
#32515=CARTESIAN_POINT('Ctrl Pts',(-7.48970588337769,0.286688560209014,
23.1473088127363));
#32516=CARTESIAN_POINT('Ctrl Pts',(-7.44337879222268,0.123431304707024,
23.13959083912));
#32517=CARTESIAN_POINT('Ctrl Pts',(-7.43743066277701,-0.051284184387765,
23.1318728655036));
#32518=CARTESIAN_POINT('Ctrl Pts',(-7.47254728234041,-0.21731416377441,
23.1241548918872));
#32519=CARTESIAN_POINT('Ctrl Pts',(-7.50766390190381,-0.383344143161055,
23.1164369182709));
#32520=CARTESIAN_POINT('Ctrl Pts',(-7.58384527047628,-0.540688612839554,
23.1087189446545));
#32521=CARTESIAN_POINT('Ctrl Pts',(-7.69230809025561,-0.671206609198054,
23.1010009710381));
#32522=CARTESIAN_POINT('Ctrl Pts',(-7.80077091003495,-0.801724605556554,
23.0932829974218));
#32523=CARTESIAN_POINT('Ctrl Pts',(-7.94151518102115,-0.905416128595054,
23.0855650238054));
#32524=CARTESIAN_POINT('Ctrl Pts',(-8.09831385678209,-0.970326116650706,
23.077847050189));
#32525=CARTESIAN_POINT('Ctrl Pts',(-8.25511253254303,-1.03523610470636,
23.0701290765727));
#32526=CARTESIAN_POINT('Ctrl Pts',(-8.42796561307872,-1.06136455777916,
23.0624111029563));
#32527=CARTESIAN_POINT('Ctrl Pts',(-8.59694407560669,-1.04569899349385,
23.05469312934));
#32528=CARTESIAN_POINT('Ctrl Pts',(-8.76592253813466,-1.03003342920854,
23.0469751557236));
#32529=CARTESIAN_POINT('Ctrl Pts',(-8.93102638265491,-0.97257384756512,
23.0392571821072));
#32530=CARTESIAN_POINT('Ctrl Pts',(-9.07322004306799,-0.879945055895734,
23.0315392084909));
#32531=CARTESIAN_POINT('Ctrl Pts',(-9.21541370348107,-0.787316264226347,
23.0238212348745));
#32532=CARTESIAN_POINT('Ctrl Pts',(-9.33469717978697,-0.659518262530998,
23.0161032612582));
#32533=CARTESIAN_POINT('Ctrl Pts',(-9.41731771909817,-0.511285397707312,
23.0083852876418));
#32534=CARTESIAN_POINT('Ctrl Pts',(-9.49993825840937,-0.363052532883626,
23.0006673140254));
#32535=CARTESIAN_POINT('Ctrl Pts',(-9.54589586072586,-0.194384804931602,
22.9929493404091));
#32536=CARTESIAN_POINT('Ctrl Pts',(-9.54989190461633,-0.0247288290775425,
22.9852313667927));
#32537=CARTESIAN_POINT('Ctrl Pts',(-9.55008596031612,-0.0164900033739872,
22.9848565669126));
#32538=CARTESIAN_POINT('Ctrl Pts',(-9.55018105960925,-0.00824884712159311,
22.9844817670325));
#32539=CARTESIAN_POINT('Ctrl Pts',(-9.5501777037735,-7.61342713928581E-6,
22.9841069671524));
#32540=CARTESIAN_POINT('Ctrl Pts',(-8.81478889550448,1.17604951161381,22.8));
#32541=CARTESIAN_POINT('Ctrl Pts',(-9.00489125583834,1.12516550422183,22.8077179736164));
#32542=CARTESIAN_POINT('Ctrl Pts',(-9.35978561312172,0.929509121580238,
22.8231539208491));
#32543=CARTESIAN_POINT('Ctrl Pts',(-9.69399222430856,0.421517693774337,
22.8463078416982));
#32544=CARTESIAN_POINT('Ctrl Pts',(-9.75281474611789,-0.183635193835607,
22.8694617625473));
#32545=CARTESIAN_POINT('Ctrl Pts',(-9.5227777403229,-0.746471923361528,
22.8926156833964));
#32546=CARTESIAN_POINT('Ctrl Pts',(-9.05688665443706,-1.13717116763217,
22.9157696042454));
#32547=CARTESIAN_POINT('Ctrl Pts',(-8.46258911977101,-1.2656564697317,22.9389235250945));
#32548=CARTESIAN_POINT('Ctrl Pts',(-7.87691550790518,-1.10229307735719,
22.9620774459436));
#32549=CARTESIAN_POINT('Ctrl Pts',(-7.43491956993902,-0.684753972836506,
22.9852313667927));
#32550=CARTESIAN_POINT('Ctrl Pts',(-7.23851903592649,-0.109317603314454,
23.0083852876418));
#32551=CARTESIAN_POINT('Ctrl Pts',(-7.33300252317075,0.49132599619855,23.0315392084909));
#32552=CARTESIAN_POINT('Ctrl Pts',(-7.69658280697753,0.978675268097788,
23.05469312934));
#32553=CARTESIAN_POINT('Ctrl Pts',(-8.24542239893397,1.24035263469515,23.077847050189));
#32554=CARTESIAN_POINT('Ctrl Pts',(-8.85296478970154,1.21601821059452,23.1010009710381));
#32555=CARTESIAN_POINT('Ctrl Pts',(-9.37911735435305,0.911283219057196,
23.1241548918872));
#32556=CARTESIAN_POINT('Ctrl Pts',(-9.70255502492968,0.396416244609647,
23.1473088127363));
#32557=CARTESIAN_POINT('Ctrl Pts',(-9.74869660384231,-0.209860001191851,
23.1704627335854));
#32558=CARTESIAN_POINT('Ctrl Pts',(-9.50690234210182,-0.767744815010462,
23.1936166544345));
#32559=CARTESIAN_POINT('Ctrl Pts',(-9.03292736505941,-1.14859603498855,
23.2167705752836));
#32560=CARTESIAN_POINT('Ctrl Pts',(-8.436065140539,-1.2645935163393,23.2399244961327));
#32561=CARTESIAN_POINT('Ctrl Pts',(-7.85394559851473,-1.08898950325348,
23.2630784169817));
#32562=CARTESIAN_POINT('Ctrl Pts',(-7.42079916644579,-0.662276368844085,
23.2862323378308));
#32563=CARTESIAN_POINT('Ctrl Pts',(-7.23650469503931,-0.0828495154220059,
23.3093862586799));
#32564=CARTESIAN_POINT('Ctrl Pts',(-7.34355848256139,0.515681534104197,
23.332540179529));
#32565=CARTESIAN_POINT('Ctrl Pts',(-7.71727509134788,0.995302037194035,
23.3556941003781));
#32566=CARTESIAN_POINT('Ctrl Pts',(-8.27147954086117,1.24541672849857,23.3788480212272));
#32567=CARTESIAN_POINT('Ctrl Pts',(-8.87837831986,1.20835188373602,23.4020019420763));
#32568=CARTESIAN_POINT('Ctrl Pts',(-9.39802717851571,0.892654252505216,
23.4251558629254));
#32569=CARTESIAN_POINT('Ctrl Pts',(-9.7106007485556,0.371120270889709,23.4483097837744));
#32570=CARTESIAN_POINT('Ctrl Pts',(-9.74402296838762,-0.235990004009924,
23.4714637046235));
#32571=CARTESIAN_POINT('Ctrl Pts',(-9.49058703805816,-0.788683553714432,
23.4946176254726));
#32572=CARTESIAN_POINT('Ctrl Pts',(-9.0087325233999,-1.15951526402384,23.5177715463217));
#32573=CARTESIAN_POINT('Ctrl Pts',(-8.40956982850905,-1.26297538057999,
23.5409254671708));
#32574=CARTESIAN_POINT('Ctrl Pts',(-7.8312593464559,-1.07520712710119,23.5640793880199));
#32575=CARTESIAN_POINT('Ctrl Pts',(-7.40715317709645,-0.639507818195355,
23.587233308869));
#32576=CARTESIAN_POINT('Ctrl Pts',(-7.23504558492588,-0.0563449701204428,
23.6103872297181));
#32577=CARTESIAN_POINT('Ctrl Pts',(-7.35462270660441,0.539810414542498,
23.6335411505671));
#32578=CARTESIAN_POINT('Ctrl Pts',(-7.73831135994277,1.011491395628,23.6566950714162));
#32579=CARTESIAN_POINT('Ctrl Pts',(-8.2976371195735,1.24993347528822,23.6798489922653));
#32580=CARTESIAN_POINT('Ctrl Pts',(-8.90362555579596,1.20015450597578,23.7030029131144));
#32581=CARTESIAN_POINT('Ctrl Pts',(-9.41654233415426,0.873632976856196,
23.7261568339635));
#32582=CARTESIAN_POINT('Ctrl Pts',(-9.71811443025979,0.345661195055098,
23.7493107548126));
#32583=CARTESIAN_POINT('Ctrl Pts',(-9.73880260375737,-0.262016291447522,
23.7724646756616));
#32584=CARTESIAN_POINT('Ctrl Pts',(-9.47383638460599,-0.809275680645407,
23.7956185965108));
#32585=CARTESIAN_POINT('Ctrl Pts',(-8.98431410313225,-1.16992489625058,
23.8187725173598));
#32586=CARTESIAN_POINT('Ctrl Pts',(-8.38311425495986,-1.2608022005996,23.8419264382089));
#32587=CARTESIAN_POINT('Ctrl Pts',(-7.80886700439182,-1.06095217981207,
23.865080359058));
#32588=CARTESIAN_POINT('Ctrl Pts',(-7.39398745671621,-0.616458283433,23.8882342799071));
#32589=CARTESIAN_POINT('Ctrl Pts',(-7.23414244016268,-0.0298154996095495,
23.9113882007562));
#32590=CARTESIAN_POINT('Ctrl Pts',(-7.36619019624783,0.563701731054729,
23.9345421216053));
#32591=CARTESIAN_POINT('Ctrl Pts',(-7.75968252106489,1.02723702411681,23.9576960424544));
#32592=CARTESIAN_POINT('Ctrl Pts',(-8.32388300007083,1.25389944282625,23.9808499633035));
#32593=CARTESIAN_POINT('Ctrl Pts',(-8.92869574141285,1.19143384195749,24.0040038841525));
#32594=CARTESIAN_POINT('Ctrl Pts',(-9.43465056894933,0.854221860214417,
24.0271578050016));
#32595=CARTESIAN_POINT('Ctrl Pts',(-9.72509085321044,0.320073427910269,
24.0503117258507));
#32596=CARTESIAN_POINT('Ctrl Pts',(-9.73300691540701,-0.287945227761225,
24.0734656466998));
#32597=CARTESIAN_POINT('Ctrl Pts',(-9.54874216054247,-0.648885562186029,
24.0889015939325));
#32598=CARTESIAN_POINT('Ctrl Pts',(-9.41981913331181,-0.797569598526366,
24.0966195675489));
#32599=CARTESIAN_POINT('Ctrl Pts',(-8.80036532666177,1.12216314098433,22.7677934774837));
#32600=CARTESIAN_POINT('Ctrl Pts',(-8.98175723208253,1.07361062937918,22.7755114511001));
#32601=CARTESIAN_POINT('Ctrl Pts',(-9.32039039569844,0.886919185923345,
22.7909473983328));
#32602=CARTESIAN_POINT('Ctrl Pts',(-9.63928372190927,0.402203831178163,
22.8141013191819));
#32603=CARTESIAN_POINT('Ctrl Pts',(-9.69541100667265,-0.175221063292699,
22.837255240031));
#32604=CARTESIAN_POINT('Ctrl Pts',(-9.47591425384351,-0.712268718199221,
22.8604091608801));
#32605=CARTESIAN_POINT('Ctrl Pts',(-9.03137021115533,-1.08506619551744,
22.8835630817292));
#32606=CARTESIAN_POINT('Ctrl Pts',(-8.46430327936862,-1.20766432489081,
22.9067170025782));
#32607=CARTESIAN_POINT('Ctrl Pts',(-7.90546512383795,-1.05178621287385,
22.9298709234273));
#32608=CARTESIAN_POINT('Ctrl Pts',(-7.48372135782099,-0.65337867272721,
22.9530248442764));
#32609=CARTESIAN_POINT('Ctrl Pts',(-7.29631985987209,-0.104308690993709,
22.9761787651255));
#32610=CARTESIAN_POINT('Ctrl Pts',(-7.38647413124429,0.468813530124974,
22.9993326859746));
#32611=CARTESIAN_POINT('Ctrl Pts',(-7.73339523384031,0.933832548720903,
23.0224866068237));
#32612=CARTESIAN_POINT('Ctrl Pts',(-8.25708709742628,1.18351990688532,23.0456405276727));
#32613=CARTESIAN_POINT('Ctrl Pts',(-8.83679200846301,1.16030048158635,23.0687944485218));
#32614=CARTESIAN_POINT('Ctrl Pts',(-9.33883636012989,0.869528390875553,
23.0919483693709));
#32615=CARTESIAN_POINT('Ctrl Pts',(-9.64745417659313,0.378252525761392,
23.11510229022));
#32616=CARTESIAN_POINT('Ctrl Pts',(-9.6914815569128,-0.200244254836913,
23.1382562110691));
#32617=CARTESIAN_POINT('Ctrl Pts',(-9.46076626342624,-0.732566889895946,
23.1614101319182));
#32618=CARTESIAN_POINT('Ctrl Pts',(-9.00850873197586,-1.09596757756927,
23.1845640527673));
#32619=CARTESIAN_POINT('Ctrl Pts',(-8.43899462394853,-1.20665007582583,
23.2077179736164));
#32620=CARTESIAN_POINT('Ctrl Pts',(-7.88354769143807,-1.03909220606962,
23.2308718944654));
#32621=CARTESIAN_POINT('Ctrl Pts',(-7.47024794859846,-0.63193098838327,
23.2540258153145));
#32622=CARTESIAN_POINT('Ctrl Pts',(-7.29439781571098,-0.079053365982365,
23.2771797361636));
#32623=CARTESIAN_POINT('Ctrl Pts',(-7.3965464185323,0.492053101798328,23.3003336570127));
#32624=CARTESIAN_POINT('Ctrl Pts',(-7.75313940157635,0.9496974823391,23.3234875778618));
#32625=CARTESIAN_POINT('Ctrl Pts',(-8.28195030594033,1.18835196484935,23.3466414987109));
#32626=CARTESIAN_POINT('Ctrl Pts',(-8.86104109538026,1.15298542440347,23.36979541956));
#32627=CARTESIAN_POINT('Ctrl Pts',(-9.35687973965453,0.851753000117917,
23.3929493404091));
#32628=CARTESIAN_POINT('Ctrl Pts',(-9.65513124665388,0.354115608868437,
23.4161032612581));
#32629=CARTESIAN_POINT('Ctrl Pts',(-9.68702206656833,-0.225176985769323,
23.4392571821073));
#32630=CARTESIAN_POINT('Ctrl Pts',(-9.44519852358965,-0.752546219473707,
23.4624111029563));
#32631=CARTESIAN_POINT('Ctrl Pts',(-8.98542249347644,-1.10638648955414,
23.4855650238054));
#32632=CARTESIAN_POINT('Ctrl Pts',(-8.41371332220462,-1.20510608274707,
23.5087189446545));
#32633=CARTESIAN_POINT('Ctrl Pts',(-7.86190091924345,-1.02594133583792,
23.5318728655036));
#32634=CARTESIAN_POINT('Ctrl Pts',(-7.45722721595169,-0.610205688504884,
23.5550267863527));
#32635=CARTESIAN_POINT('Ctrl Pts',(-7.29300556175248,-0.0537632540336343,
23.5781807072018));
#32636=CARTESIAN_POINT('Ctrl Pts',(-7.40710368188054,0.51507640140748,23.6013346280508));
#32637=CARTESIAN_POINT('Ctrl Pts',(-7.7732117922435,0.965145047370478,23.6244885488999));
#32638=CARTESIAN_POINT('Ctrl Pts',(-8.30690934924464,1.19266175513832,23.647642469749));
#32639=CARTESIAN_POINT('Ctrl Pts',(-8.88513150764547,1.14516364897274,23.6707963905981));
#32640=CARTESIAN_POINT('Ctrl Pts',(-9.3745465342937,0.83360327579335,23.6939503114472));
#32641=CARTESIAN_POINT('Ctrl Pts',(-9.66230065285511,0.329823063169471,
23.7171042322963));
#32642=CARTESIAN_POINT('Ctrl Pts',(-9.68204089807779,-0.250010753540766,
23.7402581531454));
#32643=CARTESIAN_POINT('Ctrl Pts',(-9.42921538197376,-0.772194818965664,
23.7634120739945));
#32644=CARTESIAN_POINT('Ctrl Pts',(-8.96212292069925,-1.11631915436179,
23.7865659948435));
#32645=CARTESIAN_POINT('Ctrl Pts',(-8.38846993813164,-1.20303247747056,
23.8097199156926));
#32646=CARTESIAN_POINT('Ctrl Pts',(-7.8405345901421,-1.0123395475913,23.8328738365417));
#32647=CARTESIAN_POINT('Ctrl Pts',(-7.44466474643886,-0.588212279152875,
23.8560277573908));
#32648=CARTESIAN_POINT('Ctrl Pts',(-7.29214379891493,-0.0284493589440447,
23.8791816782399));
#32649=CARTESIAN_POINT('Ctrl Pts',(-7.41814115129264,0.537873022225616,
23.902335599089));
#32650=CARTESIAN_POINT('Ctrl Pts',(-7.79360373072436,0.98016921408055,23.9254895199381));
#32651=CARTESIAN_POINT('Ctrl Pts',(-8.33195264836252,1.19644600277889,23.9486434407872));
#32652=CARTESIAN_POINT('Ctrl Pts',(-8.90905298200441,1.1368425641633,23.9717973616362));
#32653=CARTESIAN_POINT('Ctrl Pts',(-9.391825053127,0.815081572918051,23.9949512824853));
#32654=CARTESIAN_POINT('Ctrl Pts',(-9.66895741739932,0.305407722772266,
24.0181052033344));
#32655=CARTESIAN_POINT('Ctrl Pts',(-9.67651076709336,-0.274751630798765,
24.0412591241835));
#32656=CARTESIAN_POINT('Ctrl Pts',(-9.50068898914138,-0.619153746004165,
24.0566950714162));
#32657=CARTESIAN_POINT('Ctrl Pts',(-9.37767319112124,-0.761025107359477,
24.0644130450326));
#32658=CARTESIAN_POINT('Ctrl Pts',(-8.78594175781906,1.06827677035485,22.7355869549674));
#32659=CARTESIAN_POINT('Ctrl Pts',(-8.95862320832672,1.02205575453654,22.7433049285838));
#32660=CARTESIAN_POINT('Ctrl Pts',(-9.28099517827516,0.844329250266453,
22.7587408758165));
#32661=CARTESIAN_POINT('Ctrl Pts',(-9.58457521950998,0.38288996858199,22.7818947966656));
#32662=CARTESIAN_POINT('Ctrl Pts',(-9.63800726722741,-0.166806932749792,
22.8050487175147));
#32663=CARTESIAN_POINT('Ctrl Pts',(-9.42905076736411,-0.678065513036913,
22.8282026383638));
#32664=CARTESIAN_POINT('Ctrl Pts',(-9.0058537678736,-1.03296122340271,22.8513565592129));
#32665=CARTESIAN_POINT('Ctrl Pts',(-8.46601743896623,-1.14967218004993,
22.8745104800619));
#32666=CARTESIAN_POINT('Ctrl Pts',(-7.93401473977073,-1.00127934839051,
22.897664400911));
#32667=CARTESIAN_POINT('Ctrl Pts',(-7.53252314570295,-0.622003372617913,
22.9208183217601));
#32668=CARTESIAN_POINT('Ctrl Pts',(-7.35412068381769,-0.0992997786729641,
22.9439722426092));
#32669=CARTESIAN_POINT('Ctrl Pts',(-7.43994573931782,0.446301064051396,
22.9671261634583));
#32670=CARTESIAN_POINT('Ctrl Pts',(-7.77020766070311,0.888989829344018,
22.9902800843074));
#32671=CARTESIAN_POINT('Ctrl Pts',(-8.26875179591859,1.12668717907549,23.0134340051565));
#32672=CARTESIAN_POINT('Ctrl Pts',(-8.82061922722448,1.10458275257818,23.0365879260056));
#32673=CARTESIAN_POINT('Ctrl Pts',(-9.29855536590672,0.827773562693911,
23.0597418468546));
#32674=CARTESIAN_POINT('Ctrl Pts',(-9.59235332825659,0.360088806913137,
23.0828957677037));
#32675=CARTESIAN_POINT('Ctrl Pts',(-9.63426650998328,-0.190628508481975,
23.1060496885528));
#32676=CARTESIAN_POINT('Ctrl Pts',(-9.41463018475067,-0.697388964781431,
23.1292036094019));
#32677=CARTESIAN_POINT('Ctrl Pts',(-8.98409009889231,-1.04333912014998,
23.152357530251));
#32678=CARTESIAN_POINT('Ctrl Pts',(-8.44192410735806,-1.14870663531236,
23.1755114511001));
#32679=CARTESIAN_POINT('Ctrl Pts',(-7.91314978436141,-0.98919490888576,
23.1986653719492));
#32680=CARTESIAN_POINT('Ctrl Pts',(-7.51969673075113,-0.601585607922455,
23.2218192927983));
#32681=CARTESIAN_POINT('Ctrl Pts',(-7.35229093638265,-0.075257216542724,
23.2449732136473));
#32682=CARTESIAN_POINT('Ctrl Pts',(-7.44953435450321,0.468424669492461,
23.2681271344964));
#32683=CARTESIAN_POINT('Ctrl Pts',(-7.78900371180481,0.904092927484164,
23.2912810553455));
#32684=CARTESIAN_POINT('Ctrl Pts',(-8.29242107101949,1.13128720120013,23.3144349761946));
#32685=CARTESIAN_POINT('Ctrl Pts',(-8.84370387090052,1.09761896507093,23.3375888970437));
#32686=CARTESIAN_POINT('Ctrl Pts',(-9.31573230079336,0.81085174773062,23.3607428178928));
#32687=CARTESIAN_POINT('Ctrl Pts',(-9.59966174475214,0.337110946847165,
23.3838967387418));
#32688=CARTESIAN_POINT('Ctrl Pts',(-9.63002116474905,-0.214363967528721,
23.407050659591));
#32689=CARTESIAN_POINT('Ctrl Pts',(-9.39981000912115,-0.716408885232983,
23.43020458044));
#32690=CARTESIAN_POINT('Ctrl Pts',(-8.96211246355297,-1.05325771508445,
23.4533585012891));
#32691=CARTESIAN_POINT('Ctrl Pts',(-8.41785681590019,-1.14723678491415,
23.4765124221382));
#32692=CARTESIAN_POINT('Ctrl Pts',(-7.892542492031,-0.976675544574657,23.4996663429873));
#32693=CARTESIAN_POINT('Ctrl Pts',(-7.50730125480692,-0.580903558814412,
23.5228202638364));
#32694=CARTESIAN_POINT('Ctrl Pts',(-7.35096553857909,-0.0511815379468251,
23.5459741846855));
#32695=CARTESIAN_POINT('Ctrl Pts',(-7.45958465715666,0.49034238827246,23.5691281055345));
#32696=CARTESIAN_POINT('Ctrl Pts',(-7.80811222454424,0.918798699112961,
23.5922820263836));
#32697=CARTESIAN_POINT('Ctrl Pts',(-8.31618157891577,1.13539003498842,23.6154359472327));
#32698=CARTESIAN_POINT('Ctrl Pts',(-8.86663745949497,1.09017279196971,23.6385898680818));
#32699=CARTESIAN_POINT('Ctrl Pts',(-9.33255073443314,0.793573574730505,
23.6617437889309));
#32700=CARTESIAN_POINT('Ctrl Pts',(-9.60648687545043,0.313984931283844,
23.68489770978));
#32701=CARTESIAN_POINT('Ctrl Pts',(-9.62527919239822,-0.238005215634009,
23.7080516306291));
#32702=CARTESIAN_POINT('Ctrl Pts',(-9.38459437934153,-0.735113957285921,
23.7312055514782));
#32703=CARTESIAN_POINT('Ctrl Pts',(-8.93993173826624,-1.062713412473,23.7543594723273));
#32704=CARTESIAN_POINT('Ctrl Pts',(-8.39382562130343,-1.14526275434153,
23.7775133931763));
#32705=CARTESIAN_POINT('Ctrl Pts',(-7.87220217589238,-0.963726915370522,
23.8006673140254));
#32706=CARTESIAN_POINT('Ctrl Pts',(-7.49534203616152,-0.559966274872751,
23.8238212348745));
#32707=CARTESIAN_POINT('Ctrl Pts',(-7.35014515766718,-0.0270832182785388,
23.8469751557236));
#32708=CARTESIAN_POINT('Ctrl Pts',(-7.47009210633745,0.512044313396504,
23.8701290765727));
#32709=CARTESIAN_POINT('Ctrl Pts',(-7.82752494038384,0.933101404044286,
23.8932829974218));
#32710=CARTESIAN_POINT('Ctrl Pts',(-8.34002229665421,1.13899256273153,23.9164369182709));
#32711=CARTESIAN_POINT('Ctrl Pts',(-8.88941022259596,1.08225128636912,23.9395908391199));
#32712=CARTESIAN_POINT('Ctrl Pts',(-9.34899953730467,0.775941285621684,
23.962744759969));
#32713=CARTESIAN_POINT('Ctrl Pts',(-9.61282398158819,0.290742017634264,
23.9858986808181));
#32714=CARTESIAN_POINT('Ctrl Pts',(-9.62001461877971,-0.261558033836305,
24.0090526016672));
#32715=CARTESIAN_POINT('Ctrl Pts',(-9.45263581774029,-0.5894219298223,24.0244885488999));
#32716=CARTESIAN_POINT('Ctrl Pts',(-9.33552724893067,-0.724480616192588,
24.0322065225163));
#32717=CARTESIAN_POINT('Ctrl Pts',(-8.77151818897635,1.01439039972537,22.7033804324511));
#32718=CARTESIAN_POINT('Ctrl Pts',(-8.9354891845709,0.9705008796939,22.7110984060675));
#32719=CARTESIAN_POINT('Ctrl Pts',(-9.24159996085188,0.801739314609559,
22.7265343533002));
#32720=CARTESIAN_POINT('Ctrl Pts',(-9.5298667171107,0.363576105985816,22.7496882741493));
#32721=CARTESIAN_POINT('Ctrl Pts',(-9.58060352778217,-0.158392802206884,
22.7728421949984));
#32722=CARTESIAN_POINT('Ctrl Pts',(-9.38218728088471,-0.643862307874607,
22.7959961158475));
#32723=CARTESIAN_POINT('Ctrl Pts',(-8.98033732459186,-0.980856251287975,
22.8191500366966));
#32724=CARTESIAN_POINT('Ctrl Pts',(-8.46773159856383,-1.09168003520905,
22.8423039575456));
#32725=CARTESIAN_POINT('Ctrl Pts',(-7.96256435570351,-0.950772483907168,
22.8654578783947));
#32726=CARTESIAN_POINT('Ctrl Pts',(-7.58132493358492,-0.590628072508616,
22.8886117992438));
#32727=CARTESIAN_POINT('Ctrl Pts',(-7.41192150776329,-0.0942908663522186,
22.9117657200929));
#32728=CARTESIAN_POINT('Ctrl Pts',(-7.49341734739136,0.42378859797782,22.934919640942));
#32729=CARTESIAN_POINT('Ctrl Pts',(-7.8070200875659,0.844147109967134,22.9580735617911));
#32730=CARTESIAN_POINT('Ctrl Pts',(-8.28041649441091,1.06985445126566,22.9812274826402));
#32731=CARTESIAN_POINT('Ctrl Pts',(-8.80444644598594,1.04886502357001,23.0043814034893));
#32732=CARTESIAN_POINT('Ctrl Pts',(-9.25827437168355,0.786018734512268,
23.0275353243383));
#32733=CARTESIAN_POINT('Ctrl Pts',(-9.53725247992004,0.341925088064882,
23.0506892451874));
#32734=CARTESIAN_POINT('Ctrl Pts',(-9.57705146305377,-0.181012762127038,
23.0738431660365));
#32735=CARTESIAN_POINT('Ctrl Pts',(-9.36849410607509,-0.662211039666914,
23.0969970868856));
#32736=CARTESIAN_POINT('Ctrl Pts',(-8.95967146580877,-0.990710662730691,
23.1201510077347));
#32737=CARTESIAN_POINT('Ctrl Pts',(-8.44485359076759,-1.09076319479888,
23.1433049285838));
#32738=CARTESIAN_POINT('Ctrl Pts',(-7.94275187728475,-0.9392976117019,23.1664588494329));
#32739=CARTESIAN_POINT('Ctrl Pts',(-7.56914551290379,-0.57124022746164,
23.189612770282));
#32740=CARTESIAN_POINT('Ctrl Pts',(-7.41018405705432,-0.071461067103083,
23.212766691131));
#32741=CARTESIAN_POINT('Ctrl Pts',(-7.50252229047412,0.444796237186593,
23.2359206119801));
#32742=CARTESIAN_POINT('Ctrl Pts',(-7.82486802203328,0.858488372629229,
23.2590745328292));
#32743=CARTESIAN_POINT('Ctrl Pts',(-8.30289183609866,1.07422243755091,23.2822284536783));
#32744=CARTESIAN_POINT('Ctrl Pts',(-8.82636664642078,1.04225250573838,23.3053823745274));
#32745=CARTESIAN_POINT('Ctrl Pts',(-9.27458486193219,0.769950495343321,
23.3285362953765));
#32746=CARTESIAN_POINT('Ctrl Pts',(-9.54419224285041,0.320106284825893,
23.3516902162256));
#32747=CARTESIAN_POINT('Ctrl Pts',(-9.57302026292976,-0.203550949288119,
23.3748441370746));
#32748=CARTESIAN_POINT('Ctrl Pts',(-9.35442149465265,-0.680271550992258,
23.3979980579237));
#32749=CARTESIAN_POINT('Ctrl Pts',(-8.9388024336295,-1.00012894061475,23.4211519787728));
#32750=CARTESIAN_POINT('Ctrl Pts',(-8.42200030959576,-1.08936748708124,
23.4443058996219));
#32751=CARTESIAN_POINT('Ctrl Pts',(-7.92318406481855,-0.927409753311392,
23.467459820471));
#32752=CARTESIAN_POINT('Ctrl Pts',(-7.55737529366215,-0.551601429123941,
23.4906137413201));
#32753=CARTESIAN_POINT('Ctrl Pts',(-7.40892551540569,-0.0485998218600163,
23.5137676621692));
#32754=CARTESIAN_POINT('Ctrl Pts',(-7.51206563243278,0.465608375137441,
23.5369215830183));
#32755=CARTESIAN_POINT('Ctrl Pts',(-7.84301265684497,0.872452350855443,
23.5600755038674));
#32756=CARTESIAN_POINT('Ctrl Pts',(-8.32545380858691,1.07811831483852,23.5832294247164));
#32757=CARTESIAN_POINT('Ctrl Pts',(-8.84814341134448,1.03518193496667,23.6063833455655));
#32758=CARTESIAN_POINT('Ctrl Pts',(-9.29055493457258,0.753543873667659,
23.6295372664146));
#32759=CARTESIAN_POINT('Ctrl Pts',(-9.55067309804575,0.298146799398216,
23.6526911872637));
#32760=CARTESIAN_POINT('Ctrl Pts',(-9.56851748671864,-0.225999677727252,
23.6758451081128));
#32761=CARTESIAN_POINT('Ctrl Pts',(-9.33997337670931,-0.698033095606178,
23.6989990289619));
#32762=CARTESIAN_POINT('Ctrl Pts',(-8.91774055583324,-1.0091076705842,23.722152949811));
#32763=CARTESIAN_POINT('Ctrl Pts',(-8.39918130447521,-1.08749303121249,
23.74530687066));
#32764=CARTESIAN_POINT('Ctrl Pts',(-7.90386976164266,-0.915114283149746,
23.7684607915091));
#32765=CARTESIAN_POINT('Ctrl Pts',(-7.54601932588418,-0.531720270592626,
23.7916147123582));
#32766=CARTESIAN_POINT('Ctrl Pts',(-7.40814651641942,-0.0257170776130338,
23.8147686332073));
#32767=CARTESIAN_POINT('Ctrl Pts',(-7.52204306138227,0.486215604567391,
23.8379225540564));
#32768=CARTESIAN_POINT('Ctrl Pts',(-7.86144615004332,0.886033594008022,
23.8610764749055));
#32769=CARTESIAN_POINT('Ctrl Pts',(-8.3480919449459,1.08153912268417,23.8842303957546));
#32770=CARTESIAN_POINT('Ctrl Pts',(-8.86976746318751,1.02766000857494,23.9073843166037));
#32771=CARTESIAN_POINT('Ctrl Pts',(-9.30617402148235,0.736800998325318,
23.9305382374527));
#32772=CARTESIAN_POINT('Ctrl Pts',(-9.55669054577707,0.276076312496261,
23.9536921583018));
#32773=CARTESIAN_POINT('Ctrl Pts',(-9.56351847046606,-0.248364436873845,
23.9768460791509));
#32774=CARTESIAN_POINT('Ctrl Pts',(-9.40458264633919,-0.559690113640436,
23.9922820263836));
#32775=CARTESIAN_POINT('Ctrl Pts',(-9.2933813067401,-0.687936125025699,
24.));
#32776=CARTESIAN_POINT('Ctrl Pts',(-9.2933813067401,-0.687936125025699,
24.));
#32777=CARTESIAN_POINT('Ctrl Pts',(-9.32590110166393,-0.655902301852627,
24.));
#32778=CARTESIAN_POINT('Ctrl Pts',(-9.35618485076755,-0.621808682852868,
24.));
#32779=CARTESIAN_POINT('Ctrl Pts',(-9.38414220215367,-0.585954725174177,
24.));
#32780=CARTESIAN_POINT('Ctrl Pts',(-9.41249843269251,-0.549589224178562,
24.));
#32781=CARTESIAN_POINT('Ctrl Pts',(-9.43846213639955,-0.511412007721187,
24.));
#32782=CARTESIAN_POINT('Ctrl Pts',(-9.4619086878745,-0.471690294888102,
24.));
#32783=CARTESIAN_POINT('Ctrl Pts',(-9.48267051934571,-0.436516870409484,
24.));
#32784=CARTESIAN_POINT('Ctrl Pts',(-9.50145853320447,-0.400131340040127,
24.));
#32785=CARTESIAN_POINT('Ctrl Pts',(-9.51815973041198,-0.362698054803428,
24.));
#32786=CARTESIAN_POINT('Ctrl Pts',(-9.52288697181288,-0.352102636190975,
24.));
#32787=CARTESIAN_POINT('Ctrl Pts',(-9.52744818249553,-0.34141946758306,
24.));
#32788=CARTESIAN_POINT('Ctrl Pts',(-9.53183041159058,-0.330677835735727,
24.));
#32789=CARTESIAN_POINT('Ctrl Pts',(-9.54293046193044,-0.303469615523773,
24.));
#32790=CARTESIAN_POINT('Ctrl Pts',(-9.55289673212501,-0.275856964651056,
24.));
#32791=CARTESIAN_POINT('Ctrl Pts',(-9.56170183443649,-0.2479085208202,24.));
#32792=CARTESIAN_POINT('Ctrl Pts',(-9.57582144309734,-0.203091200633333,
24.));
#32793=CARTESIAN_POINT('Ctrl Pts',(-9.58695791901247,-0.157411543429852,
24.));
#32794=CARTESIAN_POINT('Ctrl Pts',(-9.59514654937063,-0.111173006432213,
24.));
#32795=CARTESIAN_POINT('Ctrl Pts',(-9.60093321692656,-0.0784975735239973,
24.));
#32796=CARTESIAN_POINT('Ctrl Pts',(-9.60524681862521,-0.0455423057826866,
24.));
#32797=CARTESIAN_POINT('Ctrl Pts',(-9.60808517048093,-0.0124084983709903,
24.));
#32798=CARTESIAN_POINT('Ctrl Pts',(-9.60984391284602,0.00812237087063378,
24.));
#32799=CARTESIAN_POINT('Ctrl Pts',(-9.61103599498872,0.0287218666781537,
24.));
#32800=CARTESIAN_POINT('Ctrl Pts',(-9.61165846902993,0.0493662487424586,
24.));
#32801=CARTESIAN_POINT('Ctrl Pts',(-9.6120205910809,0.0613760442993463,
24.));
#32802=CARTESIAN_POINT('Ctrl Pts',(-9.61218973047166,0.0734054549032458,
24.));
#32803=CARTESIAN_POINT('Ctrl Pts',(-9.61216556829573,0.0854209765709245,
24.));
#32804=CARTESIAN_POINT('Ctrl Pts',(-9.61206835676509,0.133762949416384,
24.));
#32805=CARTESIAN_POINT('Ctrl Pts',(-9.60885086759177,0.181961282887962,
24.));
#32806=CARTESIAN_POINT('Ctrl Pts',(-9.60254527348847,0.229705031101198,
24.));
#32807=CARTESIAN_POINT('Ctrl Pts',(-9.60006866958979,0.248457007683516,
24.));
#32808=CARTESIAN_POINT('Ctrl Pts',(-9.59711514423865,0.267139045895045,
24.));
#32809=CARTESIAN_POINT('Ctrl Pts',(-9.59368451474868,0.285732798488276,
24.));
#32810=CARTESIAN_POINT('Ctrl Pts',(-9.58524456415484,0.331476692924977,
24.));
#32811=CARTESIAN_POINT('Ctrl Pts',(-9.57392018758713,0.376686672569883,
24.));
#32812=CARTESIAN_POINT('Ctrl Pts',(-9.55984155019052,0.421132731117061,
24.));
#32813=CARTESIAN_POINT('Ctrl Pts',(-9.55380134842738,0.440201562399408,
24.));
#32814=CARTESIAN_POINT('Ctrl Pts',(-9.54725359771895,0.45912971099526,24.));
#32815=CARTESIAN_POINT('Ctrl Pts',(-9.54020607939479,0.477898435611738,
24.));
#32816=CARTESIAN_POINT('Ctrl Pts',(-9.53575725876718,0.489746391925897,
24.));
#32817=CARTESIAN_POINT('Ctrl Pts',(-9.53110712095903,0.501535526186162,
24.));
#32818=CARTESIAN_POINT('Ctrl Pts',(-9.52626970531564,0.513232427219491,
24.));
#32819=CARTESIAN_POINT('Ctrl Pts',(-9.50753148918547,0.55854155005979,24.));
#32820=CARTESIAN_POINT('Ctrl Pts',(-9.4859625052079,0.602540197938336,24.));
#32821=CARTESIAN_POINT('Ctrl Pts',(-9.4617427066771,0.644974417278716,24.));
#32822=CARTESIAN_POINT('Ctrl Pts',(-9.43730180712568,0.687796015944042,
24.));
#32823=CARTESIAN_POINT('Ctrl Pts',(-9.41016114958247,0.729025575350205,
24.));
#32824=CARTESIAN_POINT('Ctrl Pts',(-9.38045478374864,0.768390402360951,
24.));
#32825=CARTESIAN_POINT('Ctrl Pts',(-9.37505686111558,0.775543357113344,
24.));
#32826=CARTESIAN_POINT('Ctrl Pts',(-9.36957409662013,0.782634685144143,
24.));
#32827=CARTESIAN_POINT('Ctrl Pts',(-9.36400712941827,0.789662665096707,
24.));
#32828=CARTESIAN_POINT('Ctrl Pts',(-9.34882977059882,0.808823218706664,
24.));
#32829=CARTESIAN_POINT('Ctrl Pts',(-9.33302672335631,0.827513061791383,
24.));
#32830=CARTESIAN_POINT('Ctrl Pts',(-9.31662622921216,0.845711532137706,
24.));
#32831=CARTESIAN_POINT('Ctrl Pts',(-9.30887406128153,0.854313565525556,
24.));
#32832=CARTESIAN_POINT('Ctrl Pts',(-9.30098837274836,0.86280578480931,24.));
#32833=CARTESIAN_POINT('Ctrl Pts',(-9.29297196496173,0.871185840868798,
24.));
#32834=CARTESIAN_POINT('Ctrl Pts',(-9.28554430284086,0.878950443995364,
24.));
#32835=CARTESIAN_POINT('Ctrl Pts',(-9.27801012459867,0.886612714734314,
24.));
#32836=CARTESIAN_POINT('Ctrl Pts',(-9.27037601768741,0.894167467518663,
24.));
#32837=CARTESIAN_POINT('Ctrl Pts',(-9.23471802897501,0.929454802715901,
24.));
#32838=CARTESIAN_POINT('Ctrl Pts',(-9.19685809573334,0.962425263167257,
24.));
#32839=CARTESIAN_POINT('Ctrl Pts',(-9.15706756650192,0.992923322602774,
24.));
#32840=CARTESIAN_POINT('Ctrl Pts',(-9.1348197718603,1.00997548492369,24.));
#32841=CARTESIAN_POINT('Ctrl Pts',(-9.11196761308139,1.02625423452634,24.));
#32842=CARTESIAN_POINT('Ctrl Pts',(-9.08855317728612,1.04172777569958,24.));
#32843=CARTESIAN_POINT('Ctrl Pts',(-9.0763658218002,1.04978184749329,24.));
#32844=CARTESIAN_POINT('Ctrl Pts',(-9.06402384207715,1.05761883806443,24.));
#32845=CARTESIAN_POINT('Ctrl Pts',(-9.05155327718193,1.06522206442192,24.));
#32846=CARTESIAN_POINT('Ctrl Pts',(-9.00599330223546,1.09299969961885,24.));
#32847=CARTESIAN_POINT('Ctrl Pts',(-8.95866621855187,1.11769815363806,24.));
#32848=CARTESIAN_POINT('Ctrl Pts',(-8.90987130699021,1.13911688142547,24.));
#32849=CARTESIAN_POINT('Ctrl Pts',(-8.87875612767952,1.15277501778401,24.));
#32850=CARTESIAN_POINT('Ctrl Pts',(-8.84704312712587,1.16509870240582,24.));
#32851=CARTESIAN_POINT('Ctrl Pts',(-8.81482199187078,1.17607957877115,24.));
#32852=CARTESIAN_POINT('Ctrl Pts',(-9.55005297345142,-1.9100363332081E-5,
23.0658930328476));
#32853=CARTESIAN_POINT('Ctrl Pts',(-9.55009366141186,-0.0583092414421507,
23.0685430772439));
#32854=CARTESIAN_POINT('Ctrl Pts',(-9.5453162224635,-0.116592782065231,
23.0711931216402));
#32855=CARTESIAN_POINT('Ctrl Pts',(-9.5356587397017,-0.174056166685031,
23.0738431660365));
#32856=CARTESIAN_POINT('Ctrl Pts',(-9.50753234406088,-0.341412187973663,
23.0815611396529));
#32857=CARTESIAN_POINT('Ctrl Pts',(-9.43801322506799,-0.501811613820288,
23.0892791132692));
#32858=CARTESIAN_POINT('Ctrl Pts',(-9.33511655886048,-0.636761263920897,
23.0969970868856));
#32859=CARTESIAN_POINT('Ctrl Pts',(-9.23221989265299,-0.771710914021506,
23.104715060502));
#32860=CARTESIAN_POINT('Ctrl Pts',(-9.09594567923088,-0.881210788376099,
23.1124330341183));
#32861=CARTESIAN_POINT('Ctrl Pts',(-8.94200559334629,-0.952636147564761,
23.1201510077347));
#32862=CARTESIAN_POINT('Ctrl Pts',(-8.78806550746171,-1.02406150675342,
23.127868981351));
#32863=CARTESIAN_POINT('Ctrl Pts',(-8.61645954911465,-1.05741235077615,
23.1355869549674));
#32864=CARTESIAN_POINT('Ctrl Pts',(-8.44697295102731,-1.04884350893802,
23.1433049285838));
#32865=CARTESIAN_POINT('Ctrl Pts',(-8.27748635293998,-1.04027466709989,
23.1510229022002));
#32866=CARTESIAN_POINT('Ctrl Pts',(-8.11011911511237,-0.989786139400895,
23.1587408758165));
#32867=CARTESIAN_POINT('Ctrl Pts',(-7.96416776880173,-0.903198978178021,
23.1664588494329));
#32868=CARTESIAN_POINT('Ctrl Pts',(-7.8182164224911,-0.816611816955147,
23.1741768230492));
#32869=CARTESIAN_POINT('Ctrl Pts',(-7.69368096769745,-0.693926022208393,
23.1818947966656));
#32870=CARTESIAN_POINT('Ctrl Pts',(-7.60491966432571,-0.54928659810859,
23.189612770282));
#32871=CARTESIAN_POINT('Ctrl Pts',(-7.51615836095397,-0.404647174008787,
23.1973307438983));
#32872=CARTESIAN_POINT('Ctrl Pts',(-7.46317120900415,-0.238054120555935,
23.2050487175147));
#32873=CARTESIAN_POINT('Ctrl Pts',(-7.4520673385992,-0.0687147097812286,
23.212766691131));
#32874=CARTESIAN_POINT('Ctrl Pts',(-7.44096346819426,0.100624700993478,
23.2204846647474));
#32875=CARTESIAN_POINT('Ctrl Pts',(-7.47174287933419,0.272710469090037,
23.2282026383638));
#32876=CARTESIAN_POINT('Ctrl Pts',(-7.54085687349735,0.427702042378756,
23.2359206119801));
#32877=CARTESIAN_POINT('Ctrl Pts',(-7.60997086766051,0.582693615667473,
23.2436385855965));
#32878=CARTESIAN_POINT('Ctrl Pts',(-7.71741944484689,0.720590994148351,
23.2513565592129));
#32879=CARTESIAN_POINT('Ctrl Pts',(-7.85081436911765,0.825495360875735,
23.2590745328292));
#32880=CARTESIAN_POINT('Ctrl Pts',(-7.9842092933884,0.930399727603121,23.2667925064456));
#32881=CARTESIAN_POINT('Ctrl Pts',(-8.14355056474353,1.00231108257701,23.2745104800619));
#32882=CARTESIAN_POINT('Ctrl Pts',(-8.31046700214145,1.03293843809521,23.2822284536783));
#32883=CARTESIAN_POINT('Ctrl Pts',(-8.47738343953937,1.0635657936134,23.2899464272947));
#32884=CARTESIAN_POINT('Ctrl Pts',(-8.65187504298008,1.05290914967589,23.297664400911));
#32885=CARTESIAN_POINT('Ctrl Pts',(-8.813823880619,1.00219715930796,23.3053823745274));
#32886=CARTESIAN_POINT('Ctrl Pts',(-8.97577271825792,0.951485168940026,
23.3131003481438));
#32887=CARTESIAN_POINT('Ctrl Pts',(-9.12517879009505,0.860717832141674,
23.3208183217601));
#32888=CARTESIAN_POINT('Ctrl Pts',(-9.24481638949999,0.740360128656261,
23.3285362953765));
#32889=CARTESIAN_POINT('Ctrl Pts',(-9.36445398890493,0.620002425170845,
23.3362542689928));
#32890=CARTESIAN_POINT('Ctrl Pts',(-9.45432311587767,0.470054354998369,
23.3439722426092));
#32891=CARTESIAN_POINT('Ctrl Pts',(-9.50406234937726,0.307804114226461,
23.3516902162256));
#32892=CARTESIAN_POINT('Ctrl Pts',(-9.53457282822537,0.208278404020019,
23.3564244884329));
#32893=CARTESIAN_POINT('Ctrl Pts',(-9.54998362241142,0.104123753125398,
23.3611587606403));
#32894=CARTESIAN_POINT('Ctrl Pts',(-9.55003901931283,-1.48519368357603E-5,
23.3658930328476));
#32895=CARTESIAN_POINT('Ctrl Pts',(-8.81478889550448,1.17604951161381,22.8));
#32896=CARTESIAN_POINT('Ctrl Pts',(-8.86280031082267,1.1596387533803,22.8));
#32897=CARTESIAN_POINT('Ctrl Pts',(-8.90960753249362,1.1402211917786,22.8));
#32898=CARTESIAN_POINT('Ctrl Pts',(-8.95497271964666,1.11798779949959,22.8));
#32899=CARTESIAN_POINT('Ctrl Pts',(-9.00031627609065,1.0957650083901,22.8));
#32900=CARTESIAN_POINT('Ctrl Pts',(-9.04422007096444,1.07072837077275,22.8));
#32901=CARTESIAN_POINT('Ctrl Pts',(-9.08641936496114,1.04302434852895,22.8));
#32902=CARTESIAN_POINT('Ctrl Pts',(-9.125198107991,1.01756593305001,22.8));
#32903=CARTESIAN_POINT('Ctrl Pts',(-9.16253770006956,0.989854158189036,
22.8));
#32904=CARTESIAN_POINT('Ctrl Pts',(-9.19820266623766,0.959977147630981,
22.8));
#32905=CARTESIAN_POINT('Ctrl Pts',(-9.20529843014922,0.954032933011403,
22.8));
#32906=CARTESIAN_POINT('Ctrl Pts',(-9.21232944776528,0.948001491271412,
22.8));
#32907=CARTESIAN_POINT('Ctrl Pts',(-9.21928835806176,0.941888130657366,
22.8));
#32908=CARTESIAN_POINT('Ctrl Pts',(-9.24730655571085,0.917274313452249,
22.8));
#32909=CARTESIAN_POINT('Ctrl Pts',(-9.27408721843744,0.89139578122503,22.8));
#32910=CARTESIAN_POINT('Ctrl Pts',(-9.29952889345206,0.864316883517271,
22.8));
#32911=CARTESIAN_POINT('Ctrl Pts',(-9.33347331898954,0.828188066277435,
22.8));
#32912=CARTESIAN_POINT('Ctrl Pts',(-9.36503615316936,0.789923068886875,
22.8));
#32913=CARTESIAN_POINT('Ctrl Pts',(-9.39406761371715,0.749788140423142,
22.8));
#32914=CARTESIAN_POINT('Ctrl Pts',(-9.41426285222677,0.721868964549862,
22.8));
#32915=CARTESIAN_POINT('Ctrl Pts',(-9.43323229228493,0.69304419080465,22.8));
#32916=CARTESIAN_POINT('Ctrl Pts',(-9.45091180542575,0.663397698483226,
22.8));
#32917=CARTESIAN_POINT('Ctrl Pts',(-9.46034264350897,0.64758327720412,22.8));
#32918=CARTESIAN_POINT('Ctrl Pts',(-9.46940623093581,0.63153497639394,22.8));
#32919=CARTESIAN_POINT('Ctrl Pts',(-9.47809138410351,0.615265273228403,
22.8));
#32920=CARTESIAN_POINT('Ctrl Pts',(-9.48251083054356,0.6069864230634,22.8));
#32921=CARTESIAN_POINT('Ctrl Pts',(-9.48683227267676,0.598650243698863,
22.8));
#32922=CARTESIAN_POINT('Ctrl Pts',(-9.49105413080523,0.590258373551913,
22.8));
#32923=CARTESIAN_POINT('Ctrl Pts',(-9.49557643033991,0.581269310133437,
22.8));
#32924=CARTESIAN_POINT('Ctrl Pts',(-9.49998109806241,0.572222892914978,
22.8));
#32925=CARTESIAN_POINT('Ctrl Pts',(-9.5042634003018,0.563128708694731,22.8));
#32926=CARTESIAN_POINT('Ctrl Pts',(-9.52493465811296,0.519229839327299,
22.8));
#32927=CARTESIAN_POINT('Ctrl Pts',(-9.54278515814712,0.47416665717555,22.8));
#32928=CARTESIAN_POINT('Ctrl Pts',(-9.55766739651793,0.428186626834186,
22.8));
#32929=CARTESIAN_POINT('Ctrl Pts',(-9.56297835233027,0.411777945336887,
22.8));
#32930=CARTESIAN_POINT('Ctrl Pts',(-9.56791083552882,0.395252350342727,
22.8));
#32931=CARTESIAN_POINT('Ctrl Pts',(-9.57245656690096,0.378620722213359,
22.8));
#32932=CARTESIAN_POINT('Ctrl Pts',(-9.58437742872468,0.335005443481923,
22.8));
#32933=CARTESIAN_POINT('Ctrl Pts',(-9.59364131934433,0.29066065148619,22.8));
#32934=CARTESIAN_POINT('Ctrl Pts',(-9.60021803028088,0.245833620405334,
22.8));
#32935=CARTESIAN_POINT('Ctrl Pts',(-9.60298164316936,0.226996763799839,
22.8));
#32936=CARTESIAN_POINT('Ctrl Pts',(-9.6052702833904,0.208074803263039,22.8));
#32937=CARTESIAN_POINT('Ctrl Pts',(-9.60707964983028,0.189086526821981,
22.8));
#32938=CARTESIAN_POINT('Ctrl Pts',(-9.60796954273001,0.179747604638758,
22.8));
#32939=CARTESIAN_POINT('Ctrl Pts',(-9.60874361971098,0.170390676282926,
22.8));
#32940=CARTESIAN_POINT('Ctrl Pts',(-9.60940083091284,0.161024279585984,
22.8));
#32941=CARTESIAN_POINT('Ctrl Pts',(-9.61273685317894,0.113480190493206,
22.8));
#32942=CARTESIAN_POINT('Ctrl Pts',(-9.6130541030529,0.0658798367366342,
22.8));
#32943=CARTESIAN_POINT('Ctrl Pts',(-9.6103552475085,0.0185121206120323,
22.8));
#32944=CARTESIAN_POINT('Ctrl Pts',(-9.60768697144596,-0.0283188938653337,
22.8));
#32945=CARTESIAN_POINT('Ctrl Pts',(-9.60207037041557,-0.0749235858009301,
22.8));
#32946=CARTESIAN_POINT('Ctrl Pts',(-9.5934585486852,-0.121013695903488,
22.8));
#32947=CARTESIAN_POINT('Ctrl Pts',(-9.59107666009507,-0.133761464123487,
22.8));
#32948=CARTESIAN_POINT('Ctrl Pts',(-9.58846535604412,-0.146469761698218,
22.8));
#32949=CARTESIAN_POINT('Ctrl Pts',(-9.5856229921747,-0.159132198493557,
22.8));
#32950=CARTESIAN_POINT('Ctrl Pts',(-9.58068428043452,-0.181133648038205,
22.8));
#32951=CARTESIAN_POINT('Ctrl Pts',(-9.57504809566159,-0.202996740245752,
22.8));
#32952=CARTESIAN_POINT('Ctrl Pts',(-9.56872438197767,-0.224689669718014,
22.8));
#32953=CARTESIAN_POINT('Ctrl Pts',(-9.565514395063,-0.235701240327858,22.8));
#32954=CARTESIAN_POINT('Ctrl Pts',(-9.56212721978399,-0.246668938836283,
22.8));
#32955=CARTESIAN_POINT('Ctrl Pts',(-9.55856395930746,-0.257588424518991,
22.8));
#32956=CARTESIAN_POINT('Ctrl Pts',(-9.55533539309684,-0.267482251463418,
22.8));
#32957=CARTESIAN_POINT('Ctrl Pts',(-9.55196486814714,-0.27732838971353,
22.8));
#32958=CARTESIAN_POINT('Ctrl Pts',(-9.54845535758285,-0.287119798241869,
22.8));
#32959=CARTESIAN_POINT('Ctrl Pts',(-9.53268065995049,-0.331130638528512,
22.8));
#32960=CARTESIAN_POINT('Ctrl Pts',(-9.51409256034865,-0.374065139761816,
22.8));
#32961=CARTESIAN_POINT('Ctrl Pts',(-9.49280975524792,-0.415648691358816,
22.8));
#32962=CARTESIAN_POINT('Ctrl Pts',(-9.48095738273575,-0.438806528945255,
22.8));
#32963=CARTESIAN_POINT('Ctrl Pts',(-9.46826849283286,-0.461544912508254,
22.8));
#32964=CARTESIAN_POINT('Ctrl Pts',(-9.45475828805827,-0.48381173664456,
22.8));
#32965=CARTESIAN_POINT('Ctrl Pts',(-9.44902455967591,-0.493261772648128,
22.8));
#32966=CARTESIAN_POINT('Ctrl Pts',(-9.44314343602737,-0.502625630023286,
22.8));
#32967=CARTESIAN_POINT('Ctrl Pts',(-9.43712292970736,-0.511889198807362,
22.8));
#32968=CARTESIAN_POINT('Ctrl Pts',(-9.41182985269796,-0.550806882168746,
22.8));
#32969=CARTESIAN_POINT('Ctrl Pts',(-9.38404968213532,-0.588007909962575,
22.8));
#32970=CARTESIAN_POINT('Ctrl Pts',(-9.35388377160583,-0.62320506690565,
22.8));
#32971=CARTESIAN_POINT('Ctrl Pts',(-9.33467713894622,-0.645615093727404,
22.8));
#32972=CARTESIAN_POINT('Ctrl Pts',(-9.31450246278731,-0.667212005822818,
22.8));
#32973=CARTESIAN_POINT('Ctrl Pts',(-9.29341948377037,-0.687941604344758,
22.8));
#32974=CARTESIAN_POINT('Origin',(-8.5,0.,24.));
#32975=CARTESIAN_POINT('',(-7.46076951545867,-1.8,24.));
#32976=CARTESIAN_POINT('',(-6.42153903091735,0.,24.));
#32977=CARTESIAN_POINT('',(-7.46076951545867,-1.8,24.));
#32978=CARTESIAN_POINT('',(-7.46076951545867,1.8,24.));
#32979=CARTESIAN_POINT('',(-6.42153903091735,0.,24.));
#32980=CARTESIAN_POINT('',(-9.53923048454133,1.8,24.));
#32981=CARTESIAN_POINT('',(-7.46076951545867,1.8,24.));
#32982=CARTESIAN_POINT('',(-10.5784609690827,2.22044604925031E-16,24.));
#32983=CARTESIAN_POINT('',(-9.53923048454133,1.8,24.));
#32984=CARTESIAN_POINT('',(-9.53923048454133,-1.8,24.));
#32985=CARTESIAN_POINT('',(-10.5784609690827,2.54538057293978E-16,24.));
#32986=CARTESIAN_POINT('',(-9.53923048454133,-1.8,24.));
#32987=CARTESIAN_POINT('Origin',(-8.5,0.,22.7));
#32988=CARTESIAN_POINT('Origin',(-9.53923048454133,-1.8,22.8));
#32989=CARTESIAN_POINT('',(-9.53923048454133,-1.8,22.8));
#32990=CARTESIAN_POINT('',(-7.46076951545867,-1.8,22.8));
#32991=CARTESIAN_POINT('',(-9.53923048454133,-1.8,22.8));
#32992=CARTESIAN_POINT('',(-7.46076951545867,-1.8,22.8));
#32993=CARTESIAN_POINT('',(-9.53923048454133,-1.8,22.8));
#32994=CARTESIAN_POINT('Origin',(-10.5784609690827,2.54538057293978E-16,
22.8));
#32995=CARTESIAN_POINT('',(-10.5784609690827,2.54538057293978E-16,22.8));
#32996=CARTESIAN_POINT('',(-10.5784609690827,2.54538057293978E-16,22.8));
#32997=CARTESIAN_POINT('',(-10.5784609690827,2.54538057293978E-16,22.8));
#32998=CARTESIAN_POINT('Origin',(-9.53923048454133,1.8,22.8));
#32999=CARTESIAN_POINT('',(-9.53923048454133,1.8,22.8));
#33000=CARTESIAN_POINT('',(-9.53923048454133,1.8,22.8));
#33001=CARTESIAN_POINT('',(-9.53923048454133,1.8,22.8));
#33002=CARTESIAN_POINT('Origin',(-7.46076951545867,1.8,22.8));
#33003=CARTESIAN_POINT('',(-7.46076951545867,1.8,22.8));
#33004=CARTESIAN_POINT('',(-7.46076951545867,1.8,22.8));
#33005=CARTESIAN_POINT('',(-7.46076951545867,1.8,22.8));
#33006=CARTESIAN_POINT('Origin',(-6.42153903091735,0.,22.8));
#33007=CARTESIAN_POINT('',(-6.42153903091735,0.,22.8));
#33008=CARTESIAN_POINT('',(-6.42153903091735,0.,22.8));
#33009=CARTESIAN_POINT('',(-6.42153903091735,0.,22.8));
#33010=CARTESIAN_POINT('Origin',(-7.46076951545867,-1.8,22.8));
#33011=CARTESIAN_POINT('',(-7.46076951545867,-1.8,22.8));
#33012=CARTESIAN_POINT('Origin',(-8.5,0.,22.8));
#33013=CARTESIAN_POINT('',(0.,0.,0.));
#33014=CARTESIAN_POINT('',(0.,0.,0.));
#33015=CARTESIAN_POINT('',(0.,0.,0.));
#33016=CARTESIAN_POINT('Origin',(-8.5,0.,25.1));
#33017=CARTESIAN_POINT('',(-9.55012868473597,-2.18483901666677E-5,26.2841069671524));
#33018=CARTESIAN_POINT('',(-9.55000808233714,1.77385175400095E-6,26.3658930328476));
#33019=CARTESIAN_POINT('',(-9.5501,-1.28600160378464E-16,25.1));
#33020=CARTESIAN_POINT('',(-9.29338130674011,-0.687936125025682,26.4));
#33021=CARTESIAN_POINT('Ctrl Pts',(-9.55000808233714,1.77385175400095E-6,
26.3658930328476));
#33022=CARTESIAN_POINT('Ctrl Pts',(-9.55001544756934,-0.0803124474913518,
26.3695440482821));
#33023=CARTESIAN_POINT('Ctrl Pts',(-9.54090375927775,-0.160621737063475,
26.3731950637165));
#33024=CARTESIAN_POINT('Ctrl Pts',(-9.52264585408719,-0.238788344862009,
26.3768460791509));
#33025=CARTESIAN_POINT('Ctrl Pts',(-9.48405000778592,-0.404026708682781,
26.3845640527673));
#33026=CARTESIAN_POINT('Ctrl Pts',(-9.4045826463392,-0.559690113640417,
26.3922820263836));
#33027=CARTESIAN_POINT('Ctrl Pts',(-9.29338130674012,-0.687936125025676,
26.4));
#33028=CARTESIAN_POINT('',(-7.7065804240351,-0.68794180318535,26.4));
#33029=CARTESIAN_POINT('Origin',(-8.5,0.,26.4));
#33030=CARTESIAN_POINT('Ctrl Pts',(-7.7065804240351,-0.68794180318535,26.4));
#33031=CARTESIAN_POINT('Ctrl Pts',(-7.79864112035199,-0.793916326566851,
26.3936166544345));
#33032=CARTESIAN_POINT('Ctrl Pts',(-7.91206794128119,-0.881431589437098,
26.387233308869));
#33033=CARTESIAN_POINT('Ctrl Pts',(-8.0381219127883,-0.94316142252496,26.3808499633034));
#33034=CARTESIAN_POINT('Ctrl Pts',(-8.19053121232317,-1.01779771132126,
26.3731319896871));
#33035=CARTESIAN_POINT('Ctrl Pts',(-8.36139981181721,-1.05473895720253,
26.3654140160707));
#33036=CARTESIAN_POINT('Ctrl Pts',(-8.53102866379217,-1.04972498576314,
26.3576960424544));
#33037=CARTESIAN_POINT('Ctrl Pts',(-8.70065751576713,-1.04471101432375,
26.349978068838));
#33038=CARTESIAN_POINT('Ctrl Pts',(-8.869046620223,-0.997741825563708,26.3422600952216));
#33039=CARTESIAN_POINT('Ctrl Pts',(-9.01678108566738,-0.914233151702619,
26.3345421216053));
#33040=CARTESIAN_POINT('Ctrl Pts',(-9.16451555111177,-0.830724477841526,
26.3268241479889));
#33041=CARTESIAN_POINT('Ctrl Pts',(-9.29159537754465,-0.710676318879388,
26.3191061743726));
#33042=CARTESIAN_POINT('Ctrl Pts',(-9.38336919906597,-0.567929359810613,
26.3113882007562));
#33043=CARTESIAN_POINT('Ctrl Pts',(-9.47514302058727,-0.425182400741845,
26.3036702271398));
#33044=CARTESIAN_POINT('Ctrl Pts',(-9.53161083719701,-0.259736641566442,
26.2959522535235));
#33045=CARTESIAN_POINT('Ctrl Pts',(-9.54626210360576,-0.0906671713680419,
26.2882342799071));
#33046=CARTESIAN_POINT('Ctrl Pts',(-9.54887377180294,-0.0605296156023525,
26.2868585089889));
#33047=CARTESIAN_POINT('Ctrl Pts',(-9.55015671877703,-0.0302769163894044,
26.2854827380706));
#33048=CARTESIAN_POINT('Ctrl Pts',(-9.55012868473597,-2.18483901666677E-5,
26.2841069671524));
#33049=CARTESIAN_POINT('Origin',(-8.5,0.,25.1));
#33050=CARTESIAN_POINT('',(-9.55014863741965,-1.85392332084922E-5,25.9841069671524));
#33051=CARTESIAN_POINT('',(-9.55002929519846,-9.63122723742732E-6,26.0658930328476));
#33052=CARTESIAN_POINT('',(-9.5501,-1.28600160378464E-16,25.1));
#33053=CARTESIAN_POINT('Ctrl Pts',(-9.55002929519846,-9.63122723742732E-6,
26.0658930328476));
#33054=CARTESIAN_POINT('Ctrl Pts',(-9.55005413296486,-0.0729827234261202,
26.0692103912693));
#33055=CARTESIAN_POINT('Ctrl Pts',(-9.54254682320219,-0.145950776385278,
26.0725277496911));
#33056=CARTESIAN_POINT('Ctrl Pts',(-9.5274529085174,-0.21731420414845,26.0758451081128));
#33057=CARTESIAN_POINT('Ctrl Pts',(-9.49233628242652,-0.383344214364866,
26.0835630817291));
#33058=CARTESIAN_POINT('Ctrl Pts',(-9.41615489969101,-0.540688713228667,
26.0912810553455));
#33059=CARTESIAN_POINT('Ctrl Pts',(-9.3076920597651,-0.671206733850008,
26.0989990289619));
#33060=CARTESIAN_POINT('Ctrl Pts',(-9.19922921983919,-0.801724754471348,
26.1067170025782));
#33061=CARTESIAN_POINT('Ctrl Pts',(-9.05848492272286,-0.905416296850228,
26.1144349761946));
#33062=CARTESIAN_POINT('Ctrl Pts',(-8.90168621780771,-0.970326296905908,
26.1221529498109));
#33063=CARTESIAN_POINT('Ctrl Pts',(-8.74488751289256,-1.03523629696159,
26.1298709234273));
#33064=CARTESIAN_POINT('Ctrl Pts',(-8.57203440017859,-1.06136475469407,
26.1375888970437));
#33065=CARTESIAN_POINT('Ctrl Pts',(-8.40305590625563,-1.04569918755626,
26.14530687066));
#33066=CARTESIAN_POINT('Ctrl Pts',(-8.23407741233268,-1.03003362041845,
26.1530248442764));
#33067=CARTESIAN_POINT('Ctrl Pts',(-8.06897353720075,-0.972574028410342,
26.1607428178928));
#33068=CARTESIAN_POINT('Ctrl Pts',(-7.92677985019183,-0.879945219242199,
26.1684607915091));
#33069=CARTESIAN_POINT('Ctrl Pts',(-7.78458616318292,-0.787316410074058,
26.1761787651255));
#33070=CARTESIAN_POINT('Ctrl Pts',(-7.66530266429701,-0.659518383745877,
26.1838967387419));
#33071=CARTESIAN_POINT('Ctrl Pts',(-7.58268210950511,-0.511285491489167,
26.1916147123582));
#33072=CARTESIAN_POINT('Ctrl Pts',(-7.50006155471321,-0.363052599232457,
26.1993326859746));
#33073=CARTESIAN_POINT('Ctrl Pts',(-7.45410394401532,-0.194384841047217,
26.2070506595909));
#33074=CARTESIAN_POINT('Ctrl Pts',(-7.45010789815323,-0.0247288321007086,
26.2147686332073));
#33075=CARTESIAN_POINT('Ctrl Pts',(-7.44611185229113,0.144927176845799,
26.2224866068237));
#33076=CARTESIAN_POINT('Ctrl Pts',(-7.48407737126484,0.315571436553571,
26.23020458044));
#33077=CARTESIAN_POINT('Ctrl Pts',(-7.55962732154007,0.467529907730423,
26.2379225540564));
#33078=CARTESIAN_POINT('Ctrl Pts',(-7.63517727181531,0.619488378907277,
26.2456405276728));
#33079=CARTESIAN_POINT('Ctrl Pts',(-7.74831165339208,0.752761061553206,
26.2533585012891));
#33080=CARTESIAN_POINT('Ctrl Pts',(-7.88598648304016,0.851981672429286,
26.2610764749055));
#33081=CARTESIAN_POINT('Ctrl Pts',(-8.02366131268824,0.951202283305365,
26.2687944485219));
#33082=CARTESIAN_POINT('Ctrl Pts',(-8.18587659040763,1.0163708224116,26.2765124221382));
#33083=CARTESIAN_POINT('Ctrl Pts',(-8.35393016091651,1.03997523612929,26.2842303957546));
#33084=CARTESIAN_POINT('Ctrl Pts',(-8.52198373142539,1.06357964984699,26.2919483693709));
#33085=CARTESIAN_POINT('Ctrl Pts',(-8.69587559472376,1.04561993817614,26.2996663429873));
#33086=CARTESIAN_POINT('Ctrl Pts',(-8.85555592518767,0.988163616219066,
26.3073843166036));
#33087=CARTESIAN_POINT('Ctrl Pts',(-9.01523625565157,0.93070729426199,26.31510229022));
#33088=CARTESIAN_POINT('Ctrl Pts',(-9.160705053281,0.833754362018685,26.3228202638364));
#33089=CARTESIAN_POINT('Ctrl Pts',(-9.27519220406066,0.708490434988905,
26.3305382374527));
#33090=CARTESIAN_POINT('Ctrl Pts',(-9.38967935484033,0.583226507959125,
26.3382562110691));
#33091=CARTESIAN_POINT('Ctrl Pts',(-9.47318485877022,0.42965158614287,26.3459741846855));
#33092=CARTESIAN_POINT('Ctrl Pts',(-9.51607544515725,0.265457463892782,
26.3536921583018));
#33093=CARTESIAN_POINT('Ctrl Pts',(-9.53867648396682,0.178935967175755,
26.3577591164838));
#33094=CARTESIAN_POINT('Ctrl Pts',(-9.54999987801921,0.0894658107705327,
26.3618260746657));
#33095=CARTESIAN_POINT('Ctrl Pts',(-9.55000808233714,1.77385175400095E-6,
26.3658930328476));
#33096=CARTESIAN_POINT('Ctrl Pts',(-9.55012868473597,-2.18483901666677E-5,
26.2841069671524));
#33097=CARTESIAN_POINT('Ctrl Pts',(-9.54999944986955,0.139451788792166,
26.2777647644543));
#33098=CARTESIAN_POINT('Ctrl Pts',(-9.52201000479389,0.278975766050527,
26.2714225617561));
#33099=CARTESIAN_POINT('Ctrl Pts',(-9.46789831314616,0.407501832957038,
26.265080359058));
#33100=CARTESIAN_POINT('Ctrl Pts',(-9.40204854007008,0.563908185862314,
26.2573623854417));
#33101=CARTESIAN_POINT('Ctrl Pts',(-9.29751427771017,0.704027710451462,
26.2496444118253));
#33102=CARTESIAN_POINT('Ctrl Pts',(-9.16634773368461,0.811705368632605,
26.2419264382089));
#33103=CARTESIAN_POINT('Ctrl Pts',(-9.03518118965904,0.919383026813746,
26.2342084645926));
#33104=CARTESIAN_POINT('Ctrl Pts',(-8.87738236396781,0.994618818586882,
26.2264904909762));
#33105=CARTESIAN_POINT('Ctrl Pts',(-8.7111446128674,1.028738475975,26.2187725173598));
#33106=CARTESIAN_POINT('Ctrl Pts',(-8.54490686176699,1.06285813336311,26.2110545437435));
#33107=CARTESIAN_POINT('Ctrl Pts',(-8.3702301852574,1.05586165636621,26.2033365701271));
#33108=CARTESIAN_POINT('Ctrl Pts',(-8.20725384815146,1.0085556965313,26.1956185965107));
#33109=CARTESIAN_POINT('Ctrl Pts',(-8.04427751104553,0.961249736696391,
26.1879006228944));
#33110=CARTESIAN_POINT('Ctrl Pts',(-7.89300151334325,0.873634294023485,
26.180182649278));
#33111=CARTESIAN_POINT('Ctrl Pts',(-7.77086715620623,0.755810953939201,
26.1724646756617));
#33112=CARTESIAN_POINT('Ctrl Pts',(-7.64873279906922,0.637987613854915,
26.1647467020453));
#33113=CARTESIAN_POINT('Ctrl Pts',(-7.55574008249746,0.489956376359252,
26.1570287284289));
#33114=CARTESIAN_POINT('Ctrl Pts',(-7.50261055937172,0.328784436297264,
26.1493107548126));
#33115=CARTESIAN_POINT('Ctrl Pts',(-7.44948103624598,0.167612496235276,
26.1415927811962));
#33116=CARTESIAN_POINT('Ctrl Pts',(-7.43621470656625,-0.00670014639303557,
26.1338748075799));
#33117=CARTESIAN_POINT('Ctrl Pts',(-7.46434110638773,-0.174056192550768,
26.1261568339635));
#33118=CARTESIAN_POINT('Ctrl Pts',(-7.49246750620921,-0.341412238708501,
26.1184388603471));
#33119=CARTESIAN_POINT('Ctrl Pts',(-7.5619866355319,-0.501811688395654,
26.1107208867308));
#33120=CARTESIAN_POINT('Ctrl Pts',(-7.66488331703068,-0.636761358552236,
26.1030029131144));
#33121=CARTESIAN_POINT('Ctrl Pts',(-7.76777999852946,-0.771711028708818,
26.095284939498));
#33122=CARTESIAN_POINT('Ctrl Pts',(-7.90405423220433,-0.881210919334829,
26.0875669658817));
#33123=CARTESIAN_POINT('Ctrl Pts',(-8.05799434096646,-0.952636289137738,
26.0798489922653));
#33124=CARTESIAN_POINT('Ctrl Pts',(-8.2119344497286,-1.02406165894065,26.072131018649));
#33125=CARTESIAN_POINT('Ctrl Pts',(-8.38354043357801,-1.05741250792046,
26.0644130450326));
#33126=CARTESIAN_POINT('Ctrl Pts',(-8.55302705685301,-1.04884366480909,
26.0566950714162));
#33127=CARTESIAN_POINT('Ctrl Pts',(-8.72251368012801,-1.04027482169772,
26.0489770977999));
#33128=CARTESIAN_POINT('Ctrl Pts',(-8.88988094282861,-0.989786286495173,
26.0412591241835));
#33129=CARTESIAN_POINT('Ctrl Pts',(-9.03583231082944,-0.903199112404309,
26.0335411505671));
#33130=CARTESIAN_POINT('Ctrl Pts',(-9.18178367883027,-0.816611938313444,
26.0258231769508));
#33131=CARTESIAN_POINT('Ctrl Pts',(-9.30631915213132,-0.693926125334262,
26.0181052033344));
#33132=CARTESIAN_POINT('Ctrl Pts',(-9.39508046869405,-0.549286679739332,
26.0103872297181));
#33133=CARTESIAN_POINT('Ctrl Pts',(-9.48384178525678,-0.404647234144403,
26.0026692561017));
#33134=CARTESIAN_POINT('Ctrl Pts',(-9.53682894508118,-0.238054155933727,
25.9949512824853));
#33135=CARTESIAN_POINT('Ctrl Pts',(-9.54793281713632,-0.0687147199931099,
25.987233308869));
#33136=CARTESIAN_POINT('Ctrl Pts',(-9.54943210957357,-0.045849782935783,
25.9861911949634));
#33137=CARTESIAN_POINT('Ctrl Pts',(-9.55016780438665,-0.0229347754959868,
25.9851490810579));
#33138=CARTESIAN_POINT('Ctrl Pts',(-9.55014863741965,-1.85392332084922E-5,
25.9841069671524));
#33139=CARTESIAN_POINT('Origin',(-8.5,0.,25.1));
#33140=CARTESIAN_POINT('',(-9.5501656695242,-1.36966039699926E-5,25.6841069671524));
#33141=CARTESIAN_POINT('',(-9.55003919466624,-1.48519393190782E-5,25.7658930328476));
#33142=CARTESIAN_POINT('',(-9.5501,-1.28600160378464E-16,25.1));
#33143=CARTESIAN_POINT('Ctrl Pts',(-9.55003919466624,-1.48519393190782E-5,
25.7658930328476));
#33144=CARTESIAN_POINT('Ctrl Pts',(-9.55007410770739,-0.0656465986864928,
25.7688767342566));
#33145=CARTESIAN_POINT('Ctrl Pts',(-9.54400992574163,-0.13127197210093,
25.7718604356656));
#33146=CARTESIAN_POINT('Ctrl Pts',(-9.53178263717497,-0.195728209905797,
25.7748441370746));
#33147=CARTESIAN_POINT('Ctrl Pts',(-9.50015417386016,-0.362457877052181,
25.782562110691));
#33148=CARTESIAN_POINT('Ctrl Pts',(-9.42728790559935,-0.521364770823876,
25.7902800843074));
#33149=CARTESIAN_POINT('Ctrl Pts',(-9.32158491639723,-0.654127791549347,
25.7979980579237));
#33150=CARTESIAN_POINT('Ctrl Pts',(-9.21588192719511,-0.786890812274816,
25.8057160315401));
#33151=CARTESIAN_POINT('Ctrl Pts',(-9.07734221705168,-0.89350995995406,
25.8134340051565));
#33152=CARTESIAN_POINT('Ctrl Pts',(-8.92193866025693,-0.9616926273552,25.8211519787728));
#33153=CARTESIAN_POINT('Ctrl Pts',(-8.76653510346219,-1.02987529475634,
25.8288699523892));
#33154=CARTESIAN_POINT('Ctrl Pts',(-8.59426770001613,-1.05962148187937,
25.8365879260055));
#33155=CARTESIAN_POINT('Ctrl Pts',(-8.42499794361343,-1.04750161530483,
25.8443058996219));
#33156=CARTESIAN_POINT('Ctrl Pts',(-8.25572818721072,-1.03538174873029,
25.8520238732383));
#33157=CARTESIAN_POINT('Ctrl Pts',(-8.08945607785137,-0.981395828458169,
25.8597418468546));
#33158=CARTESIAN_POINT('Ctrl Pts',(-7.94535188446413,-0.891768137164413,
25.867459820471));
#33159=CARTESIAN_POINT('Ctrl Pts',(-7.80124769107689,-0.802140445870657,
25.8751777940874));
#33160=CARTESIAN_POINT('Ctrl Pts',(-7.67931141366176,-0.676870983555263,
25.8828957677037));
#33161=CARTESIAN_POINT('Ctrl Pts',(-7.593601641113,-0.530402637186899,25.8906137413201));
#33162=CARTESIAN_POINT('Ctrl Pts',(-7.50789186856424,-0.383934290818535,
25.8983317149364));
#33163=CARTESIAN_POINT('Ctrl Pts',(-7.45840860088185,-0.216267060397201,
25.9060496885528));
#33164=CARTESIAN_POINT('Ctrl Pts',(-7.45085698941586,-0.0467320647085198,
25.9137676621692));
#33165=CARTESIAN_POINT('Ctrl Pts',(-7.44330537794987,0.122802930980162,
25.9214856357855));
#33166=CARTESIAN_POINT('Ctrl Pts',(-7.47768542270028,0.294205691936192,
25.9292036094019));
#33167=CARTESIAN_POINT('Ctrl Pts',(-7.55003329168869,0.447714413024386,
25.9369215830183));
#33168=CARTESIAN_POINT('Ctrl Pts',(-7.62238116067709,0.601223134112577,
25.9446395566346));
#33169=CARTESIAN_POINT('Ctrl Pts',(-7.73269685390349,0.736837815332934,
25.952357530251));
#33170=CARTESIAN_POINT('Ctrl Pts',(-7.8682615725681,0.838922822330773,25.9600755038674));
#33171=CARTESIAN_POINT('Ctrl Pts',(-8.00382629123272,0.941007829328613,
25.9677934774837));
#33172=CARTESIAN_POINT('Ctrl Pts',(-8.16464003533555,1.00956316210393,25.9755114511001));
#33173=CARTESIAN_POINT('Ctrl Pts',(-8.33216185572768,1.03668476398556,25.9832294247164));
#33174=CARTESIAN_POINT('Ctrl Pts',(-8.49968367611981,1.06380636586718,25.9909473983328));
#33175=CARTESIAN_POINT('Ctrl Pts',(-8.67391357280124,1.04949423685511,25.9986653719492));
#33176=CARTESIAN_POINT('Ctrl Pts',(-8.83476378732716,0.995398487625139,
26.0063833455655));
#33177=CARTESIAN_POINT('Ctrl Pts',(-8.99561400185307,0.941302738395167,
26.0141013191819));
#33178=CARTESIAN_POINT('Ctrl Pts',(-9.14308453422347,0.847423368947298,
26.0218192927982));
#33179=CARTESIAN_POINT('Ctrl Pts',(-9.26017283489315,0.724584159174464,
26.0295372664146));
#33180=CARTESIAN_POINT('Ctrl Pts',(-9.37726113556284,0.60174494940163,26.037255240031));
#33181=CARTESIAN_POINT('Ctrl Pts',(-9.4639672045318,0.449945899303832,26.0449732136473));
#33182=CARTESIAN_POINT('Ctrl Pts',(-9.51029430429316,0.286688613470416,
26.0526911872637));
#33183=CARTESIAN_POINT('Ctrl Pts',(-9.53670897597608,0.193602976179322,
26.0570918024583));
#33184=CARTESIAN_POINT('Ctrl Pts',(-9.54999634685876,0.0967922386666701,
26.061492417653));
#33185=CARTESIAN_POINT('Ctrl Pts',(-9.55002929519846,-9.63122723742732E-6,
26.0658930328476));
#33186=CARTESIAN_POINT('Ctrl Pts',(-9.55014863741965,-1.85392332084922E-5,
25.9841069671524));
#33187=CARTESIAN_POINT('Ctrl Pts',(-9.55002585239389,0.146784586201418,
25.9774311074416));
#33188=CARTESIAN_POINT('Ctrl Pts',(-9.51892520411974,0.293638139822104,
25.9707552477307));
#33189=CARTESIAN_POINT('Ctrl Pts',(-9.45914326904298,0.427702105940413,
25.9640793880199));
#33190=CARTESIAN_POINT('Ctrl Pts',(-9.39002926460864,0.582693702262755,
25.9563614144035));
#33191=CARTESIAN_POINT('Ctrl Pts',(-9.28258067145411,0.72059110123688,25.9486434407872));
#33192=CARTESIAN_POINT('Ctrl Pts',(-9.14918572735926,0.825495483554338,
25.9409254671708));
#33193=CARTESIAN_POINT('Ctrl Pts',(-9.01579078326441,0.930399865871797,
25.9332074935544));
#33194=CARTESIAN_POINT('Ctrl Pts',(-8.85644948822923,1.00231123153259,25.9254895199381));
#33195=CARTESIAN_POINT('Ctrl Pts',(-8.6895330260255,1.03293859160238,25.9177715463217));
#33196=CARTESIAN_POINT('Ctrl Pts',(-8.52261656382178,1.06356595167218,25.9100535727053));
#33197=CARTESIAN_POINT('Ctrl Pts',(-8.3481249344495,1.05290930615098,25.902335599089));
#33198=CARTESIAN_POINT('Ctrl Pts',(-8.18617607274301,1.00219730824664,25.8946176254726));
#33199=CARTESIAN_POINT('Ctrl Pts',(-8.02422721103653,0.951485310342298,
25.8868996518563));
#33200=CARTESIAN_POINT('Ctrl Pts',(-7.87482111699583,0.860717960054822,
25.8791816782399));
#33201=CARTESIAN_POINT('Ctrl Pts',(-7.75518349981129,0.740360238682796,
25.8714637046235));
#33202=CARTESIAN_POINT('Ctrl Pts',(-7.63554588262674,0.62000251731077,25.8637457310072));
#33203=CARTESIAN_POINT('Ctrl Pts',(-7.54567674229835,0.470054424854194,
25.8560277573908));
#33204=CARTESIAN_POINT('Ctrl Pts',(-7.49593750140689,0.307804159969934,
25.8483097837744));
#33205=CARTESIAN_POINT('Ctrl Pts',(-7.44619826051544,0.145553895085674,
25.8405918101581));
#33206=CARTESIAN_POINT('Ctrl Pts',(-7.43658891906092,-0.028998542226271,
25.8328738365417));
#33207=CARTESIAN_POINT('Ctrl Pts',(-7.46821738179425,-0.195728206307347,
25.8251558629254));
#33208=CARTESIAN_POINT('Ctrl Pts',(-7.49984584452757,-0.362457870388421,
25.817437889309));
#33209=CARTESIAN_POINT('Ctrl Pts',(-7.57271211144874,-0.521364761238627,
25.8097199156926));
#33210=CARTESIAN_POINT('Ctrl Pts',(-7.67841509870752,-0.654127779523261,
25.8020019420763));
#33211=CARTESIAN_POINT('Ctrl Pts',(-7.7841180859663,-0.786890797807898,
25.7942839684599));
#33212=CARTESIAN_POINT('Ctrl Pts',(-7.92265779356269,-0.893509943526962,
25.7865659948435));
#33213=CARTESIAN_POINT('Ctrl Pts',(-8.07806134750036,-0.961692609674572,
25.7788480212272));
#33214=CARTESIAN_POINT('Ctrl Pts',(-8.23346490143802,-1.02987527582218,
25.7711300476108));
#33215=CARTESIAN_POINT('Ctrl Pts',(-8.40573230171696,-1.05962146239834,
25.7634120739945));
#33216=CARTESIAN_POINT('Ctrl Pts',(-8.57500205500766,-1.04750159604662,
25.7556941003781));
#33217=CARTESIAN_POINT('Ctrl Pts',(-8.74427180829836,-1.0353817296949,25.7479761267617));
#33218=CARTESIAN_POINT('Ctrl Pts',(-8.91054391460082,-0.981395810415311,
25.7402581531454));
#33219=CARTESIAN_POINT('Ctrl Pts',(-9.05464810533871,-0.891768120769351,
25.732540179529));
#33220=CARTESIAN_POINT('Ctrl Pts',(-9.19875229607661,-0.802140431123391,
25.7248222059126));
#33221=CARTESIAN_POINT('Ctrl Pts',(-9.32068857124995,-0.676870971111062,
25.7171042322963));
#33222=CARTESIAN_POINT('Ctrl Pts',(-9.40639834222295,-0.530402627435509,
25.7093862586799));
#33223=CARTESIAN_POINT('Ctrl Pts',(-9.49210811319594,-0.383934283759956,
25.7016682850636));
#33224=CARTESIAN_POINT('Ctrl Pts',(-9.54159137996859,-0.216267056421179,
25.6939503114472));
#33225=CARTESIAN_POINT('Ctrl Pts',(-9.54914299129575,-0.0467320638493777,
25.6862323378308));
#33226=CARTESIAN_POINT('Ctrl Pts',(-9.54983617727468,-0.0311699176136354,
25.685523880938));
#33227=CARTESIAN_POINT('Ctrl Pts',(-9.55017604807986,-0.0155920336305797,
25.6848154240452));
#33228=CARTESIAN_POINT('Ctrl Pts',(-9.5501656695242,-1.36966039699926E-5,
25.6841069671524));
#33229=CARTESIAN_POINT('Origin',(-8.5,0.,25.1));
#33230=CARTESIAN_POINT('',(-9.55017788167088,-7.61182092967605E-6,25.3841069671524));
#33231=CARTESIAN_POINT('',(-9.55005314880761,-1.91003690738122E-5,25.4658930328476));
#33232=CARTESIAN_POINT('',(-9.5501,-1.28600160378464E-16,25.1));
#33233=CARTESIAN_POINT('',(-7.70661869325988,-0.68793612502568,25.2));
#33234=CARTESIAN_POINT('Ctrl Pts',(-9.55017788167088,-7.61182092967605E-6,
25.3841069671524));
#33235=CARTESIAN_POINT('Ctrl Pts',(-9.55011213443803,0.161456744878573,
25.3767637934161));
#33236=CARTESIAN_POINT('Ctrl Pts',(-9.51225375626492,0.322950830145204,
25.3694206196799));
#33237=CARTESIAN_POINT('Ctrl Pts',(-9.44037266037286,0.467529898294161,
25.3620774459436));
#33238=CARTESIAN_POINT('Ctrl Pts',(-9.36482271132683,0.619488366598228,
25.3543594723273));
#33239=CARTESIAN_POINT('Ctrl Pts',(-9.25168833177352,0.752761047051947,
25.3466414987109));
#33240=CARTESIAN_POINT('Ctrl Pts',(-9.11401350383482,0.851981655213685,
25.3389235250945));
#33241=CARTESIAN_POINT('Ctrl Pts',(-8.97633867589611,0.951202263375423,
25.3312055514782));
#33242=CARTESIAN_POINT('Ctrl Pts',(-8.814123399572,1.01637079924518,25.3234875778618));
#33243=CARTESIAN_POINT('Ctrl Pts',(-8.64606983101463,1.03997521165314,25.3157696042454));
#33244=CARTESIAN_POINT('Ctrl Pts',(-8.47801626245725,1.06357962406111,25.3080516306291));
#33245=CARTESIAN_POINT('Ctrl Pts',(-8.30412440166661,1.04561991300728,25.3003336570127));
#33246=CARTESIAN_POINT('Ctrl Pts',(-8.1444440694765,0.988163587521729,25.2926156833963));
#33247=CARTESIAN_POINT('Ctrl Pts',(-7.98476373728639,0.930707262036181,
25.28489770978));
#33248=CARTESIAN_POINT('Ctrl Pts',(-7.83929493369681,0.833754322118917,
25.2771797361636));
#33249=CARTESIAN_POINT('Ctrl Pts',(-7.72480777961413,0.708490392601629,
25.2694617625473));
#33250=CARTESIAN_POINT('Ctrl Pts',(-7.61032062553146,0.583226463084341,
25.2617437889309));
#33251=CARTESIAN_POINT('Ctrl Pts',(-7.5268151209557,0.429651543967029,25.2540258153145));
#33252=CARTESIAN_POINT('Ctrl Pts',(-7.48392451805012,0.265457409338225,
25.2463078416982));
#33253=CARTESIAN_POINT('Ctrl Pts',(-7.44103391514455,0.101263274709422,
25.2385898680818));
#33254=CARTESIAN_POINT('Ctrl Pts',(-7.43875821390916,-0.0735500754308729,
25.2308718944654));
#33255=CARTESIAN_POINT('Ctrl Pts',(-7.47735407353822,-0.238788422518332,
25.2231539208491));
#33256=CARTESIAN_POINT('Ctrl Pts',(-7.51594993316728,-0.404026769605792,
25.2154359472327));
#33257=CARTESIAN_POINT('Ctrl Pts',(-7.59541735366079,-0.559690113640417,
25.2077179736164));
#33258=CARTESIAN_POINT('Ctrl Pts',(-7.70661869325989,-0.687936125025681,
25.2));
#33259=CARTESIAN_POINT('',(-9.29341958724171,-0.687941828405758,25.2));
#33260=CARTESIAN_POINT('Origin',(-8.5,0.,25.2));
#33261=CARTESIAN_POINT('Ctrl Pts',(-9.29341958724171,-0.687941828405758,
25.2));
#33262=CARTESIAN_POINT('Ctrl Pts',(-9.20135889014717,-0.793916350040231,
25.2063833455655));
#33263=CARTESIAN_POINT('Ctrl Pts',(-9.08793206769768,-0.88143161422273,
25.212766691131));
#33264=CARTESIAN_POINT('Ctrl Pts',(-8.96187809424672,-0.943161447318046,
25.2191500366966));
#33265=CARTESIAN_POINT('Ctrl Pts',(-8.8094687923616,-1.01779773612335,25.2268680103129));
#33266=CARTESIAN_POINT('Ctrl Pts',(-8.63860018989813,-1.05473898010619,
25.2345859839293));
#33267=CARTESIAN_POINT('Ctrl Pts',(-8.46897133498624,-1.04972500737682,
25.2423039575456));
#33268=CARTESIAN_POINT('Ctrl Pts',(-8.29934248007435,-1.04471103464745,
25.250021931162));
#33269=CARTESIAN_POINT('Ctrl Pts',(-8.13095337271404,-0.997741845205878,
25.2577399047784));
#33270=CARTESIAN_POINT('Ctrl Pts',(-7.98321890464159,-0.91423316965448,
25.2654578783947));
#33271=CARTESIAN_POINT('Ctrl Pts',(-7.83548443656915,-0.830724494103082,
25.2731758520111));
#33272=CARTESIAN_POINT('Ctrl Pts',(-7.70840460778457,-0.710676332441859,
25.2808938256275));
#33273=CARTESIAN_POINT('Ctrl Pts',(-7.61663078459231,-0.567929370544709,
25.2886117992438));
#33274=CARTESIAN_POINT('Ctrl Pts',(-7.52485696140006,-0.425182408647558,
25.2963297728602));
#33275=CARTESIAN_POINT('Ctrl Pts',(-7.46838914380013,-0.25973664651448,
25.3040477464766));
#33276=CARTESIAN_POINT('Ctrl Pts',(-7.45373787713935,-0.0906671732020418,
25.3117657200929));
#33277=CARTESIAN_POINT('Ctrl Pts',(-7.43908661047857,0.0784023001103964,
25.3194836937093));
#33278=CARTESIAN_POINT('Ctrl Pts',(-7.46625189475693,0.251095484602196,
25.3272016673256));
#33279=CARTESIAN_POINT('Ctrl Pts',(-7.53210166904304,0.407501840417961,
25.334919640942));
#33280=CARTESIAN_POINT('Ctrl Pts',(-7.59795144332914,0.563908196233726,
25.3426376145584));
#33281=CARTESIAN_POINT('Ctrl Pts',(-7.70248570762299,0.704027723373456,
25.3503555881747));
#33282=CARTESIAN_POINT('Ctrl Pts',(-7.83365225406373,0.811705383531112,
25.3580735617911));
#33283=CARTESIAN_POINT('Ctrl Pts',(-7.96481880050447,0.919383043688767,
25.3657915354074));
#33284=CARTESIAN_POINT('Ctrl Pts',(-8.12261762909211,0.994618836864348,
25.3735095090238));
#33285=CARTESIAN_POINT('Ctrl Pts',(-8.28885538324795,1.02873849488606,25.3812274826402));
#33286=CARTESIAN_POINT('Ctrl Pts',(-8.45509313740379,1.06285815290777,25.3889454562565));
#33287=CARTESIAN_POINT('Ctrl Pts',(-8.62976981712784,1.05586167577561,25.3966634298729));
#33288=CARTESIAN_POINT('Ctrl Pts',(-8.79274615723093,1.00855571506968,25.4043814034893));
#33289=CARTESIAN_POINT('Ctrl Pts',(-8.95572249733401,0.961249754363756,
25.4120993771056));
#33290=CARTESIAN_POINT('Ctrl Pts',(-9.10699849781613,0.873634310084068,
25.419817350722));
#33291=CARTESIAN_POINT('Ctrl Pts',(-9.22913285719828,0.755810967834823,
25.4275353243384));
#33292=CARTESIAN_POINT('Ctrl Pts',(-9.35126721658042,0.637987625585578,
25.4352532979547));
#33293=CARTESIAN_POINT('Ctrl Pts',(-9.4442599348626,0.489956385366774,25.4429712715711));
#33294=CARTESIAN_POINT('Ctrl Pts',(-9.49738945896532,0.328784442341286,
25.4506892451874));
#33295=CARTESIAN_POINT('Ctrl Pts',(-9.53227642295773,0.222952518041617,
25.4557571744075));
#33296=CARTESIAN_POINT('Ctrl Pts',(-9.54997533738096,0.111454639072124,
25.4608251036276));
#33297=CARTESIAN_POINT('Ctrl Pts',(-9.55005314880761,-1.91003690738122E-5,
25.4658930328476));
#33298=CARTESIAN_POINT('Origin',(-8.5,0.,24.5374873996035));
#33299=CARTESIAN_POINT('',(-9.71736802727299,-1.11661151494524E-5,26.1625126003965));
#33300=CARTESIAN_POINT('',(-9.71748325610114,-2.53302756962299E-5,26.1874873996035));
#33301=CARTESIAN_POINT('',(-9.71745,-6.10603367124078E-16,24.5374873996035));
#33302=CARTESIAN_POINT('',(-8.18521110449559,1.17604951161383,26.4));
#33303=CARTESIAN_POINT('Ctrl Pts',(-9.71748325610114,-2.53302756962961E-5,
26.1874873996035));
#33304=CARTESIAN_POINT('Ctrl Pts',(-9.71751575780888,-0.0351020206249033,
26.1888631705217));
#33305=CARTESIAN_POINT('Ctrl Pts',(-9.7076841214477,-0.266938209970575,
26.1979569150563));
#33306=CARTESIAN_POINT('Ctrl Pts',(-9.56508058954619,-0.684754074175086,
26.2147686332073));
#33307=CARTESIAN_POINT('Ctrl Pts',(-9.12308458528742,-1.10229325462015,
26.2379225540564));
#33308=CARTESIAN_POINT('Ctrl Pts',(-8.53741089167782,-1.26565666435994,
26.2610764749055));
#33309=CARTESIAN_POINT('Ctrl Pts',(-7.94311327301097,-1.13717141591269,
26.2842303957546));
#33310=CARTESIAN_POINT('Ctrl Pts',(-7.47722213792833,-0.746472111678944,
26.3073843166037));
#33311=CARTESIAN_POINT('Ctrl Pts',(-7.24718515000566,-0.183635660921369,
26.3305382374527));
#33312=CARTESIAN_POINT('Ctrl Pts',(-7.30600772843461,0.421517288496708,
26.3536921583018));
#33313=CARTESIAN_POINT('Ctrl Pts',(-7.64021467375676,0.929507511744114,
26.3768460791509));
#33314=CARTESIAN_POINT('Ctrl Pts',(-7.99510874416174,1.12516550422186,26.3922820263836));
#33315=CARTESIAN_POINT('Ctrl Pts',(-8.1852111044956,1.17604951161383,26.4));
#33316=CARTESIAN_POINT('',(-8.81478889550438,1.17604951161383,26.4));
#33317=CARTESIAN_POINT('Origin',(-8.5,0.,26.4));
#33318=CARTESIAN_POINT('Ctrl Pts',(-9.71736802727299,-1.11661151495218E-5,
26.1625126003965));
#33319=CARTESIAN_POINT('Ctrl Pts',(-9.71739682332927,-0.0846136716837212,
26.1658299588182));
#33320=CARTESIAN_POINT('Ctrl Pts',(-9.68844354006211,-0.366028022972056,
26.1768652908563));
#33321=CARTESIAN_POINT('Ctrl Pts',(-9.47383654720263,-0.809275815695625,
26.1956185965107));
#33322=CARTESIAN_POINT('Ctrl Pts',(-8.98431418402503,-1.16992509177172,
26.2187725173598));
#33323=CARTESIAN_POINT('Ctrl Pts',(-8.38311423523835,-1.26080241069298,
26.2419264382089));
#33324=CARTESIAN_POINT('Ctrl Pts',(-7.80886688894933,-1.06095235748777,
26.265080359058));
#33325=CARTESIAN_POINT('Ctrl Pts',(-7.39398727066922,-0.616458384095017,
26.2882342799071));
#33326=CARTESIAN_POINT('Ctrl Pts',(-7.23414222788049,-0.0298155056950012,
26.3113882007562));
#33327=CARTESIAN_POINT('Ctrl Pts',(-7.36618999782964,0.563701837361564,
26.3345421216053));
#33328=CARTESIAN_POINT('Ctrl Pts',(-7.75968238765149,1.02723719824325,26.3576960424544));
#33329=CARTESIAN_POINT('Ctrl Pts',(-8.2913615143234,1.24083453904628,26.3795153352526));
#33330=CARTESIAN_POINT('Ctrl Pts',(-8.65756915925267,1.21801623774878,26.3936166544345));
#33331=CARTESIAN_POINT('Ctrl Pts',(-8.81482194563459,1.17607986114086,26.4));
#33332=CARTESIAN_POINT('Origin',(-8.5,0.,24.5374873996035));
#33333=CARTESIAN_POINT('',(-9.71737950437713,-1.72188301428289E-5,25.8625126003965));
#33334=CARTESIAN_POINT('',(-9.71750638855972,-2.14937524795297E-5,25.8874873996035));
#33335=CARTESIAN_POINT('',(-9.71745,-6.10603367124078E-16,24.5374873996035));
#33336=CARTESIAN_POINT('Ctrl Pts',(-9.71750638855971,-2.14937524796385E-5,
25.8874873996035));
#33337=CARTESIAN_POINT('Ctrl Pts',(-9.71752861008525,-0.0265897937602074,
25.888529513509));
#33338=CARTESIAN_POINT('Ctrl Pts',(-9.71035873773204,-0.24991293726262,
25.8972896010309));
#33339=CARTESIAN_POINT('Ctrl Pts',(-9.57920099393642,-0.662276467266634,
25.9137676621692));
#33340=CARTESIAN_POINT('Ctrl Pts',(-9.14605449749695,-1.08898966509019,
25.9369215830183));
#33341=CARTESIAN_POINT('Ctrl Pts',(-8.56393486896201,-1.2645937042741,25.9600755038673));
#33342=CARTESIAN_POINT('Ctrl Pts',(-7.96707255574195,-1.14859620568215,
25.9832294247164));
#33343=CARTESIAN_POINT('Ctrl Pts',(-7.49309750825848,-0.767744929110479,
26.0063833455655));
#33344=CARTESIAN_POINT('Ctrl Pts',(-7.25130321058993,-0.209860032372193,
26.0295372664146));
#33345=CARTESIAN_POINT('Ctrl Pts',(-7.29744479634916,0.396416303503929,
26.0526911872637));
#33346=CARTESIAN_POINT('Ctrl Pts',(-7.62088251501485,0.911283354515532,
26.0758451081128));
#33347=CARTESIAN_POINT('Ctrl Pts',(-8.14703515781832,1.21601839122289,26.0989990289619));
#33348=CARTESIAN_POINT('Ctrl Pts',(-8.75457763896279,1.24035281914371,26.122152949811));
#33349=CARTESIAN_POINT('Ctrl Pts',(-9.30341731233995,0.978675413103695,
26.14530687066));
#33350=CARTESIAN_POINT('Ctrl Pts',(-9.64539425734869,0.520283629650974,
26.1670850205909));
#33351=CARTESIAN_POINT('Ctrl Pts',(-9.71733342562011,0.16167563114474,26.1811451969054));
#33352=CARTESIAN_POINT('Ctrl Pts',(-9.71748325610114,-2.53302756962961E-5,
26.1874873996035));
#33353=CARTESIAN_POINT('Ctrl Pts',(-9.71737950437712,-1.72188301428705E-5,
25.8625126003965));
#33354=CARTESIAN_POINT('Ctrl Pts',(-9.71741998136212,-0.0761084197418133,
25.8654963018055));
#33355=CARTESIAN_POINT('Ctrl Pts',(-9.69220323214041,-0.348999073966435,
25.8761979768309));
#33356=CARTESIAN_POINT('Ctrl Pts',(-9.49058720348329,-0.788683685422225,
25.8946176254726));
#33357=CARTESIAN_POINT('Ctrl Pts',(-9.00873260835677,-1.15951545765943,
25.9177715463217));
#33358=CARTESIAN_POINT('Ctrl Pts',(-8.40956981340752,-1.26297559149317,
25.9409254671708));
#33359=CARTESIAN_POINT('Ctrl Pts',(-7.83125923477822,-1.07520730665756,
25.9640793880199));
#33360=CARTESIAN_POINT('Ctrl Pts',(-7.40715299459429,-0.63950792499141,
25.987233308869));
#33361=CARTESIAN_POINT('Ctrl Pts',(-7.2350453736822,-0.056344979529684,
26.0103872297181));
#33362=CARTESIAN_POINT('Ctrl Pts',(-7.35462251532982,0.539810504688725,
26.0335411505671));
#33363=CARTESIAN_POINT('Ctrl Pts',(-7.73831123274286,1.0114915645451,26.0566950714162));
#33364=CARTESIAN_POINT('Ctrl Pts',(-8.29763708577969,1.24993368402129,26.0798489922653));
#33365=CARTESIAN_POINT('Ctrl Pts',(-8.90362562319939,1.20015470640273,26.1030029131144));
#33366=CARTESIAN_POINT('Ctrl Pts',(-9.41654248721522,0.873633122741245,
26.1261568339635));
#33367=CARTESIAN_POINT('Ctrl Pts',(-9.67490713951847,0.421305975808577,
26.1459933963908));
#33368=CARTESIAN_POINT('Ctrl Pts',(-9.7173298280956,0.112217608765634,26.1581119852019));
#33369=CARTESIAN_POINT('Ctrl Pts',(-9.71736802727299,-1.11661151495218E-5,
26.1625126003965));
#33370=CARTESIAN_POINT('Origin',(-8.5,0.,24.5374873996035));
#33371=CARTESIAN_POINT('',(-9.71739568233103,-2.21443141968369E-5,25.5625126003965));
#33372=CARTESIAN_POINT('',(-9.7175261349988,-1.58793738679787E-5,25.5874873996035));
#33373=CARTESIAN_POINT('',(-9.71745,-6.10603367124078E-16,24.5374873996035));
#33374=CARTESIAN_POINT('Ctrl Pts',(-9.7175261349988,-1.58793738680163E-5,
25.5874873996035));
#33375=CARTESIAN_POINT('Ctrl Pts',(-9.71753816754102,-0.0180768701490775,
25.5881958564963));
#33376=CARTESIAN_POINT('Ctrl Pts',(-9.71285149565645,-0.232889174626129,
25.5966222870055));
#33377=CARTESIAN_POINT('Ctrl Pts',(-9.59284698531382,-0.639507913234122,
25.612766691131));
#33378=CARTESIAN_POINT('Ctrl Pts',(-9.16874075292704,-1.07520728689,25.6359206119801));
#33379=CARTESIAN_POINT('Ctrl Pts',(-8.59043018492992,-1.26297556827349,
25.6590745328292));
#33380=CARTESIAN_POINT('Ctrl Pts',(-7.99126740099621,-1.15951543634185,
25.6822284536783));
#33381=CARTESIAN_POINT('Ctrl Pts',(-7.50941281472855,-0.788683670922342,
25.7053823745274));
#33382=CARTESIAN_POINT('Ctrl Pts',(-7.25597684673547,-0.235990039080846,
25.7285362953765));
#33383=CARTESIAN_POINT('Ctrl Pts',(-7.28939907153445,0.371120326042741,
25.7516902162256));
#33384=CARTESIAN_POINT('Ctrl Pts',(-7.60197268802659,0.892654385164513,
25.7748441370747));
#33385=CARTESIAN_POINT('Ctrl Pts',(-8.12162162390845,1.2083520633118,25.7979980579237));
#33386=CARTESIAN_POINT('Ctrl Pts',(-8.7285204930998,1.2454169135826,25.8211519787728));
#33387=CARTESIAN_POINT('Ctrl Pts',(-9.2827250249746,0.995302185107979,25.8443058996219));
#33388=CARTESIAN_POINT('Ctrl Pts',(-9.63962141358243,0.537268419868294,
25.8664177065655));
#33389=CARTESIAN_POINT('Ctrl Pts',(-9.7173640358032,0.170177025493677,25.8808115398927));
#33390=CARTESIAN_POINT('Ctrl Pts',(-9.71750638855971,-2.14937524796385E-5,
25.8874873996035));
#33391=CARTESIAN_POINT('Ctrl Pts',(-9.71739568233103,-2.2144314196941E-5,
25.5625126003965));
#33392=CARTESIAN_POINT('Ctrl Pts',(-9.71744285456702,-0.0676017501666064,
25.5651626447928));
#33393=CARTESIAN_POINT('Ctrl Pts',(-9.69577288570607,-0.331969861171505,
25.5755306628055));
#33394=CARTESIAN_POINT('Ctrl Pts',(-9.50690251025353,-0.767744943225855,
25.5936166544345));
#33395=CARTESIAN_POINT('Ctrl Pts',(-9.03292745405576,-1.14859622679878,
25.6167705752836));
#33396=CARTESIAN_POINT('Ctrl Pts',(-8.4360651298626,-1.26459372752363,25.6399244961327));
#33397=CARTESIAN_POINT('Ctrl Pts',(-7.85394549062537,-1.08898968511111,
25.6630784169818));
#33398=CARTESIAN_POINT('Ctrl Pts',(-7.42079898622258,-0.662276479442534,
25.6862323378308));
#33399=CARTESIAN_POINT('Ctrl Pts',(-7.23650448403929,-0.0828495292575919,
25.7093862586799));
#33400=CARTESIAN_POINT('Ctrl Pts',(-7.34355828943908,0.515681620221391,
25.732540179529));
#33401=CARTESIAN_POINT('Ctrl Pts',(-7.71727496063508,0.995302203406518,
25.7556941003781));
#33402=CARTESIAN_POINT('Ctrl Pts',(-8.27147950269888,1.24541693647946,25.7788480212272));
#33403=CARTESIAN_POINT('Ctrl Pts',(-8.878378383048,1.20835208552723,25.8020019420763));
#33404=CARTESIAN_POINT('Ctrl Pts',(-9.39802732848356,0.892654401575867,
25.8251558629253));
#33405=CARTESIAN_POINT('Ctrl Pts',(-9.67032153700355,0.43832717639768,25.8453260823654));
#33406=CARTESIAN_POINT('Ctrl Pts',(-9.71731527909489,0.120717535865137,
25.8577783281891));
#33407=CARTESIAN_POINT('Ctrl Pts',(-9.71737950437712,-1.72188301428705E-5,
25.8625126003965));
#33408=CARTESIAN_POINT('Origin',(-8.5,0.,24.5374873996035));
#33409=CARTESIAN_POINT('',(-9.71741565872953,-3.18308007817847E-5,25.2625126003965));
#33410=CARTESIAN_POINT('',(-9.7175402933437,-8.82488467109868E-6,25.2874873996035));
#33411=CARTESIAN_POINT('',(-9.71745,-6.10603367124078E-16,24.5374873996035));
#33412=CARTESIAN_POINT('',(-8.81478889550441,1.17604951161383,25.2));
#33413=CARTESIAN_POINT('Ctrl Pts',(-8.8147888955044,1.17604951161383,25.2));
#33414=CARTESIAN_POINT('Ctrl Pts',(-9.00489125583826,1.12516550422186,25.2077179736164));
#33415=CARTESIAN_POINT('Ctrl Pts',(-9.35978529202387,0.929507318017654,
25.2231539208491));
#33416=CARTESIAN_POINT('Ctrl Pts',(-9.66055721233611,0.472338081655336,
25.2439914543146));
#33417=CARTESIAN_POINT('Ctrl Pts',(-9.71730344186206,0.137705854269909,
25.2571110141637));
#33418=CARTESIAN_POINT('Ctrl Pts',(-9.71741565872953,-3.18308007818402E-5,
25.2625126003965));
#33419=CARTESIAN_POINT('',(-8.18517804880579,1.17607982959759,25.2));
#33420=CARTESIAN_POINT('Origin',(-8.5,0.,25.2));
#33421=CARTESIAN_POINT('Ctrl Pts',(-8.18517804880579,1.17607982959759,25.2));
#33422=CARTESIAN_POINT('Ctrl Pts',(-8.3424308355762,1.21801620838825,25.2063833455655));
#33423=CARTESIAN_POINT('Ctrl Pts',(-8.70863847539721,1.24083450908453,25.2204846647474));
#33424=CARTESIAN_POINT('Ctrl Pts',(-9.24031759749596,1.02723717888941,25.2423039575457));
#33425=CARTESIAN_POINT('Ctrl Pts',(-9.62744039394288,0.571205219807404,
25.2650830785146));
#33426=CARTESIAN_POINT('Ctrl Pts',(-9.71746406825214,0.187187424104769,
25.2801442258672));
#33427=CARTESIAN_POINT('Ctrl Pts',(-9.71754029334369,-8.82488467114119E-6,
25.2874873996035));
#33428=CARTESIAN_POINT('Origin',(-8.5,0.,24.5374873996035));
#33429=CARTESIAN_POINT('Ctrl Pts',(-9.71754029334369,-8.82488467114119E-6,
25.2874873996035));
#33430=CARTESIAN_POINT('Ctrl Pts',(-9.71754418391693,-0.00956343086266385,
25.2878621994836));
#33431=CARTESIAN_POINT('Ctrl Pts',(-9.71516353125157,-0.215866953049769,
25.2959549729801));
#33432=CARTESIAN_POINT('Ctrl Pts',(-9.60601270884069,-0.616458373015401,
25.3117657200929));
#33433=CARTESIAN_POINT('Ctrl Pts',(-9.19113309833576,-1.06095233793524,
25.334919640942));
#33434=CARTESIAN_POINT('Ctrl Pts',(-8.61688576258933,-1.26080238756323,
25.3580735617911));
#33435=CARTESIAN_POINT('Ctrl Pts',(-8.01568582487961,-1.16992507024812,
25.3812274826402));
#33436=CARTESIAN_POINT('Ctrl Pts',(-7.52616347069768,-0.809275800827533,
25.4043814034893));
#33437=CARTESIAN_POINT('Ctrl Pts',(-7.26119721213712,-0.262016330420185,
25.4275353243383));
#33438=CARTESIAN_POINT('Ctrl Pts',(-7.28188538871804,0.345661246443408,
25.4506892451874));
#33439=CARTESIAN_POINT('Ctrl Pts',(-7.58345752963543,0.873633106680533,
25.4738431660365));
#33440=CARTESIAN_POINT('Ctrl Pts',(-8.09637438422115,1.20015468433752,25.4969970868856));
#33441=CARTESIAN_POINT('Ctrl Pts',(-8.70236291049992,1.2499336610416,25.5201510077347));
#33442=CARTESIAN_POINT('Ctrl Pts',(-9.26168875325356,1.01149154594881,25.5433049285838));
#33443=CARTESIAN_POINT('Ctrl Pts',(-9.63363746876147,0.554242853504049,
25.56575039254));
#33444=CARTESIAN_POINT('Ctrl Pts',(-9.71740708427495,0.178680690828068,
25.58047788288));
#33445=CARTESIAN_POINT('Ctrl Pts',(-9.7175261349988,-1.58793738680163E-5,
25.5874873996035));
#33446=CARTESIAN_POINT('Ctrl Pts',(-9.71741565872953,-3.18308007818402E-5,
25.2625126003965));
#33447=CARTESIAN_POINT('Ctrl Pts',(-9.71746378121149,-0.0590985238410443,
25.2648289877801));
#33448=CARTESIAN_POINT('Ctrl Pts',(-9.6991494544252,-0.314940022053408,
25.27486334878));
#33449=CARTESIAN_POINT('Ctrl Pts',(-9.52277787696657,-0.746472135969,25.2926156833964));
#33450=CARTESIAN_POINT('Ctrl Pts',(-9.05688673586305,-1.13717144686837,
25.3157696042454));
#33451=CARTESIAN_POINT('Ctrl Pts',(-8.46258910686823,-1.26565668871267,
25.3389235250945));
#33452=CARTESIAN_POINT('Ctrl Pts',(-7.87691540315674,-1.10229327660247,
25.3620774459436));
#33453=CARTESIAN_POINT('Ctrl Pts',(-7.43491939071853,-0.684754086769719,
25.3852313667927));
#33454=CARTESIAN_POINT('Ctrl Pts',(-7.23851882542848,-0.109317624216872,
25.4083852876418));
#33455=CARTESIAN_POINT('Ctrl Pts',(-7.3330023279845,0.49132607864821,25.4315392084909));
#33456=CARTESIAN_POINT('Ctrl Pts',(-7.69658267289797,0.978675431042071,
25.45469312934));
#33457=CARTESIAN_POINT('Ctrl Pts',(-8.24542235634912,1.24035284195992,25.477847050189));
#33458=CARTESIAN_POINT('Ctrl Pts',(-8.85296484867377,1.21601841356867,25.5010009710381));
#33459=CARTESIAN_POINT('Ctrl Pts',(-9.37911750114581,0.911283371272776,
25.5241548918872));
#33460=CARTESIAN_POINT('Ctrl Pts',(-9.66553668642746,0.455344583774923,
25.54465876834));
#33461=CARTESIAN_POINT('Ctrl Pts',(-9.7173054704261,0.129216693970434,25.5574446711764));
#33462=CARTESIAN_POINT('Ctrl Pts',(-9.71739568233103,-2.2144314196941E-5,
25.5625126003965));
#33463=CARTESIAN_POINT('Ctrl Pts',(-7.70661869325989,-0.687936125025681,
25.2));
#33464=CARTESIAN_POINT('Ctrl Pts',(-7.59541735366079,-0.559690113640417,
25.2077179736164));
#33465=CARTESIAN_POINT('Ctrl Pts',(-7.43648251267377,-0.248363425571168,
25.2231539208491));
#33466=CARTESIAN_POINT('Ctrl Pts',(-7.44330961637993,0.276076624849719,
25.2463078416982));
#33467=CARTESIAN_POINT('Ctrl Pts',(-7.69382613010723,0.736801382201653,
25.2694617625473));
#33468=CARTESIAN_POINT('Ctrl Pts',(-8.13023254087597,1.02766020195344,25.2926156833963));
#33469=CARTESIAN_POINT('Ctrl Pts',(-8.65190812324789,1.08153933511494,25.3157696042454));
#33470=CARTESIAN_POINT('Ctrl Pts',(-9.13855395222022,0.886033727505665,
25.3389235250945));
#33471=CARTESIAN_POINT('Ctrl Pts',(-9.47795709088013,0.48621568614451,25.3620774459436));
#33472=CARTESIAN_POINT('Ctrl Pts',(-9.59185364649637,-0.0257170823187401,
25.3852313667927));
#33473=CARTESIAN_POINT('Ctrl Pts',(-9.45398081691536,-0.53172034786108,
25.4083852876418));
#33474=CARTESIAN_POINT('Ctrl Pts',(-9.09613032696405,-0.915114419537387,
25.4315392084909));
#33475=CARTESIAN_POINT('Ctrl Pts',(-8.60081871066168,-1.0874931924762,25.45469312934));
#33476=CARTESIAN_POINT('Ctrl Pts',(-8.08225938207407,-1.00910782066413,
25.4778470501891));
#33477=CARTESIAN_POINT('Ctrl Pts',(-7.66002649848424,-0.698033199268136,
25.5010009710381));
#33478=CARTESIAN_POINT('Ctrl Pts',(-7.43148235448289,-0.225999711342754,
25.5241548918872));
#33479=CARTESIAN_POINT('Ctrl Pts',(-7.44932674581528,0.298146843722718,
25.5473088127363));
#33480=CARTESIAN_POINT('Ctrl Pts',(-7.7094449479405,0.753543985646414,25.5704627335854));
#33481=CARTESIAN_POINT('Ctrl Pts',(-8.15185653691784,1.0351820888109,25.5936166544345));
#33482=CARTESIAN_POINT('Ctrl Pts',(-8.67454621735263,1.07811847505834,25.6167705752836));
#33483=CARTESIAN_POINT('Ctrl Pts',(-9.15698744079146,0.872452480513238,
25.6399244961327));
#33484=CARTESIAN_POINT('Ctrl Pts',(-9.48793451438624,0.465608444332083,
25.6630784169817));
#33485=CARTESIAN_POINT('Ctrl Pts',(-9.59107464674124,-0.048599829082402,
25.6862323378308));
#33486=CARTESIAN_POINT('Ctrl Pts',(-9.44262484642329,-0.551601511098732,
25.7093862586799));
#33487=CARTESIAN_POINT('Ctrl Pts',(-9.07681602090327,-0.927409891135722,
25.732540179529));
#33488=CARTESIAN_POINT('Ctrl Pts',(-8.5779997019959,-1.08936764897449,25.7556941003781));
#33489=CARTESIAN_POINT('Ctrl Pts',(-8.06119750115908,-1.00012908924603,
25.7788480212272));
#33490=CARTESIAN_POINT('Ctrl Pts',(-7.64557837836991,-0.680271652088834,
25.8020019420763));
#33491=CARTESIAN_POINT('Ctrl Pts',(-7.4269795776064,-0.203550979538212,
25.8251558629254));
#33492=CARTESIAN_POINT('Ctrl Pts',(-7.45580760196995,0.32010633239762,25.8483097837744));
#33493=CARTESIAN_POINT('Ctrl Pts',(-7.72541502295513,0.769950609767346,
25.8714637046235));
#33494=CARTESIAN_POINT('Ctrl Pts',(-8.17363330507722,1.04225266062977,25.8946176254726));
#33495=CARTESIAN_POINT('Ctrl Pts',(-8.69710819319406,1.07422259719338,25.9177715463217));
#33496=CARTESIAN_POINT('Ctrl Pts',(-9.17513207829958,0.858488500211005,
25.9409254671708));
#33497=CARTESIAN_POINT('Ctrl Pts',(-9.49747785776318,0.444796303288628,
25.9640793880199));
#33498=CARTESIAN_POINT('Ctrl Pts',(-9.58981610490559,-0.0714610777230468,
25.987233308869));
#33499=CARTESIAN_POINT('Ctrl Pts',(-9.43085462543237,-0.57124031235508,
26.0103872297181));
#33500=CARTESIAN_POINT('Ctrl Pts',(-9.05724820552922,-0.939297751292626,
26.0335411505671));
#33501=CARTESIAN_POINT('Ctrl Pts',(-8.55514641742741,-1.09076335690027,
26.0566950714162));
#33502=CARTESIAN_POINT('Ctrl Pts',(-8.04032846587919,-0.990710809960839,
26.0798489922653));
#33503=CARTESIAN_POINT('Ctrl Pts',(-7.6315057648546,-0.662211138082807,
26.1030029131144));
#33504=CARTESIAN_POINT('Ctrl Pts',(-7.42294837688651,-0.181012789021348,
26.1261568339635));
#33505=CARTESIAN_POINT('Ctrl Pts',(-7.46274736592571,0.341925138863589,
26.1493107548126));
#33506=CARTESIAN_POINT('Ctrl Pts',(-7.74172551564097,0.786018851350577,
26.1724646756617));
#33507=CARTESIAN_POINT('Ctrl Pts',(-8.19555350874781,1.0488651793693,26.1956185965107));
#33508=CARTESIAN_POINT('Ctrl Pts',(-8.71958353827659,1.06985461036002,26.2187725173598));
#33509=CARTESIAN_POINT('Ctrl Pts',(-9.19298001535027,0.844147235040609,
26.2419264382089));
#33510=CARTESIAN_POINT('Ctrl Pts',(-9.50658280242999,0.423788661273173,
26.265080359058));
#33511=CARTESIAN_POINT('Ctrl Pts',(-9.58807865380676,-0.0942908823910285,
26.2882342799071));
#33512=CARTESIAN_POINT('Ctrl Pts',(-9.41867520397754,-0.590628159917251,
26.3113882007562));
#33513=CARTESIAN_POINT('Ctrl Pts',(-9.03743572467889,-0.95077263680366,
26.3345421216053));
#33514=CARTESIAN_POINT('Ctrl Pts',(-8.53226841131125,-1.0916802030838,26.3576960424544));
#33515=CARTESIAN_POINT('Ctrl Pts',(-8.01966261282913,-0.980856465439986,
26.3808499633034));
#33516=CARTESIAN_POINT('Ctrl Pts',(-7.61781261410204,-0.643862470306016,
26.4040038841525));
#33517=CARTESIAN_POINT('Ctrl Pts',(-7.41939638262019,-0.158393205087297,
26.4271578050016));
#33518=CARTESIAN_POINT('Ctrl Pts',(-7.47013324212837,0.363575756417424,
26.4503117258507));
#33519=CARTESIAN_POINT('Ctrl Pts',(-7.75840028659244,0.801737926060614,
26.4734656466998));
#33520=CARTESIAN_POINT('Ctrl Pts',(-8.06451081542917,0.970500879693931,
26.4889015939325));
#33521=CARTESIAN_POINT('Ctrl Pts',(-8.22848181102372,1.01439039972539,26.4966195675489));
#33522=CARTESIAN_POINT('Ctrl Pts',(-7.66447275106931,-0.72448061619257,
25.1677934774837));
#33523=CARTESIAN_POINT('Ctrl Pts',(-7.5473641822597,-0.58942192982228,25.1755114511001));
#33524=CARTESIAN_POINT('Ctrl Pts',(-7.3799864165864,-0.261556968811283,
25.1909473983328));
#33525=CARTESIAN_POINT('Ctrl Pts',(-7.3871761891829,0.290742346580538,25.2141013191819));
#33526=CARTESIAN_POINT('Ctrl Pts',(-7.65100062233763,0.77594168989027,25.237255240031));
#33527=CARTESIAN_POINT('Ctrl Pts',(-8.11058978168339,1.08225149002027,25.2604091608801));
#33528=CARTESIAN_POINT('Ctrl Pts',(-8.65997777516216,1.13899278644703,25.2835630817291));
#33529=CARTESIAN_POINT('Ctrl Pts',(-9.17247516731213,0.933101544633581,
25.3067170025782));
#33530=CARTESIAN_POINT('Ctrl Pts',(-9.52990805401342,0.512044399307156,
25.3298709234273));
#33531=CARTESIAN_POINT('Ctrl Pts',(-9.64985501390302,-0.0270832232342217,
25.3530248442764));
#33532=CARTESIAN_POINT('Ctrl Pts',(-9.5046581142238,-0.559966356245853,
25.3761787651255));
#33533=CARTESIAN_POINT('Ctrl Pts',(-9.12779791742128,-0.963727059003338,
25.3993326859746));
#33534=CARTESIAN_POINT('Ctrl Pts',(-8.60617439463756,-1.14526292417188,
25.4224866068237));
#33535=CARTESIAN_POINT('Ctrl Pts',(-8.06006819634258,-1.06271357052546,
25.4456405276728));
#33536=CARTESIAN_POINT('Ctrl Pts',(-7.61540548922205,-0.735114066454602,
25.4687944485218));
#33537=CARTESIAN_POINT('Ctrl Pts',(-7.37472064036763,-0.238005251035231,
25.4919483693709));
#33538=CARTESIAN_POINT('Ctrl Pts',(-7.3935129601162,0.313984977962948,25.51510229022));
#33539=CARTESIAN_POINT('Ctrl Pts',(-7.66744914183881,0.793573692657787,
25.5382562110691));
#33540=CARTESIAN_POINT('Ctrl Pts',(-8.13336248601895,1.09017295398644,25.5614101319182));
#33541=CARTESIAN_POINT('Ctrl Pts',(-8.68381844840173,1.13539020371943,25.5845640527673));
#33542=CARTESIAN_POINT('Ctrl Pts',(-9.19188787827883,0.918798835658428,
25.6077179736164));
#33543=CARTESIAN_POINT('Ctrl Pts',(-9.54041549746167,0.490342461142855,
25.6308718944655));
#33544=CARTESIAN_POINT('Ctrl Pts',(-9.6490346321814,-0.0511815455528781,
25.6540258153145));
#33545=CARTESIAN_POINT('Ctrl Pts',(-9.49269889272013,-0.580903645143862,
25.6771797361636));
#33546=CARTESIAN_POINT('Ctrl Pts',(-9.10745759824453,-0.97667568972048,
25.7003336570127));
#33547=CARTESIAN_POINT('Ctrl Pts',(-8.58214319630724,-1.14723695540749,
25.7234875778618));
#33548=CARTESIAN_POINT('Ctrl Pts',(-8.03788746777146,-1.0532578716113,25.7466414987109));
#33549=CARTESIAN_POINT('Ctrl Pts',(-7.60018985715613,-0.716408991700003,
25.76979541956));
#33550=CARTESIAN_POINT('Ctrl Pts',(-7.36997866731609,-0.214363999385756,
25.7929493404091));
#33551=CARTESIAN_POINT('Ctrl Pts',(-7.40033809182479,0.337110996945993,
25.8161032612581));
#33552=CARTESIAN_POINT('Ctrl Pts',(-7.68426757797895,0.810851868233069,
25.8392571821072));
#33553=CARTESIAN_POINT('Ctrl Pts',(-8.15629607802097,1.09761912819045,25.8624111029563));
#33554=CARTESIAN_POINT('Ctrl Pts',(-8.7075789598293,1.13128736932312,25.8855650238054));
#33555=CARTESIAN_POINT('Ctrl Pts',(-9.21099639385792,0.904093061843329,
25.9087189446545));
#33556=CARTESIAN_POINT('Ctrl Pts',(-9.55046580160874,0.468424739105964,
25.9318728655036));
#33557=CARTESIAN_POINT('Ctrl Pts',(-9.64770923418088,-0.0752572277268409,
25.9550267863527));
#33558=CARTESIAN_POINT('Ctrl Pts',(-9.48030341493372,-0.601585697325598,
25.9781807072018));
#33559=CARTESIAN_POINT('Ctrl Pts',(-9.08685030285179,-0.989195055891815,
26.0013346280508));
#33560=CARTESIAN_POINT('Ctrl Pts',(-8.55807590127228,-1.14870680602488,
26.0244885488999));
#33561=CARTESIAN_POINT('Ctrl Pts',(-8.01590982916678,-1.04333927520127,
26.047642469749));
#33562=CARTESIAN_POINT('Ctrl Pts',(-7.58536967932256,-0.697389068425364,
26.0707963905981));
#33563=CARTESIAN_POINT('Ctrl Pts',(-7.36573332145432,-0.190628536804963,
26.0939503114472));
#33564=CARTESIAN_POINT('Ctrl Pts',(-7.40764650940019,0.360088860410369,
26.1171042322963));
#33565=CARTESIAN_POINT('Ctrl Pts',(-7.70144451543227,0.827773685738895,
26.1402581531454));
#33566=CARTESIAN_POINT('Ctrl Pts',(-8.17938072510464,1.10458291665383,26.1634120739944));
#33567=CARTESIAN_POINT('Ctrl Pts',(-8.73124823850532,1.12668734662125,26.1865659948435));
#33568=CARTESIAN_POINT('Ctrl Pts',(-9.22979244768016,0.888989961061638,
26.2097199156926));
#33569=CARTESIAN_POINT('Ctrl Pts',(-9.56005441846232,0.44630113070912,26.2328738365417));
#33570=CARTESIAN_POINT('Ctrl Pts',(-9.64587948633527,-0.0992997955637866,
26.2560277573908));
#33571=CARTESIAN_POINT('Ctrl Pts',(-9.46747699916709,-0.622003464669862,
26.2791816782399));
#33572=CARTESIAN_POINT('Ctrl Pts',(-9.06598534488173,-1.00127950940916,
26.302335599089));
#33573=CARTESIAN_POINT('Ctrl Pts',(-8.53398257143344,-1.14967235684252,
26.3254895199381));
#33574=CARTESIAN_POINT('Ctrl Pts',(-7.99414616622307,-1.03296144893089,
26.3486434407871));
#33575=CARTESIAN_POINT('Ctrl Pts',(-7.57094912204414,-0.678065684096992,
26.3717973616362));
#33576=CARTESIAN_POINT('Ctrl Pts',(-7.36199263841535,-0.166807357031988,
26.3949512824853));
#33577=CARTESIAN_POINT('Ctrl Pts',(-7.41542473756378,0.382889600443852,
26.4181052033344));
#33578=CARTESIAN_POINT('Ctrl Pts',(-7.71900508231388,0.844327787955114,
26.4412591241835));
#33579=CARTESIAN_POINT('Ctrl Pts',(-8.04137679167336,1.02205575453657,26.4566950714162));
#33580=CARTESIAN_POINT('Ctrl Pts',(-8.21405824218102,1.06827677035487,26.4644130450326));
#33581=CARTESIAN_POINT('Ctrl Pts',(-7.62232680887874,-0.761025107359458,
25.1355869549674));
#33582=CARTESIAN_POINT('Ctrl Pts',(-7.49931101085861,-0.619153746004144,
25.1433049285838));
#33583=CARTESIAN_POINT('Ctrl Pts',(-7.32349032049903,-0.274750512051398,
25.1587408758165));
#33584=CARTESIAN_POINT('Ctrl Pts',(-7.33104276198587,0.305408068311358,
25.1818947966656));
#33585=CARTESIAN_POINT('Ctrl Pts',(-7.60817511456803,0.815081997578886,
25.2050487175147));
#33586=CARTESIAN_POINT('Ctrl Pts',(-8.0909470224908,1.13684277808709,25.2282026383638));
#33587=CARTESIAN_POINT('Ctrl Pts',(-8.66804742707643,1.19644623777912,25.2513565592129));
#33588=CARTESIAN_POINT('Ctrl Pts',(-9.20639638240405,0.980169361761496,
25.2745104800619));
#33589=CARTESIAN_POINT('Ctrl Pts',(-9.5818590171467,0.537873112469803,25.297664400911));
#33590=CARTESIAN_POINT('Ctrl Pts',(-9.70785638130967,-0.0284493641497029,
25.3208183217601));
#33591=CARTESIAN_POINT('Ctrl Pts',(-9.55533541153225,-0.588212364630628,
25.3439722426092));
#33592=CARTESIAN_POINT('Ctrl Pts',(-9.15946550787852,-1.01233969846929,
25.3671261634583));
#33593=CARTESIAN_POINT('Ctrl Pts',(-8.61153007861345,-1.20303265586756,
25.3902800843074));
#33594=CARTESIAN_POINT('Ctrl Pts',(-8.03787701061109,-1.11631932038679,
25.4134340051565));
#33595=CARTESIAN_POINT('Ctrl Pts',(-7.57078447995986,-0.772194933641068,
25.4365879260056));
#33596=CARTESIAN_POINT('Ctrl Pts',(-7.31795892625238,-0.250010790727708,
25.4597418468546));
#33597=CARTESIAN_POINT('Ctrl Pts',(-7.33769917441712,0.329823112203178,
25.4828957677037));
#33598=CARTESIAN_POINT('Ctrl Pts',(-7.62545333573712,0.833603399669161,
25.5060496885528));
#33599=CARTESIAN_POINT('Ctrl Pts',(-8.11486843512004,1.14516381916198,25.5292036094019));
#33600=CARTESIAN_POINT('Ctrl Pts',(-8.69309067945083,1.19266193238051,25.552357530251));
#33601=CARTESIAN_POINT('Ctrl Pts',(-9.22678831576619,0.965145190803617,
25.5755114511001));
#33602=CARTESIAN_POINT('Ctrl Pts',(-9.59289648053711,0.515076477953626,
25.5986653719492));
#33603=CARTESIAN_POINT('Ctrl Pts',(-9.70699461762157,-0.0537632620233534,
25.6218192927982));
#33604=CARTESIAN_POINT('Ctrl Pts',(-9.54277293901697,-0.610205779188992,
25.6449732136473));
#33605=CARTESIAN_POINT('Ctrl Pts',(-9.13809917558578,-1.02594148830524,
25.6681271344964));
#33606=CARTESIAN_POINT('Ctrl Pts',(-8.58628669061858,-1.20510626184049,
25.6912810553455));
#33607=CARTESIAN_POINT('Ctrl Pts',(-8.01457743438384,-1.10638665397658,
25.7144349761946));
#33608=CARTESIAN_POINT('Ctrl Pts',(-7.55480133594234,-0.752546331311173,
25.7375888970437));
#33609=CARTESIAN_POINT('Ctrl Pts',(-7.31297775702578,-0.225177019233301,
25.7607428178928));
#33610=CARTESIAN_POINT('Ctrl Pts',(-7.34486858167961,0.354115661494367,
25.7838967387419));
#33611=CARTESIAN_POINT('Ctrl Pts',(-7.64312013300277,0.851753126698791,
25.8070506595909));
#33612=CARTESIAN_POINT('Ctrl Pts',(-8.13895885096471,1.15298559575112,25.83020458044));
#33613=CARTESIAN_POINT('Ctrl Pts',(-8.71804972646455,1.18835214145286,25.8533585012891));
#33614=CARTESIAN_POINT('Ctrl Pts',(-9.24686070941626,0.949697623475654,
25.8765124221382));
#33615=CARTESIAN_POINT('Ctrl Pts',(-9.6034537454543,0.4920531749233,25.8996663429873));
#33616=CARTESIAN_POINT('Ctrl Pts',(-9.70560236345618,-0.0790533777306346,
25.9228202638364));
#33617=CARTESIAN_POINT('Ctrl Pts',(-9.52975220443507,-0.631931082296116,
25.9459741846855));
#33618=CARTESIAN_POINT('Ctrl Pts',(-9.11645240017437,-1.039092360491,25.9691281055346));
#33619=CARTESIAN_POINT('Ctrl Pts',(-8.56100538511715,-1.20665025514949,
25.9922820263836));
#33620=CARTESIAN_POINT('Ctrl Pts',(-7.99149119245436,-1.09596774044171,
26.0154359472327));
#33621=CARTESIAN_POINT('Ctrl Pts',(-7.53923359379052,-0.732566998767922,
26.0385898680818));
#33622=CARTESIAN_POINT('Ctrl Pts',(-7.30851826602212,-0.200244284588578,
26.0617437889309));
#33623=CARTESIAN_POINT('Ctrl Pts',(-7.35254565287468,0.378252581957149,
26.08489770978));
#33624=CARTESIAN_POINT('Ctrl Pts',(-7.66116351522356,0.869528520127214,
26.1080516306291));
#33625=CARTESIAN_POINT('Ctrl Pts',(-8.16320794146148,1.16030065393836,26.1312055514782));
#33626=CARTESIAN_POINT('Ctrl Pts',(-8.74291293873406,1.18352008288248,26.1543594723273));
#33627=CARTESIAN_POINT('Ctrl Pts',(-9.26660488001006,0.933832687082666,
26.1775133931763));
#33628=CARTESIAN_POINT('Ctrl Pts',(-9.61352603449465,0.468813600145068,
26.2006673140254));
#33629=CARTESIAN_POINT('Ctrl Pts',(-9.70368031886378,-0.104308708736543,
26.2238212348745));
#33630=CARTESIAN_POINT('Ctrl Pts',(-9.51627879435664,-0.653378769422475,
26.2469751557236));
#33631=CARTESIAN_POINT('Ctrl Pts',(-9.09453496508457,-1.05178638201465,
26.2701290765727));
#33632=CARTESIAN_POINT('Ctrl Pts',(-8.53569673155563,-1.20766451060123,
26.2932829974218));
#33633=CARTESIAN_POINT('Ctrl Pts',(-7.96862971961702,-1.08506643242179,
26.3164369182709));
#33634=CARTESIAN_POINT('Ctrl Pts',(-7.52408562998623,-0.712268897887968,
26.3395908391199));
#33635=CARTESIAN_POINT('Ctrl Pts',(-7.3045888942105,-0.175221508976678,
26.362744759969));
#33636=CARTESIAN_POINT('Ctrl Pts',(-7.3607162329992,0.40220344447028,26.3858986808181));
#33637=CARTESIAN_POINT('Ctrl Pts',(-7.67960987803532,0.886917649849614,
26.4090526016672));
#33638=CARTESIAN_POINT('Ctrl Pts',(-8.01824276791755,1.07361062937922,26.4244885488999));
#33639=CARTESIAN_POINT('Ctrl Pts',(-8.19963467333831,1.12216314098435,26.4322065225163));
#33640=CARTESIAN_POINT('Ctrl Pts',(-7.58018086668817,-0.797569598526346,
25.1033804324511));
#33641=CARTESIAN_POINT('Ctrl Pts',(-7.45125783945751,-0.648885562186007,
25.1110984060675));
#33642=CARTESIAN_POINT('Ctrl Pts',(-7.26699422441166,-0.287944055291513,
25.1265343533002));
#33643=CARTESIAN_POINT('Ctrl Pts',(-7.27490933478883,0.320073790042177,
25.1496882741493));
#33644=CARTESIAN_POINT('Ctrl Pts',(-7.56534960679844,0.854222305267502,
25.1728421949984));
#33645=CARTESIAN_POINT('Ctrl Pts',(-8.07130426329821,1.19143406615391,25.1959961158475));
#33646=CARTESIAN_POINT('Ctrl Pts',(-8.67611707899071,1.25389968911121,25.2191500366966));
#33647=CARTESIAN_POINT('Ctrl Pts',(-9.24031759749596,1.02723717888941,25.2423039575457));
#33648=CARTESIAN_POINT('Ctrl Pts',(-9.63380998027999,0.563701825632449,
25.2654578783947));
#33649=CARTESIAN_POINT('Ctrl Pts',(-9.76585774871632,-0.0298155050651843,
25.2886117992438));
#33650=CARTESIAN_POINT('Ctrl Pts',(-9.60601270884069,-0.616458373015401,
25.3117657200929));
#33651=CARTESIAN_POINT('Ctrl Pts',(-9.19113309833576,-1.06095233793524,
25.334919640942));
#33652=CARTESIAN_POINT('Ctrl Pts',(-8.61688576258933,-1.26080238756323,
25.3580735617911));
#33653=CARTESIAN_POINT('Ctrl Pts',(-8.01568582487961,-1.16992507024812,
25.3812274826402));
#33654=CARTESIAN_POINT('Ctrl Pts',(-7.52616347069768,-0.809275800827533,
25.4043814034893));
#33655=CARTESIAN_POINT('Ctrl Pts',(-7.26119721213712,-0.262016330420185,
25.4275353243383));
#33656=CARTESIAN_POINT('Ctrl Pts',(-7.28188538871804,0.345661246443408,
25.4506892451874));
#33657=CARTESIAN_POINT('Ctrl Pts',(-7.58345752963543,0.873633106680533,
25.4738431660365));
#33658=CARTESIAN_POINT('Ctrl Pts',(-8.09637438422115,1.20015468433752,25.4969970868856));
#33659=CARTESIAN_POINT('Ctrl Pts',(-8.70236291049992,1.2499336610416,25.5201510077347));
#33660=CARTESIAN_POINT('Ctrl Pts',(-9.26168875325356,1.01149154594881,25.5433049285838));
#33661=CARTESIAN_POINT('Ctrl Pts',(-9.64537746361254,0.539810494764398,
25.5664588494329));
#33662=CARTESIAN_POINT('Ctrl Pts',(-9.76495460306173,-0.0563449784938296,
25.5896127702819));
#33663=CARTESIAN_POINT('Ctrl Pts',(-9.59284698531382,-0.639507913234122,
25.612766691131));
#33664=CARTESIAN_POINT('Ctrl Pts',(-9.16874075292704,-1.07520728689,25.6359206119801));
#33665=CARTESIAN_POINT('Ctrl Pts',(-8.59043018492992,-1.26297556827349,
25.6590745328292));
#33666=CARTESIAN_POINT('Ctrl Pts',(-7.99126740099621,-1.15951543634185,
25.6822284536783));
#33667=CARTESIAN_POINT('Ctrl Pts',(-7.50941281472855,-0.788683670922342,
25.7053823745274));
#33668=CARTESIAN_POINT('Ctrl Pts',(-7.25597684673547,-0.235990039080846,
25.7285362953765));
#33669=CARTESIAN_POINT('Ctrl Pts',(-7.28939907153445,0.371120326042741,
25.7516902162256));
#33670=CARTESIAN_POINT('Ctrl Pts',(-7.60197268802659,0.892654385164513,
25.7748441370747));
#33671=CARTESIAN_POINT('Ctrl Pts',(-8.12162162390845,1.2083520633118,25.7979980579237));
#33672=CARTESIAN_POINT('Ctrl Pts',(-8.7285204930998,1.2454169135826,25.8211519787728));
#33673=CARTESIAN_POINT('Ctrl Pts',(-9.2827250249746,0.995302185107979,25.8443058996219));
#33674=CARTESIAN_POINT('Ctrl Pts',(-9.65644168929986,0.515681610740635,
25.867459820471));
#33675=CARTESIAN_POINT('Ctrl Pts',(-9.76349549273147,-0.0828495277344286,
25.8906137413201));
#33676=CARTESIAN_POINT('Ctrl Pts',(-9.57920099393642,-0.662276467266634,
25.9137676621692));
#33677=CARTESIAN_POINT('Ctrl Pts',(-9.14605449749695,-1.08898966509019,
25.9369215830183));
#33678=CARTESIAN_POINT('Ctrl Pts',(-8.56393486896201,-1.2645937042741,25.9600755038673));
#33679=CARTESIAN_POINT('Ctrl Pts',(-7.96707255574195,-1.14859620568215,
25.9832294247164));
#33680=CARTESIAN_POINT('Ctrl Pts',(-7.49309750825848,-0.767744929110479,
26.0063833455655));
#33681=CARTESIAN_POINT('Ctrl Pts',(-7.25130321058993,-0.209860032372193,
26.0295372664146));
#33682=CARTESIAN_POINT('Ctrl Pts',(-7.29744479634916,0.396416303503929,
26.0526911872637));
#33683=CARTESIAN_POINT('Ctrl Pts',(-7.62088251501485,0.911283354515532,
26.0758451081128));
#33684=CARTESIAN_POINT('Ctrl Pts',(-8.14703515781832,1.21601839122289,26.0989990289619));
#33685=CARTESIAN_POINT('Ctrl Pts',(-8.75457763896279,1.24035281914371,26.122152949811));
#33686=CARTESIAN_POINT('Ctrl Pts',(-9.30341731233995,0.978675413103695,
26.14530687066));
#33687=CARTESIAN_POINT('Ctrl Pts',(-9.66699765052699,0.491326069581015,
26.1684607915091));
#33688=CARTESIAN_POINT('Ctrl Pts',(-9.76148115139229,-0.109317621909302,
26.1916147123582));
#33689=CARTESIAN_POINT('Ctrl Pts',(-9.56508058954619,-0.684754074175086,
26.2147686332073));
#33690=CARTESIAN_POINT('Ctrl Pts',(-9.12308458528742,-1.10229325462015,
26.2379225540564));
#33691=CARTESIAN_POINT('Ctrl Pts',(-8.53741089167782,-1.26565666435994,
26.2610764749055));
#33692=CARTESIAN_POINT('Ctrl Pts',(-7.94311327301097,-1.13717141591269,
26.2842303957546));
#33693=CARTESIAN_POINT('Ctrl Pts',(-7.47722213792833,-0.746472111678944,
26.3073843166037));
#33694=CARTESIAN_POINT('Ctrl Pts',(-7.24718515000566,-0.183635660921369,
26.3305382374527));
#33695=CARTESIAN_POINT('Ctrl Pts',(-7.30600772843461,0.421517288496708,
26.3536921583018));
#33696=CARTESIAN_POINT('Ctrl Pts',(-7.64021467375676,0.929507511744114,
26.3768460791509));
#33697=CARTESIAN_POINT('Ctrl Pts',(-7.99510874416174,1.12516550422186,26.3922820263836));
#33698=CARTESIAN_POINT('Ctrl Pts',(-8.1852111044956,1.17604951161383,26.4));
#33699=CARTESIAN_POINT('Ctrl Pts',(-8.1852111044956,1.17604951161383,26.4));
#33700=CARTESIAN_POINT('Ctrl Pts',(-8.13719978503581,1.15963878614564,26.4));
#33701=CARTESIAN_POINT('Ctrl Pts',(-8.09039266389787,1.14022121612444,26.4));
#33702=CARTESIAN_POINT('Ctrl Pts',(-8.045027575811,1.1179877975994,26.4));
#33703=CARTESIAN_POINT('Ctrl Pts',(-7.99968396671727,1.09576490592363,26.4));
#33704=CARTESIAN_POINT('Ctrl Pts',(-7.95578012736231,1.07072813106631,26.4));
#33705=CARTESIAN_POINT('Ctrl Pts',(-7.91358079345595,1.04302395957461,26.4));
#33706=CARTESIAN_POINT('Ctrl Pts',(-7.87480205233853,1.01756543227811,26.4));
#33707=CARTESIAN_POINT('Ctrl Pts',(-7.83746246318038,0.989853539891906,
26.4));
#33708=CARTESIAN_POINT('Ctrl Pts',(-7.80179749749225,0.959976425281334,
26.4));
#33709=CARTESIAN_POINT('Ctrl Pts',(-7.79470173084572,0.954032187588742,
26.4));
#33710=CARTESIAN_POINT('Ctrl Pts',(-7.78767071045979,0.948000723246587,
26.4));
#33711=CARTESIAN_POINT('Ctrl Pts',(-7.78071179729939,0.941887340642186,
26.4));
#33712=CARTESIAN_POINT('Ctrl Pts',(-7.75269360207171,0.917273447155726,
26.4));
#33713=CARTESIAN_POINT('Ctrl Pts',(-7.72591293956663,0.891394850496869,
26.4));
#33714=CARTESIAN_POINT('Ctrl Pts',(-7.70047126076455,0.864315910058709,
26.4));
#33715=CARTESIAN_POINT('Ctrl Pts',(-7.66652682771193,0.82818703318742,26.4));
#33716=CARTESIAN_POINT('Ctrl Pts',(-7.63496397922782,0.78992201446398,26.4));
#33717=CARTESIAN_POINT('Ctrl Pts',(-7.60593250072696,0.749787089159704,
26.4));
#33718=CARTESIAN_POINT('Ctrl Pts',(-7.58573725869745,0.721867927883357,
26.4));
#33719=CARTESIAN_POINT('Ctrl Pts',(-7.56676781226386,0.693043181405103,
26.4));
#33720=CARTESIAN_POINT('Ctrl Pts',(-7.54908829087147,0.663396724297125,
26.4));
#33721=CARTESIAN_POINT('Ctrl Pts',(-7.53965742741635,0.647582286637428,
26.4));
#33722=CARTESIAN_POINT('Ctrl Pts',(-7.53059381571656,0.631533970667596,
26.4));
#33723=CARTESIAN_POINT('Ctrl Pts',(-7.52190863960029,0.615264252922367,
26.4));
#33724=CARTESIAN_POINT('Ctrl Pts',(-7.51748928486193,0.606985588995857,
26.4));
#33725=CARTESIAN_POINT('Ctrl Pts',(-7.51316793018883,0.598649598701858,
26.4));
#33726=CARTESIAN_POINT('Ctrl Pts',(-7.508946155198,0.590257920257115,26.4));
#33727=CARTESIAN_POINT('Ctrl Pts',(-7.50442378911426,0.581268752888771,
26.4));
#33728=CARTESIAN_POINT('Ctrl Pts',(-7.50001905759358,0.572222229998695,
26.4));
#33729=CARTESIAN_POINT('Ctrl Pts',(-7.49573669483179,0.563127939236245,
26.4));
#33730=CARTESIAN_POINT('Ctrl Pts',(-7.47506542038098,0.519229140665572,
26.4));
#33731=CARTESIAN_POINT('Ctrl Pts',(-7.45721490167107,0.474166034199356,
26.4));
#33732=CARTESIAN_POINT('Ctrl Pts',(-7.44233264532585,0.428186070859631,
26.4));
#33733=CARTESIAN_POINT('Ctrl Pts',(-7.43702167377983,0.411777384480363,
26.4));
#33734=CARTESIAN_POINT('Ctrl Pts',(-7.4320891762645,0.39525178308813,26.4));
#33735=CARTESIAN_POINT('Ctrl Pts',(-7.42754343216099,0.378620146479998,
26.4));
#33736=CARTESIAN_POINT('Ctrl Pts',(-7.41562255541274,0.335004913063347,
26.4));
#33737=CARTESIAN_POINT('Ctrl Pts',(-7.40635865253341,0.290660154332935,
26.4));
#33738=CARTESIAN_POINT('Ctrl Pts',(-7.39978193143838,0.245833148209606,
26.4));
#33739=CARTESIAN_POINT('Ctrl Pts',(-7.39701831329359,0.226996295360151,
26.4));
#33740=CARTESIAN_POINT('Ctrl Pts',(-7.39472966852691,0.208074337051025,
26.4));
#33741=CARTESIAN_POINT('Ctrl Pts',(-7.39292029821568,0.189086061607282,
26.4));
#33742=CARTESIAN_POINT('Ctrl Pts',(-7.39203040388929,0.179747144924149,
26.4));
#33743=CARTESIAN_POINT('Ctrl Pts',(-7.39125632551953,0.170390221780269,
26.4));
#33744=CARTESIAN_POINT('Ctrl Pts',(-7.3905991129645,0.161023830066182,26.4));
#33745=CARTESIAN_POINT('Ctrl Pts',(-7.38726308367779,0.113479764101907,
26.4));
#33746=CARTESIAN_POINT('Ctrl Pts',(-7.38694582795301,0.0658794268722831,
26.4));
#33747=CARTESIAN_POINT('Ctrl Pts',(-7.38964467812272,0.0185117250965961,
26.4));
#33748=CARTESIAN_POINT('Ctrl Pts',(-7.39231294873441,-0.028319272789147,
26.4));
#33749=CARTESIAN_POINT('Ctrl Pts',(-7.39792954447875,-0.0749239502970285,
26.4));
#33750=CARTESIAN_POINT('Ctrl Pts',(-7.40654136040071,-0.121014043924224,
26.4));
#33751=CARTESIAN_POINT('Ctrl Pts',(-7.40892324964069,-0.13376181966341,
26.4));
#33752=CARTESIAN_POINT('Ctrl Pts',(-7.41153455473596,-0.146470124525479,
26.4));
#33753=CARTESIAN_POINT('Ctrl Pts',(-7.41437692003386,-0.159132568267465,
26.4));
#33754=CARTESIAN_POINT('Ctrl Pts',(-7.41931563096904,-0.181134015238621,
26.4));
#33755=CARTESIAN_POINT('Ctrl Pts',(-7.42495181516823,-0.202997104027968,
26.4));
#33756=CARTESIAN_POINT('Ctrl Pts',(-7.43127552851572,-0.224690029431199,
26.4));
#33757=CARTESIAN_POINT('Ctrl Pts',(-7.43448552072453,-0.235701616722459,
26.4));
#33758=CARTESIAN_POINT('Ctrl Pts',(-7.43787270196213,-0.246669331595252,
26.4));
#33759=CARTESIAN_POINT('Ctrl Pts',(-7.44143596905709,-0.257588833328584,
26.4));
#33760=CARTESIAN_POINT('Ctrl Pts',(-7.44466453004633,-0.267482640438386,
26.4));
#33761=CARTESIAN_POINT('Ctrl Pts',(-7.44803504929267,-0.277328758820201,
26.4));
#33762=CARTESIAN_POINT('Ctrl Pts',(-7.4515445537233,-0.287120147614807,
26.4));
#33763=CARTESIAN_POINT('Ctrl Pts',(-7.46731925100687,-0.331130975147226,
26.4));
#33764=CARTESIAN_POINT('Ctrl Pts',(-7.48590735102023,-0.374065461792036,
26.4));
#33765=CARTESIAN_POINT('Ctrl Pts',(-7.50719015735612,-0.415648998792841,
26.4));
#33766=CARTESIAN_POINT('Ctrl Pts',(-7.51904253208635,-0.438806831240468,
26.4));
#33767=CARTESIAN_POINT('Ctrl Pts',(-7.53173142467898,-0.461545209553912,
26.4));
#33768=CARTESIAN_POINT('Ctrl Pts',(-7.54524163262262,-0.483812028629736,
26.4));
#33769=CARTESIAN_POINT('Ctrl Pts',(-7.55097536126223,-0.493262060692935,
26.4));
#33770=CARTESIAN_POINT('Ctrl Pts',(-7.55685648518396,-0.502625914171693,
26.4));
#33771=CARTESIAN_POINT('Ctrl Pts',(-7.56287699180982,-0.511889479160034,
26.4));
#33772=CARTESIAN_POINT('Ctrl Pts',(-7.58817006364992,-0.550807136644064,
26.4));
#33773=CARTESIAN_POINT('Ctrl Pts',(-7.61595022831774,-0.588008141121294,
26.4));
#33774=CARTESIAN_POINT('Ctrl Pts',(-7.64611613239271,-0.62320527942628,
26.4));
#33775=CARTESIAN_POINT('Ctrl Pts',(-7.66532276604225,-0.645615300331212,
26.4));
#33776=CARTESIAN_POINT('Ctrl Pts',(-7.6854974434774,-0.667212207978329,
26.4));
#33777=CARTESIAN_POINT('Ctrl Pts',(-7.70658042403511,-0.687941803185361,
26.4));
#33778=CARTESIAN_POINT('Ctrl Pts',(-7.70661869325989,-0.687936125025681,
25.2));
#33779=CARTESIAN_POINT('Ctrl Pts',(-7.67409908369756,-0.655902484444094,
25.2));
#33780=CARTESIAN_POINT('Ctrl Pts',(-7.64381552971734,-0.621809035232042,
25.2));
#33781=CARTESIAN_POINT('Ctrl Pts',(-7.61585836477246,-0.585955246406357,
25.2));
#33782=CARTESIAN_POINT('Ctrl Pts',(-7.58750223492001,-0.549589803284789,
25.2));
#33783=CARTESIAN_POINT('Ctrl Pts',(-7.56153863793393,-0.511412632439867,
25.2));
#33784=CARTESIAN_POINT('Ctrl Pts',(-7.53809218129987,-0.471690967864502,
25.2));
#33785=CARTESIAN_POINT('Ctrl Pts',(-7.51733028405296,-0.436517332408129,
25.2));
#33786=CARTESIAN_POINT('Ctrl Pts',(-7.49854222357723,-0.400131575643489,
25.2));
#33787=CARTESIAN_POINT('Ctrl Pts',(-7.48184098880052,-0.362698062471297,
25.2));
#33788=CARTESIAN_POINT('Ctrl Pts',(-7.47711369552762,-0.352102486912628,
25.2));
#33789=CARTESIAN_POINT('Ctrl Pts',(-7.47255243649911,-0.341419159457484,
25.2));
#33790=CARTESIAN_POINT('Ctrl Pts',(-7.46817016271403,-0.330677368055269,
25.2));
#33791=CARTESIAN_POINT('Ctrl Pts',(-7.45707013423535,-0.303469074752666,
25.2));
#33792=CARTESIAN_POINT('Ctrl Pts',(-7.44710388175771,-0.275856356158202,
25.2));
#33793=CARTESIAN_POINT('Ctrl Pts',(-7.43829878902219,-0.247907854317032,
25.2));
#33794=CARTESIAN_POINT('Ctrl Pts',(-7.42417917490964,-0.203090375061034,
25.2));
#33795=CARTESIAN_POINT('Ctrl Pts',(-7.4130426814431,-0.157410581164318,
25.2));
#33796=CARTESIAN_POINT('Ctrl Pts',(-7.40485403128444,-0.111171922541295,
25.2));
#33797=CARTESIAN_POINT('Ctrl Pts',(-7.39906737058042,-0.078496521385322,
25.2));
#33798=CARTESIAN_POINT('Ctrl Pts',(-7.39475376399804,-0.0455412949444171,
25.2));
#33799=CARTESIAN_POINT('Ctrl Pts',(-7.39191539897434,-0.0124075347941399,
25.2));
#33800=CARTESIAN_POINT('Ctrl Pts',(-7.39015663071979,0.00812351213599617,
25.2));
#33801=CARTESIAN_POINT('Ctrl Pts',(-7.38896453092616,0.0287231847245958,
25.2));
#33802=CARTESIAN_POINT('Ctrl Pts',(-7.38834204837582,0.0493677427878705,
25.2));
#33803=CARTESIAN_POINT('Ctrl Pts',(-7.38797993275816,0.0613772632001962,
25.2));
#33804=CARTESIAN_POINT('Ctrl Pts',(-7.38781079076705,0.0734063969638433,
25.2));
#33805=CARTESIAN_POINT('Ctrl Pts',(-7.38783494145012,0.0854216419247253,
25.2));
#33806=CARTESIAN_POINT('Ctrl Pts',(-7.38793210908909,0.133763669381329,
25.2));
#33807=CARTESIAN_POINT('Ctrl Pts',(-7.39114956164653,0.181962052576744,
25.2));
#33808=CARTESIAN_POINT('Ctrl Pts',(-7.39745513654038,0.229705853778749,
25.2));
#33809=CARTESIAN_POINT('Ctrl Pts',(-7.39993171457249,0.248457712446122,
25.2));
#33810=CARTESIAN_POINT('Ctrl Pts',(-7.40288520968687,0.267139634278219,
25.2));
#33811=CARTESIAN_POINT('Ctrl Pts',(-7.40631580517995,0.285733272919791,
25.2));
#33812=CARTESIAN_POINT('Ctrl Pts',(-7.41475571884804,0.331477140195014,
25.2));
#33813=CARTESIAN_POINT('Ctrl Pts',(-7.42608006767679,0.376687101444302,
25.2));
#33814=CARTESIAN_POINT('Ctrl Pts',(-7.44015868375257,0.421133147358343,
25.2));
#33815=CARTESIAN_POINT('Ctrl Pts',(-7.44619887655232,0.44020197380139,25.2));
#33816=CARTESIAN_POINT('Ctrl Pts',(-7.45274661951137,0.459130118611719,
25.2));
#33817=CARTESIAN_POINT('Ctrl Pts',(-7.45979413108642,0.477898840262571,
25.2));
#33818=CARTESIAN_POINT('Ctrl Pts',(-7.46424294742261,0.489746794622125,
25.2));
#33819=CARTESIAN_POINT('Ctrl Pts',(-7.46889308133366,0.501535927254051,
25.2));
#33820=CARTESIAN_POINT('Ctrl Pts',(-7.47373049342834,0.513232826928775,
25.2));
#33821=CARTESIAN_POINT('Ctrl Pts',(-7.49246868158931,0.558541910115242,
25.2));
#33822=CARTESIAN_POINT('Ctrl Pts',(-7.51403763849658,0.60254052436522,25.2));
#33823=CARTESIAN_POINT('Ctrl Pts',(-7.5382574080668,0.644974713240491,25.2));
#33824=CARTESIAN_POINT('Ctrl Pts',(-7.56269829320146,0.687796307107259,
25.2));
#33825=CARTESIAN_POINT('Ctrl Pts',(-7.58983893767671,0.729025863014533,
25.2));
#33826=CARTESIAN_POINT('Ctrl Pts',(-7.61954528866539,0.768390684532343,
25.2));
#33827=CARTESIAN_POINT('Ctrl Pts',(-7.6249432342603,0.775543672288655,25.2));
#33828=CARTESIAN_POINT('Ctrl Pts',(-7.63042602246557,0.782635032671784,
25.2));
#33829=CARTESIAN_POINT('Ctrl Pts',(-7.63599301409741,0.789663044280778,
25.2));
#33830=CARTESIAN_POINT('Ctrl Pts',(-7.65117037049777,0.808823597058622,
25.2));
#33831=CARTESIAN_POINT('Ctrl Pts',(-7.66697341498186,0.827513438421461,
25.2));
#33832=CARTESIAN_POINT('Ctrl Pts',(-7.68337390615606,0.845711906332443,
25.2));
#33833=CARTESIAN_POINT('Ctrl Pts',(-7.69112608445907,0.854313951636385,
25.2));
#33834=CARTESIAN_POINT('Ctrl Pts',(-7.69901178372298,0.862806182343179,
25.2));
#33835=CARTESIAN_POINT('Ctrl Pts',(-7.70702820259955,0.871186249340306,
25.2));
#33836=CARTESIAN_POINT('Ctrl Pts',(-7.71445585235118,0.878950838929277,
25.2));
#33837=CARTESIAN_POINT('Ctrl Pts',(-7.72199001781368,0.886613096267017,
25.2));
#33838=CARTESIAN_POINT('Ctrl Pts',(-7.72962411164412,0.89416783589762,25.2));
#33839=CARTESIAN_POINT('Ctrl Pts',(-7.76528208932064,0.929455159197961,
25.2));
#33840=CARTESIAN_POINT('Ctrl Pts',(-7.80314201059037,0.962425606050914,
25.2));
#33841=CARTESIAN_POINT('Ctrl Pts',(-7.84293252810485,0.992923651767303,
25.2));
#33842=CARTESIAN_POINT('Ctrl Pts',(-7.86518031888562,1.0099758084796,25.2));
#33843=CARTESIAN_POINT('Ctrl Pts',(-7.88803247402863,1.02625455224781,25.2));
#33844=CARTESIAN_POINT('Ctrl Pts',(-7.9114469066033,1.04172808762183,25.2));
#33845=CARTESIAN_POINT('Ctrl Pts',(-7.92363425798135,1.04978215479012,25.2));
#33846=CARTESIAN_POINT('Ctrl Pts',(-7.93597623364268,1.05761914082858,25.2));
#33847=CARTESIAN_POINT('Ctrl Pts',(-7.94844679456435,1.06522236279636,25.2));
#33848=CARTESIAN_POINT('Ctrl Pts',(-7.99400675878279,1.09299998426606,25.2));
#33849=CARTESIAN_POINT('Ctrl Pts',(-8.04133383320788,1.11769842594191,25.2));
#33850=CARTESIAN_POINT('Ctrl Pts',(-8.09012873835892,1.13911714460503,25.2));
#33851=CARTESIAN_POINT('Ctrl Pts',(-8.1212439149797,1.1527752757589,25.2));
#33852=CARTESIAN_POINT('Ctrl Pts',(-8.15295691405469,1.16509895636455,25.2));
#33853=CARTESIAN_POINT('Ctrl Pts',(-8.18517804880577,1.17607982959758,25.2));
#33854=CARTESIAN_POINT('Ctrl Pts',(-9.5501656695242,-1.36966039699926E-5,
25.6841069671524));
#33855=CARTESIAN_POINT('Ctrl Pts',(-9.55006298344665,0.154119342427657,
25.6770974504288));
#33856=CARTESIAN_POINT('Ctrl Pts',(-9.515673521871,0.308296731012387,25.6700879337053));
#33857=CARTESIAN_POINT('Ctrl Pts',(-9.44996669084627,0.447714404793194,
25.6630784169817));
#33858=CARTESIAN_POINT('Ctrl Pts',(-9.37761882318798,0.601223123059134,
25.6553604433654));
#33859=CARTESIAN_POINT('Ctrl Pts',(-9.26730313198972,0.736837801786184,
25.647642469749));
#33860=CARTESIAN_POINT('Ctrl Pts',(-9.13173841581746,0.838922806907227,
25.6399244961327));
#33861=CARTESIAN_POINT('Ctrl Pts',(-8.99617369964519,0.941007812028272,
25.6322065225163));
#33862=CARTESIAN_POINT('Ctrl Pts',(-8.83535995849891,1.00956314354331,25.6244885488999));
#33863=CARTESIAN_POINT('Ctrl Pts',(-8.66783814118664,1.03668474492625,25.6167705752836));
#33864=CARTESIAN_POINT('Ctrl Pts',(-8.50031632387437,1.06380634630919,25.6090526016672));
#33865=CARTESIAN_POINT('Ctrl Pts',(-8.3260864303961,1.04949421756004,25.6013346280509));
#33866=CARTESIAN_POINT('Ctrl Pts',(-8.16523621882741,0.995398469324722,
25.5936166544345));
#33867=CARTESIAN_POINT('Ctrl Pts',(-8.00438600725873,0.941302721089401,
25.5858986808181));
#33868=CARTESIAN_POINT('Ctrl Pts',(-7.85691547759961,0.847423353367908,
25.5781807072018));
#33869=CARTESIAN_POINT('Ctrl Pts',(-7.73982717908252,0.724584145853212,
25.5704627335854));
#33870=CARTESIAN_POINT('Ctrl Pts',(-7.62273888056543,0.601744938338516,
25.562744759969));
#33871=CARTESIAN_POINT('Ctrl Pts',(-7.53603281319035,0.449945891030617,
25.5550267863527));
#33872=CARTESIAN_POINT('Ctrl Pts',(-7.48970571428075,0.28668860819909,25.5473088127363));
#33873=CARTESIAN_POINT('Ctrl Pts',(-7.44337861537115,0.123431325367562,
25.5395908391199));
#33874=CARTESIAN_POINT('Ctrl Pts',(-7.43743048492702,-0.0512841929875971,
25.5318728655036));
#33875=CARTESIAN_POINT('Ctrl Pts',(-7.47254711037184,-0.217314200152739,
25.5241548918872));
#33876=CARTESIAN_POINT('Ctrl Pts',(-7.50766373581667,-0.383344207317882,
25.5164369182709));
#33877=CARTESIAN_POINT('Ctrl Pts',(-7.58384511715045,-0.540688703293009,
25.5087189446545));
#33878=CARTESIAN_POINT('Ctrl Pts',(-7.69230795508232,-0.671206721513239,
25.5010009710381));
#33879=CARTESIAN_POINT('Ctrl Pts',(-7.80077079301418,-0.801724739733468,
25.4932829974218));
#33880=CARTESIAN_POINT('Ctrl Pts',(-7.94151508754413,-0.9054162801988,25.4855650238054));
#33881=CARTESIAN_POINT('Ctrl Pts',(-8.0983137895737,-0.97032627906681,25.4778470501891));
#33882=CARTESIAN_POINT('Ctrl Pts',(-8.25511249160327,-1.03523627793482,
25.4701290765727));
#33883=CARTESIAN_POINT('Ctrl Pts',(-8.42796560113247,-1.06136473520551,
25.4624111029563));
#33884=CARTESIAN_POINT('Ctrl Pts',(-8.59694409194747,-1.04569916835105,
25.45469312934));
#33885=CARTESIAN_POINT('Ctrl Pts',(-8.76592258276247,-1.0300336014966,25.4469751557236));
#33886=CARTESIAN_POINT('Ctrl Pts',(-8.93102645486326,-0.972574010516992,
25.4392571821072));
#33887=CARTESIAN_POINT('Ctrl Pts',(-9.07322013923887,-0.879945203081139,
25.4315392084909));
#33888=CARTESIAN_POINT('Ctrl Pts',(-9.21541382361448,-0.787316395645285,
25.4238212348745));
#33889=CARTESIAN_POINT('Ctrl Pts',(-9.33469732026492,-0.659518371753182,
25.4161032612582));
#33890=CARTESIAN_POINT('Ctrl Pts',(-9.41731787352031,-0.511285482216741,
25.4083852876418));
#33891=CARTESIAN_POINT('Ctrl Pts',(-9.4999384267757,-0.3630525926803,25.4006673140254));
#33892=CARTESIAN_POINT('Ctrl Pts',(-9.54589603663603,-0.19438483749952,
25.3929493404091));
#33893=CARTESIAN_POINT('Ctrl Pts',(-9.54989208229683,-0.0247288318319217,
25.3852313667927));
#33894=CARTESIAN_POINT('Ctrl Pts',(-9.55008613808259,-0.0164900046805863,
25.3848565669126));
#33895=CARTESIAN_POINT('Ctrl Pts',(-9.55018123744808,-0.00824884697431659,
25.3844817670325));
#33896=CARTESIAN_POINT('Ctrl Pts',(-9.55017788167088,-7.61182092967605E-6,
25.3841069671524));
#33897=CARTESIAN_POINT('Ctrl Pts',(-8.8147888955044,1.17604951161383,25.2));
#33898=CARTESIAN_POINT('Ctrl Pts',(-9.00489125583826,1.12516550422186,25.2077179736164));
#33899=CARTESIAN_POINT('Ctrl Pts',(-9.35978529202387,0.929507318017654,
25.2231539208491));
#33900=CARTESIAN_POINT('Ctrl Pts',(-9.69399227712924,0.421517236998932,
25.2463078416982));
#33901=CARTESIAN_POINT('Ctrl Pts',(-9.75281486267965,-0.183635718934528,
25.2694617625473));
#33902=CARTESIAN_POINT('Ctrl Pts',(-9.52277787696657,-0.746472135969,25.2926156833964));
#33903=CARTESIAN_POINT('Ctrl Pts',(-9.05688673586305,-1.13717144686837,
25.3157696042454));
#33904=CARTESIAN_POINT('Ctrl Pts',(-8.46258910686823,-1.26565668871267,
25.3389235250945));
#33905=CARTESIAN_POINT('Ctrl Pts',(-7.87691540315674,-1.10229327660247,
25.3620774459436));
#33906=CARTESIAN_POINT('Ctrl Pts',(-7.43491939071853,-0.684754086769719,
25.3852313667927));
#33907=CARTESIAN_POINT('Ctrl Pts',(-7.23851882542848,-0.109317624216872,
25.4083852876418));
#33908=CARTESIAN_POINT('Ctrl Pts',(-7.3330023279845,0.49132607864821,25.4315392084909));
#33909=CARTESIAN_POINT('Ctrl Pts',(-7.69658267289797,0.978675431042071,
25.45469312934));
#33910=CARTESIAN_POINT('Ctrl Pts',(-8.24542235634912,1.24035284195992,25.477847050189));
#33911=CARTESIAN_POINT('Ctrl Pts',(-8.85296484867377,1.21601841356867,25.5010009710381));
#33912=CARTESIAN_POINT('Ctrl Pts',(-9.37911750114581,0.911283371272776,
25.5241548918872));
#33913=CARTESIAN_POINT('Ctrl Pts',(-9.70255522576049,0.396416310789831,
25.5473088127363));
#33914=CARTESIAN_POINT('Ctrl Pts',(-9.7486968123668,-0.209860036229624,
25.5704627335854));
#33915=CARTESIAN_POINT('Ctrl Pts',(-9.50690251025353,-0.767744943225855,
25.5936166544345));
#33916=CARTESIAN_POINT('Ctrl Pts',(-9.03292745405576,-1.14859622679878,
25.6167705752836));
#33917=CARTESIAN_POINT('Ctrl Pts',(-8.4360651298626,-1.26459372752363,25.6399244961327));
#33918=CARTESIAN_POINT('Ctrl Pts',(-7.85394549062537,-1.08898968511111,
25.6630784169818));
#33919=CARTESIAN_POINT('Ctrl Pts',(-7.42079898622258,-0.662276479442534,
25.6862323378308));
#33920=CARTESIAN_POINT('Ctrl Pts',(-7.23650448403929,-0.0828495292575919,
25.7093862586799));
#33921=CARTESIAN_POINT('Ctrl Pts',(-7.34355828943908,0.515681620221391,
25.732540179529));
#33922=CARTESIAN_POINT('Ctrl Pts',(-7.71727496063508,0.995302203406518,
25.7556941003781));
#33923=CARTESIAN_POINT('Ctrl Pts',(-8.27147950269888,1.24541693647946,25.7788480212272));
#33924=CARTESIAN_POINT('Ctrl Pts',(-8.878378383048,1.20835208552723,25.8020019420763));
#33925=CARTESIAN_POINT('Ctrl Pts',(-9.39802732848356,0.892654401575867,
25.8251558629253));
#33926=CARTESIAN_POINT('Ctrl Pts',(-9.71060095072233,0.371120332865739,
25.8483097837744));
#33927=CARTESIAN_POINT('Ctrl Pts',(-9.74402317613577,-0.235990043419514,
25.8714637046235));
#33928=CARTESIAN_POINT('Ctrl Pts',(-9.49058720348329,-0.788683685422225,
25.8946176254726));
#33929=CARTESIAN_POINT('Ctrl Pts',(-9.00873260835677,-1.15951545765943,
25.9177715463217));
#33930=CARTESIAN_POINT('Ctrl Pts',(-8.40956981340752,-1.26297559149317,
25.9409254671708));
#33931=CARTESIAN_POINT('Ctrl Pts',(-7.83125923477822,-1.07520730665756,
25.9640793880199));
#33932=CARTESIAN_POINT('Ctrl Pts',(-7.40715299459429,-0.63950792499141,
25.987233308869));
#33933=CARTESIAN_POINT('Ctrl Pts',(-7.2350453736822,-0.056344979529684,
26.0103872297181));
#33934=CARTESIAN_POINT('Ctrl Pts',(-7.35462251532982,0.539810504688725,
26.0335411505671));
#33935=CARTESIAN_POINT('Ctrl Pts',(-7.73831123274286,1.0114915645451,26.0566950714162));
#33936=CARTESIAN_POINT('Ctrl Pts',(-8.29763708577969,1.24993368402129,26.0798489922653));
#33937=CARTESIAN_POINT('Ctrl Pts',(-8.90362562319939,1.20015470640273,26.1030029131144));
#33938=CARTESIAN_POINT('Ctrl Pts',(-9.41654248721522,0.873633122741245,
26.1261568339635));
#33939=CARTESIAN_POINT('Ctrl Pts',(-9.71811463367633,0.345661252800576,
26.1493107548126));
#33940=CARTESIAN_POINT('Ctrl Pts',(-9.73880281063852,-0.262016335241189,
26.1724646756617));
#33941=CARTESIAN_POINT('Ctrl Pts',(-9.47383654720263,-0.809275815695625,
26.1956185965107));
#33942=CARTESIAN_POINT('Ctrl Pts',(-8.98431418402503,-1.16992509177172,
26.2187725173598));
#33943=CARTESIAN_POINT('Ctrl Pts',(-8.38311423523835,-1.26080241069298,
26.2419264382089));
#33944=CARTESIAN_POINT('Ctrl Pts',(-7.80886688894933,-1.06095235748777,
26.265080359058));
#33945=CARTESIAN_POINT('Ctrl Pts',(-7.39398727066922,-0.616458384095017,
26.2882342799071));
#33946=CARTESIAN_POINT('Ctrl Pts',(-7.23414222788049,-0.0298155056950012,
26.3113882007562));
#33947=CARTESIAN_POINT('Ctrl Pts',(-7.36618999782964,0.563701837361564,
26.3345421216053));
#33948=CARTESIAN_POINT('Ctrl Pts',(-7.75968238765149,1.02723719824325,26.3576960424544));
#33949=CARTESIAN_POINT('Ctrl Pts',(-8.32388291100964,1.25389971972182,26.3808499633034));
#33950=CARTESIAN_POINT('Ctrl Pts',(-8.9286957354243,1.19143409461849,26.4040038841525));
#33951=CARTESIAN_POINT('Ctrl Pts',(-9.43465037119409,0.854222360422852,
26.4271578050016));
#33952=CARTESIAN_POINT('Ctrl Pts',(-9.72509064095728,0.320073835810339,
26.4503117258507));
#33953=CARTESIAN_POINT('Ctrl Pts',(-9.73300563867467,-0.287943914027406,
26.4734656466998));
#33954=CARTESIAN_POINT('Ctrl Pts',(-9.54874216054247,-0.648885562186029,
26.4889015939325));
#33955=CARTESIAN_POINT('Ctrl Pts',(-9.41981913331181,-0.797569598526366,
26.4966195675489));
#33956=CARTESIAN_POINT('Ctrl Pts',(-8.80036532666169,1.12216314098435,25.1677934774837));
#33957=CARTESIAN_POINT('Ctrl Pts',(-8.98175723208245,1.07361062937922,25.1755114511001));
#33958=CARTESIAN_POINT('Ctrl Pts',(-9.32039008931324,0.886917464999664,
25.1909473983328));
#33959=CARTESIAN_POINT('Ctrl Pts',(-9.63928377230971,0.402203395332122,
25.2141013191819));
#33960=CARTESIAN_POINT('Ctrl Pts',(-9.69541111789357,-0.175221564331685,
25.237255240031));
#33961=CARTESIAN_POINT('Ctrl Pts',(-9.47591438422618,-0.712268921065058,
25.2604091608801));
#33962=CARTESIAN_POINT('Ctrl Pts',(-9.03137028885039,-1.08506646195909,
25.2835630817291));
#33963=CARTESIAN_POINT('Ctrl Pts',(-8.46430326705704,-1.20766453383812,
25.3067170025782));
#33964=CARTESIAN_POINT('Ctrl Pts',(-7.90546502388907,-1.05178640298975,
25.3298709234273));
#33965=CARTESIAN_POINT('Ctrl Pts',(-7.48372118681235,-0.653378781440023,
25.3530248442764));
#33966=CARTESIAN_POINT('Ctrl Pts',(-7.29631965901905,-0.104308710938382,
25.3761787651255));
#33967=CARTESIAN_POINT('Ctrl Pts',(-7.38647394500143,0.468813608796805,
25.3993326859746));
#33968=CARTESIAN_POINT('Ctrl Pts',(-7.73339510590426,0.933832704199109,
25.4224866068237));
#33969=CARTESIAN_POINT('Ctrl Pts',(-8.25708705679266,1.18352010465326,25.4456405276728));
#33970=CARTESIAN_POINT('Ctrl Pts',(-8.83679206473314,1.16030067526026,25.4687944485218));
#33971=CARTESIAN_POINT('Ctrl Pts',(-9.33883650019663,0.869528536116644,
25.4919483693709));
#33972=CARTESIAN_POINT('Ctrl Pts',(-9.64745436822191,0.378252588909212,
25.51510229022));
#33973=CARTESIAN_POINT('Ctrl Pts',(-9.69148175588273,-0.200244288269261,
25.5382562110691));
#33974=CARTESIAN_POINT('Ctrl Pts',(-9.46076642387327,-0.732567012236534,
25.5614101319182));
#33975=CARTESIAN_POINT('Ctrl Pts',(-9.00850881689442,-1.09596776059079,
25.5845640527673));
#33976=CARTESIAN_POINT('Ctrl Pts',(-8.43899461376132,-1.20665027733373,
25.6077179736164));
#33977=CARTESIAN_POINT('Ctrl Pts',(-7.88354758849218,-1.03909237959457,
25.6308718944655));
#33978=CARTESIAN_POINT('Ctrl Pts',(-7.47024777663305,-0.631931093914118,
25.6540258153145));
#33979=CARTESIAN_POINT('Ctrl Pts',(-7.29439761437894,-0.0790533791840066,
25.6771797361636));
#33980=CARTESIAN_POINT('Ctrl Pts',(-7.39654623425882,0.492053183969649,
25.7003336570127));
#33981=CARTESIAN_POINT('Ctrl Pts',(-7.75313927685278,0.949697640935758,
25.7234875778618));
#33982=CARTESIAN_POINT('Ctrl Pts',(-8.28195026952663,1.18835216330059,25.7466414987109));
#33983=CARTESIAN_POINT('Ctrl Pts',(-8.861041155673,1.15298561694865,25.76979541956));
#33984=CARTESIAN_POINT('Ctrl Pts',(-9.35687988275089,0.851753142358179,
25.7929493404091));
#33985=CARTESIAN_POINT('Ctrl Pts',(-9.65513143955736,0.354115668004737,
25.8161032612581));
#33986=CARTESIAN_POINT('Ctrl Pts',(-9.68702226479751,-0.225177023373172,
25.8392571821072));
#33987=CARTESIAN_POINT('Ctrl Pts',(-9.44519868143504,-0.752546345146674,
25.8624111029563));
#33988=CARTESIAN_POINT('Ctrl Pts',(-8.98542257454059,-1.10638667431739,
25.8855650238054));
#33989=CARTESIAN_POINT('Ctrl Pts',(-8.41371330779504,-1.20510628399625,
25.9087189446545));
#33990=CARTESIAN_POINT('Ctrl Pts',(-7.86190081268282,-1.02594150716706,
25.9318728655036));
#33991=CARTESIAN_POINT('Ctrl Pts',(-7.45722704181174,-0.610205790407563,
25.9550267863527));
#33992=CARTESIAN_POINT('Ctrl Pts',(-7.29300536018796,-0.0537632630117455,
25.9781807072018));
#33993=CARTESIAN_POINT('Ctrl Pts',(-7.40710349937011,0.515076487423223,
26.0013346280509));
#33994=CARTESIAN_POINT('Ctrl Pts',(-7.77321167087187,0.965145208547828,
26.0244885488999));
#33995=CARTESIAN_POINT('Ctrl Pts',(-8.30690931699925,1.19266195430728,26.047642469749));
#33996=CARTESIAN_POINT('Ctrl Pts',(-8.88513157196049,1.14516384021616,26.0707963905981));
#33997=CARTESIAN_POINT('Ctrl Pts',(-9.37454668034144,0.833603414993973,
26.0939503114472));
#33998=CARTESIAN_POINT('Ctrl Pts',(-9.66230084695114,0.329823118269062,
26.1171042322963));
#33999=CARTESIAN_POINT('Ctrl Pts',(-9.68204109547968,-0.250010795327814,
26.1402581531454));
#34000=CARTESIAN_POINT('Ctrl Pts',(-9.42921553712026,-0.772194947827906,
26.1634120739945));
#34001=CARTESIAN_POINT('Ctrl Pts',(-8.96212299788553,-1.11631934092418,
26.1865659948435));
#34002=CARTESIAN_POINT('Ctrl Pts',(-8.38846991931377,-1.20303267793751,
26.2097199156926));
#34003=CARTESIAN_POINT('Ctrl Pts',(-7.84053447998916,-1.01233971712592,
26.2328738365417));
#34004=CARTESIAN_POINT('Ctrl Pts',(-7.44466456891651,-0.588212375202577,
26.2560277573908));
#34005=CARTESIAN_POINT('Ctrl Pts',(-7.29214359635947,-0.0284493647506621,
26.2791816782399));
#34006=CARTESIAN_POINT('Ctrl Pts',(-7.41814096196594,0.537873123661492,
26.302335599089));
#34007=CARTESIAN_POINT('Ctrl Pts',(-7.79360360342394,0.980169380228542,
26.3254895199381));
#34008=CARTESIAN_POINT('Ctrl Pts',(-8.3319525633821,1.19644626698716,26.3486434407871));
#34009=CARTESIAN_POINT('Ctrl Pts',(-8.90905297629025,1.13684280524742,26.3717973616362));
#34010=CARTESIAN_POINT('Ctrl Pts',(-9.39182486443287,0.815082050207028,
26.3949512824853));
#34011=CARTESIAN_POINT('Ctrl Pts',(-9.66895721487156,0.305408111982431,
26.4181052033344));
#34012=CARTESIAN_POINT('Ctrl Pts',(-9.67650954886066,-0.274750377259986,
26.4412591241835));
#34013=CARTESIAN_POINT('Ctrl Pts',(-9.50068898914138,-0.619153746004165,
26.4566950714162));
#34014=CARTESIAN_POINT('Ctrl Pts',(-9.37767319112124,-0.761025107359477,
26.4644130450326));
#34015=CARTESIAN_POINT('Ctrl Pts',(-8.78594175781898,1.06827677035487,25.1355869549674));
#34016=CARTESIAN_POINT('Ctrl Pts',(-8.95862320832664,1.02205575453657,25.1433049285838));
#34017=CARTESIAN_POINT('Ctrl Pts',(-9.2809948866026,0.844327611981674,25.1587408758165));
#34018=CARTESIAN_POINT('Ctrl Pts',(-9.58457526749019,0.382889553665313,
25.1818947966656));
#34019=CARTESIAN_POINT('Ctrl Pts',(-9.63800737310749,-0.166807409728842,
25.2050487175147));
#34020=CARTESIAN_POINT('Ctrl Pts',(-9.42905089148579,-0.678065706161117,
25.2282026383638));
#34021=CARTESIAN_POINT('Ctrl Pts',(-9.00585384183773,-1.0329614770498,25.2513565592128));
#34022=CARTESIAN_POINT('Ctrl Pts',(-8.46601742724585,-1.14967237896357,
25.2745104800619));
#34023=CARTESIAN_POINT('Ctrl Pts',(-7.9340146446214,-1.00127952937703,25.297664400911));
#34024=CARTESIAN_POINT('Ctrl Pts',(-7.53252298290617,-0.622003476110328,
25.3208183217601));
#34025=CARTESIAN_POINT('Ctrl Pts',(-7.35412049260963,-0.0992997976598917,
25.3439722426092));
#34026=CARTESIAN_POINT('Ctrl Pts',(-7.43994556201836,0.4463011389454,25.3671261634583));
#34027=CARTESIAN_POINT('Ctrl Pts',(-7.77020753891055,0.888989977356148,
25.3902800843074));
#34028=CARTESIAN_POINT('Ctrl Pts',(-8.2687517572362,1.12668736734659,25.4134340051565));
#34029=CARTESIAN_POINT('Ctrl Pts',(-8.82061928079252,1.10458293695185,25.4365879260056));
#34030=CARTESIAN_POINT('Ctrl Pts',(-9.29855549924744,0.827773700960511,
25.4597418468546));
#34031=CARTESIAN_POINT('Ctrl Pts',(-9.59235351068334,0.360088867028593,
25.4828957677037));
#34032=CARTESIAN_POINT('Ctrl Pts',(-9.63426669939866,-0.1906285403089,25.5060496885528));
#34033=CARTESIAN_POINT('Ctrl Pts',(-9.41463033749301,-0.697389081247213,
25.5292036094019));
#34034=CARTESIAN_POINT('Ctrl Pts',(-8.98409017973308,-1.04333929438279,
25.552357530251));
#34035=CARTESIAN_POINT('Ctrl Pts',(-8.44192409766004,-1.14870682714383,
25.5755114511001));
#34036=CARTESIAN_POINT('Ctrl Pts',(-7.91314968635899,-0.989195074078023,
25.5986653719492));
#34037=CARTESIAN_POINT('Ctrl Pts',(-7.51969656704351,-0.601585708385703,
25.6218192927982));
#34038=CARTESIAN_POINT('Ctrl Pts',(-7.35229074471859,-0.0752572291104221,
25.6449732136473));
#34039=CARTESIAN_POINT('Ctrl Pts',(-7.44953417907855,0.468424747717907,
25.6681271344964));
#34040=CARTESIAN_POINT('Ctrl Pts',(-7.78900359307048,0.904093078464998,
25.6912810553455));
#34041=CARTESIAN_POINT('Ctrl Pts',(-8.29242103635439,1.13128739012173,25.7144349761946));
#34042=CARTESIAN_POINT('Ctrl Pts',(-8.843703928298,1.09761914837007,25.7375888970437));
#34043=CARTESIAN_POINT('Ctrl Pts',(-9.31573243701821,0.810851883140491,
25.7607428178928));
#34044=CARTESIAN_POINT('Ctrl Pts',(-9.59966192839239,0.337111003143734,
25.7838967387419));
#34045=CARTESIAN_POINT('Ctrl Pts',(-9.63002135345923,-0.21436400332683,
25.8070506595909));
#34046=CARTESIAN_POINT('Ctrl Pts',(-9.39981015938679,-0.716409004871123,
25.83020458044));
#34047=CARTESIAN_POINT('Ctrl Pts',(-8.96211254072442,-1.05325789097535,
25.8533585012891));
#34048=CARTESIAN_POINT('Ctrl Pts',(-8.41785680218255,-1.14723697649933,
25.8765124221382));
#34049=CARTESIAN_POINT('Ctrl Pts',(-7.89254239058742,-0.976675707676555,
25.8996663429873));
#34050=CARTESIAN_POINT('Ctrl Pts',(-7.50730108902919,-0.580903655823716,
25.9228202638364));
#34051=CARTESIAN_POINT('Ctrl Pts',(-7.35096534669371,-0.051181546493807,
25.9459741846855));
#34052=CARTESIAN_POINT('Ctrl Pts',(-7.4595844834104,0.49034247015772,25.9691281055346));
#34053=CARTESIAN_POINT('Ctrl Pts',(-7.80811210900088,0.91879885255056,25.9922820263836));
#34054=CARTESIAN_POINT('Ctrl Pts',(-8.31618154821881,1.13539022459327,26.0154359472327));
#34055=CARTESIAN_POINT('Ctrl Pts',(-8.86663752072159,1.0901729740296,26.0385898680818));
#34056=CARTESIAN_POINT('Ctrl Pts',(-9.33255087346766,0.793573707246701,
26.0617437889309));
#34057=CARTESIAN_POINT('Ctrl Pts',(-9.60648706022596,0.313984983737547,
26.08489770978));
#34058=CARTESIAN_POINT('Ctrl Pts',(-9.62527938032086,-0.23800525541444,
26.1080516306291));
#34059=CARTESIAN_POINT('Ctrl Pts',(-9.38459452703789,-0.735114079960188,
26.1312055514782));
#34060=CARTESIAN_POINT('Ctrl Pts',(-8.93993181174604,-1.06271359007664,
26.1543594723272));
#34061=CARTESIAN_POINT('Ctrl Pts',(-8.39382560338919,-1.14526294518203,
26.1775133931763));
#34062=CARTESIAN_POINT('Ctrl Pts',(-7.87220207102899,-0.963727076764081,
26.2006673140254));
#34063=CARTESIAN_POINT('Ctrl Pts',(-7.49534186716381,-0.559966366310139,
26.2238212348745));
#34064=CARTESIAN_POINT('Ctrl Pts',(-7.35014496483845,-0.0270832238063217,
26.2469751557236));
#34065=CARTESIAN_POINT('Ctrl Pts',(-7.47009192610224,0.51204440996142,26.2701290765727));
#34066=CARTESIAN_POINT('Ctrl Pts',(-7.8275248191964,0.933101562213838,26.2932829974218));
#34067=CARTESIAN_POINT('Ctrl Pts',(-8.34002221575455,1.1389928142525,26.3164369182709));
#34068=CARTESIAN_POINT('Ctrl Pts',(-8.8894102171562,1.08225151587636,26.3395908391199));
#34069=CARTESIAN_POINT('Ctrl Pts',(-9.34899935767165,0.775941739991204,
26.362744759969));
#34070=CARTESIAN_POINT('Ctrl Pts',(-9.61282378878583,0.290742388154523,
26.3858986808181));
#34071=CARTESIAN_POINT('Ctrl Pts',(-9.62001345904665,-0.261556840492567,
26.4090526016672));
#34072=CARTESIAN_POINT('Ctrl Pts',(-9.45263581774029,-0.5894219298223,26.4244885488999));
#34073=CARTESIAN_POINT('Ctrl Pts',(-9.33552724893067,-0.724480616192588,
26.4322065225163));
#34074=CARTESIAN_POINT('Ctrl Pts',(-8.77151818897628,1.01439039972539,25.1033804324511));
#34075=CARTESIAN_POINT('Ctrl Pts',(-8.93548918457083,0.970500879693931,
25.1110984060675));
#34076=CARTESIAN_POINT('Ctrl Pts',(-9.24159968389196,0.801737758963685,
25.1265343533002));
#34077=CARTESIAN_POINT('Ctrl Pts',(-9.52986676267067,0.363575711998503,
25.1496882741493));
#34078=CARTESIAN_POINT('Ctrl Pts',(-9.5806036283214,-0.158393255125999,
25.1728421949984));
#34079=CARTESIAN_POINT('Ctrl Pts',(-9.38218739874541,-0.643862491257174,
25.1959961158475));
#34080=CARTESIAN_POINT('Ctrl Pts',(-8.98033739482507,-0.980856492140519,
25.2191500366966));
#34081=CARTESIAN_POINT('Ctrl Pts',(-8.46773158743466,-1.09168022408902,
25.2423039575456));
#34082=CARTESIAN_POINT('Ctrl Pts',(-7.96256426535373,-0.950772655764307,
25.2654578783947));
#34083=CARTESIAN_POINT('Ctrl Pts',(-7.58132477899998,-0.590628170780633,
25.2886117992438));
#34084=CARTESIAN_POINT('Ctrl Pts',(-7.41192132620021,-0.0942908843814014,
25.3117657200929));
#34085=CARTESIAN_POINT('Ctrl Pts',(-7.4934171790353,0.423788669093995,25.334919640942));
#34086=CARTESIAN_POINT('Ctrl Pts',(-7.80701997191684,0.844147250513186,
25.3580735617911));
#34087=CARTESIAN_POINT('Ctrl Pts',(-8.28041645767974,1.06985463003993,25.3812274826402));
#34088=CARTESIAN_POINT('Ctrl Pts',(-8.80444649685189,1.04886519864344,25.4043814034892));
#34089=CARTESIAN_POINT('Ctrl Pts',(-9.25827449829825,0.78601886580438,25.4275353243384));
#34090=CARTESIAN_POINT('Ctrl Pts',(-9.53725265314477,0.341925145147974,
25.4506892451874));
#34091=CARTESIAN_POINT('Ctrl Pts',(-9.5770516429146,-0.181012792348538,
25.4738431660365));
#34092=CARTESIAN_POINT('Ctrl Pts',(-9.36849425111276,-0.662211150257891,
25.4969970868856));
#34093=CARTESIAN_POINT('Ctrl Pts',(-8.95967154257173,-0.990710828174794,
25.5201510077347));
#34094=CARTESIAN_POINT('Ctrl Pts',(-8.44485358155876,-1.09076337695393,
25.5433049285838));
#34095=CARTESIAN_POINT('Ctrl Pts',(-7.9427517842258,-0.93929776856148,25.5664588494329));
#34096=CARTESIAN_POINT('Ctrl Pts',(-7.56914535745397,-0.571240322857287,
25.5896127702819));
#34097=CARTESIAN_POINT('Ctrl Pts',(-7.41018387505824,-0.0714610790368369,
25.612766691131));
#34098=CARTESIAN_POINT('Ctrl Pts',(-7.50252212389829,0.444796311466165,
25.6359206119801));
#34099=CARTESIAN_POINT('Ctrl Pts',(-7.82486790928818,0.858488515994237,
25.6590745328292));
#34100=CARTESIAN_POINT('Ctrl Pts',(-8.30289180318214,1.07422261694286,25.6822284536783));
#34101=CARTESIAN_POINT('Ctrl Pts',(-8.826366700923,1.04225267979148,25.7053823745274));
#34102=CARTESIAN_POINT('Ctrl Pts',(-9.27458499128554,0.769950623922804,
25.7285362953765));
#34103=CARTESIAN_POINT('Ctrl Pts',(-9.54419241722742,0.320106338282732,
25.7516902162256));
#34104=CARTESIAN_POINT('Ctrl Pts',(-9.57302044212097,-0.203550983280489,
25.7748441370746));
#34105=CARTESIAN_POINT('Ctrl Pts',(-9.35442163733854,-0.680271664595571,
25.7979980579237));
#34106=CARTESIAN_POINT('Ctrl Pts',(-8.93880250690824,-1.00012910763331,
25.8211519787728));
#34107=CARTESIAN_POINT('Ctrl Pts',(-8.42200029657007,-1.08936766900241,
25.8443058996219));
#34108=CARTESIAN_POINT('Ctrl Pts',(-7.92318396849201,-0.92740990818605,
25.867459820471));
#34109=CARTESIAN_POINT('Ctrl Pts',(-7.55737513624663,-0.551601521239869,
25.8906137413201));
#34110=CARTESIAN_POINT('Ctrl Pts',(-7.40892533319946,-0.0485998299758685,
25.9137676621692));
#34111=CARTESIAN_POINT('Ctrl Pts',(-7.51206546745069,0.465608452892217,
25.9369215830183));
#34112=CARTESIAN_POINT('Ctrl Pts',(-7.84301254712989,0.872452496553292,
25.9600755038674));
#34113=CARTESIAN_POINT('Ctrl Pts',(-8.32545377943837,1.07811849487926,25.9832294247164));
#34114=CARTESIAN_POINT('Ctrl Pts',(-8.84814346948268,1.03518210784304,26.0063833455655));
#34115=CARTESIAN_POINT('Ctrl Pts',(-9.29055506659387,0.753543999499429,
26.0295372664146));
#34116=CARTESIAN_POINT('Ctrl Pts',(-9.55067327350077,0.298146849206033,
26.0526911872637));
#34117=CARTESIAN_POINT('Ctrl Pts',(-9.56851766516202,-0.225999715501066,
26.0758451081128));
#34118=CARTESIAN_POINT('Ctrl Pts',(-9.33997351695551,-0.698033212092468,
26.0989990289619));
#34119=CARTESIAN_POINT('Ctrl Pts',(-8.91774062560654,-1.00910783922911,
26.1221529498109));
#34120=CARTESIAN_POINT('Ctrl Pts',(-8.39918128746461,-1.08749321242655,
26.14530687066));
#34121=CARTESIAN_POINT('Ctrl Pts',(-7.90386966206882,-0.915114436402238,
26.1684607915091));
#34122=CARTESIAN_POINT('Ctrl Pts',(-7.5460191654111,-0.531720357417699,
26.1916147123582));
#34123=CARTESIAN_POINT('Ctrl Pts',(-7.40814633331743,-0.0257170828619826,
26.2147686332073));
#34124=CARTESIAN_POINT('Ctrl Pts',(-7.52204289023854,0.486215696261348,
26.2379225540564));
#34125=CARTESIAN_POINT('Ctrl Pts',(-7.86144603496885,0.886033744199133,
26.2610764749055));
#34126=CARTESIAN_POINT('Ctrl Pts',(-8.34809186812701,1.08153936151783,26.2842303957546));
#34127=CARTESIAN_POINT('Ctrl Pts',(-8.86976745802214,1.0276602265053,26.3073843166036));
#34128=CARTESIAN_POINT('Ctrl Pts',(-9.30617385091043,0.73680142977538,26.3305382374527));
#34129=CARTESIAN_POINT('Ctrl Pts',(-9.55669036270011,0.276076664326615,
26.3536921583018));
#34130=CARTESIAN_POINT('Ctrl Pts',(-9.56351736923264,-0.248363303725146,
26.3768460791509));
#34131=CARTESIAN_POINT('Ctrl Pts',(-9.40458264633919,-0.559690113640436,
26.3922820263836));
#34132=CARTESIAN_POINT('Ctrl Pts',(-9.2933813067401,-0.687936125025699,
26.4));
#34133=CARTESIAN_POINT('Ctrl Pts',(-9.2933813067401,-0.687936125025699,
26.4));
#34134=CARTESIAN_POINT('Ctrl Pts',(-9.3259008940156,-0.655902506397881,
26.4));
#34135=CARTESIAN_POINT('Ctrl Pts',(-9.35618442453939,-0.621809077591114,
26.4));
#34136=CARTESIAN_POINT('Ctrl Pts',(-9.38414156706932,-0.585955309047688,
26.4));
#34137=CARTESIAN_POINT('Ctrl Pts',(-9.41249768479717,-0.549589872890676,
26.4));
#34138=CARTESIAN_POINT('Ctrl Pts',(-9.43846126893405,-0.511412707527682,
26.4));
#34139=CARTESIAN_POINT('Ctrl Pts',(-9.46190771414193,-0.471691048741587,
26.4));
#34140=CARTESIAN_POINT('Ctrl Pts',(-9.48266961930019,-0.436517387867455,
26.4));
#34141=CARTESIAN_POINT('Ctrl Pts',(-9.50145768537511,-0.400131603820207,
26.4));
#34142=CARTESIAN_POINT('Ctrl Pts',(-9.51815892464979,-0.362698063167964,
26.4));
#34143=CARTESIAN_POINT('Ctrl Pts',(-9.52288622415338,-0.352102468719386,
26.4));
#34144=CARTESIAN_POINT('Ctrl Pts',(-9.52744748898763,-0.341419122144753,
26.4));
#34145=CARTESIAN_POINT('Ctrl Pts',(-9.53182976813775,-0.330677311537023,
26.4));
#34146=CARTESIAN_POINT('Ctrl Pts',(-9.54292979396936,-0.303469009386603,
26.4));
#34147=CARTESIAN_POINT('Ctrl Pts',(-9.55289604429056,-0.275856282583612,
26.4));
#34148=CARTESIAN_POINT('Ctrl Pts',(-9.5617011358392,-0.247907773694988,
26.4));
#34149=CARTESIAN_POINT('Ctrl Pts',(-9.57582075051757,-0.203090275300733,
26.4));
#34150=CARTESIAN_POINT('Ctrl Pts',(-9.58695724599474,-0.157410464943264,
26.4));
#34151=CARTESIAN_POINT('Ctrl Pts',(-9.59514589843678,-0.111171791667601,
26.4));
#34152=CARTESIAN_POINT('Ctrl Pts',(-9.60093255826271,-0.0784963942267053,
26.4));
#34153=CARTESIAN_POINT('Ctrl Pts',(-9.60524616537179,-0.045541172645693,
26.4));
#34154=CARTESIAN_POINT('Ctrl Pts',(-9.6080845319163,-0.0124074180728123,
26.4));
#34155=CARTESIAN_POINT('Ctrl Pts',(-9.6098433032337,0.00812365015497431,
26.4));
#34156=CARTESIAN_POINT('Ctrl Pts',(-9.61103540510615,0.028723343930919,
26.4));
#34157=CARTESIAN_POINT('Ctrl Pts',(-9.61165788864374,0.0493679230858363,
26.4));
#34158=CARTESIAN_POINT('Ctrl Pts',(-9.61202000347441,0.0613774106196558,
26.4));
#34159=CARTESIAN_POINT('Ctrl Pts',(-9.6121891457594,0.0734065113012894,
26.4));
#34160=CARTESIAN_POINT('Ctrl Pts',(-9.61216499643434,0.0854217231952467,
26.4));
#34161=CARTESIAN_POINT('Ctrl Pts',(-9.61206783397847,0.133763757288094,
26.4));
#34162=CARTESIAN_POINT('Ctrl Pts',(-9.60885038574432,0.181962146521315,
26.4));
#34163=CARTESIAN_POINT('Ctrl Pts',(-9.60254481310853,0.22970595413251,26.4));
#34164=CARTESIAN_POINT('Ctrl Pts',(-9.60006823815714,0.248457798706134,
26.4));
#34165=CARTESIAN_POINT('Ctrl Pts',(-9.59711474664968,0.267139706625319,
26.4));
#34166=CARTESIAN_POINT('Ctrl Pts',(-9.59368415521716,0.28573333164128,26.4));
#34167=CARTESIAN_POINT('Ctrl Pts',(-9.58524424594579,0.331477195708921,
26.4));
#34168=CARTESIAN_POINT('Ctrl Pts',(-9.57391990043447,0.376687154779727,
26.4));
#34169=CARTESIAN_POINT('Ctrl Pts',(-9.55984128692189,0.42113319919065,26.4));
#34170=CARTESIAN_POINT('Ctrl Pts',(-9.55380109519868,0.440202025061907,
26.4));
#34171=CARTESIAN_POINT('Ctrl Pts',(-9.54725335317324,0.459130169423877,
26.4));
#34172=CARTESIAN_POINT('Ctrl Pts',(-9.54020584241397,0.47789889072224,26.4));
#34173=CARTESIAN_POINT('Ctrl Pts',(-9.53575702659671,0.489746844848731,
26.4));
#34174=CARTESIAN_POINT('Ctrl Pts',(-9.53110689315819,0.501535977285736,
26.4));
#34175=CARTESIAN_POINT('Ctrl Pts',(-9.52626948149497,0.513232876797037,
26.4));
#34176=CARTESIAN_POINT('Ctrl Pts',(-9.50753129667904,0.558541955303412,
26.4));
#34177=CARTESIAN_POINT('Ctrl Pts',(-9.48596234301021,0.602540565578701,
26.4));
#34178=CARTESIAN_POINT('Ctrl Pts',(-9.46174257689923,0.644974750847517,
26.4));
#34179=CARTESIAN_POINT('Ctrl Pts',(-9.43730169352057,0.687796344114401,
26.4));
#34180=CARTESIAN_POINT('Ctrl Pts',(-9.41016105064264,0.729025899571633,
26.4));
#34181=CARTESIAN_POINT('Ctrl Pts',(-9.3804547014595,0.768390720401401,26.4));
#34182=CARTESIAN_POINT('Ctrl Pts',(-9.3750567531779,0.775543712027657,26.4));
#34183=CARTESIAN_POINT('Ctrl Pts',(-9.36957396219805,0.782635076204051,
26.4));
#34184=CARTESIAN_POINT('Ctrl Pts',(-9.36400696770699,0.789663091524419,
26.4));
#34185=CARTESIAN_POINT('Ctrl Pts',(-9.3488296116131,0.808823644192825,26.4));
#34186=CARTESIAN_POINT('Ctrl Pts',(-9.33302656747451,0.827513485340246,
26.4));
#34187=CARTESIAN_POINT('Ctrl Pts',(-9.31662607666973,0.845711952950721,
26.4));
#34188=CARTESIAN_POINT('Ctrl Pts',(-9.308873897103,0.854313999708652,26.4));
#34189=CARTESIAN_POINT('Ctrl Pts',(-9.30098819653116,0.862806231809669,
26.4));
#34190=CARTESIAN_POINT('Ctrl Pts',(-9.29297177630242,0.87118630014213,26.4));
#34191=CARTESIAN_POINT('Ctrl Pts',(-9.28554412806376,0.878950888077058,
26.4));
#34192=CARTESIAN_POINT('Ctrl Pts',(-9.27800996416404,0.886613143777747,
26.4));
#34193=CARTESIAN_POINT('Ctrl Pts',(-9.27037587193287,0.894167881801814,
26.4));
#34194=CARTESIAN_POINT('Ctrl Pts',(-9.23471789561382,0.929455203647225,
26.4));
#34195=CARTESIAN_POINT('Ctrl Pts',(-9.19685797580996,0.96242564884392,26.4));
#34196=CARTESIAN_POINT('Ctrl Pts',(-9.15706745972836,0.992923692890463,
26.4));
#34197=CARTESIAN_POINT('Ctrl Pts',(-9.13481966941932,1.00997584892161,26.4));
#34198=CARTESIAN_POINT('Ctrl Pts',(-9.11196751471993,1.02625459198139,26.4));
#34199=CARTESIAN_POINT('Ctrl Pts',(-9.08855308253825,1.04172812665066,26.4));
#34200=CARTESIAN_POINT('Ctrl Pts',(-9.07636573164392,1.04978219326764,26.4));
#34201=CARTESIAN_POINT('Ctrl Pts',(-9.06402375646026,1.0576191787653,26.4));
#34202=CARTESIAN_POINT('Ctrl Pts',(-9.05155319600525,1.06522240020876,26.4));
#34203=CARTESIAN_POINT('Ctrl Pts',(-9.0059932331111,1.09300001999494,26.4));
#34204=CARTESIAN_POINT('Ctrl Pts',(-8.95866615983379,1.11769846015436,26.4));
#34205=CARTESIAN_POINT('Ctrl Pts',(-8.90987125549013,1.13911717768622,26.4));
#34206=CARTESIAN_POINT('Ctrl Pts',(-8.87875607920242,1.15277530819852,26.4));
#34207=CARTESIAN_POINT('Ctrl Pts',(-8.84704308031516,1.16509898830357,26.4));
#34208=CARTESIAN_POINT('Ctrl Pts',(-8.81482194563461,1.17607986114086,26.4));
#34209=CARTESIAN_POINT('Ctrl Pts',(-9.55005314880761,-1.91003690738122E-5,
25.4658930328476));
#34210=CARTESIAN_POINT('Ctrl Pts',(-9.55009383677427,-0.0583092511807032,
25.4685430772439));
#34211=CARTESIAN_POINT('Ctrl Pts',(-9.5453163970275,-0.116592801535466,
25.4711931216402));
#34212=CARTESIAN_POINT('Ctrl Pts',(-9.53565891265265,-0.174056195750679,
25.4738431660365));
#34213=CARTESIAN_POINT('Ctrl Pts',(-9.50753251231398,-0.34141224498499,
25.4815611396529));
#34214=CARTESIAN_POINT('Ctrl Pts',(-9.43801338171337,-0.50181169762144,
25.4892791132692));
#34215=CARTESIAN_POINT('Ctrl Pts',(-9.33511669832289,-0.636761370259148,
25.4969970868856));
#34216=CARTESIAN_POINT('Ctrl Pts',(-9.23222001493242,-0.771711042896858,
25.504715060502));
#34217=CARTESIAN_POINT('Ctrl Pts',(-9.09594577875207,-0.881210935535826,
25.5124330341183));
#34218=CARTESIAN_POINT('Ctrl Pts',(-8.94200566715974,-0.952636306651832,
25.5201510077347));
#34219=CARTESIAN_POINT('Ctrl Pts',(-8.78806555556741,-1.02406167776784,
25.527868981351));
#34220=CARTESIAN_POINT('Ctrl Pts',(-8.61645956856308,-1.05741252736088,
25.5355869549674));
#34221=CARTESIAN_POINT('Ctrl Pts',(-8.4469729421721,-1.048843684092,25.5433049285838));
#34222=CARTESIAN_POINT('Ctrl Pts',(-8.27748631578111,-1.04027484082311,
25.5510229022001));
#34223=CARTESIAN_POINT('Ctrl Pts',(-8.11011905000345,-0.989786304692296,
25.5587408758165));
#34224=CARTESIAN_POINT('Ctrl Pts',(-7.96416767931932,-0.903199129009522,
25.5664588494329));
#34225=CARTESIAN_POINT('Ctrl Pts',(-7.81821630863519,-0.816611953326749,
25.5741768230492));
#34226=CARTESIAN_POINT('Ctrl Pts',(-7.69368083304458,-0.693926138092018,
25.5818947966656));
#34227=CARTESIAN_POINT('Ctrl Pts',(-7.60491951484999,-0.54928668983791,
25.589612770282));
#34228=CARTESIAN_POINT('Ctrl Pts',(-7.51615819665539,-0.404647241583803,
25.5973307438983));
#34229=CARTESIAN_POINT('Ctrl Pts',(-7.46317103585682,-0.23805416031032,
25.6050487175147));
#34230=CARTESIAN_POINT('Ctrl Pts',(-7.45206716359754,-0.0687147212564117,
25.612766691131));
#34231=CARTESIAN_POINT('Ctrl Pts',(-7.44096329133826,0.100624717797497,
25.6204846647474));
#34232=CARTESIAN_POINT('Ctrl Pts',(-7.47174270761827,0.272710514631827,
25.6282026383638));
#34233=CARTESIAN_POINT('Ctrl Pts',(-7.54085671332326,0.427702113803672,
25.6359206119801));
#34234=CARTESIAN_POINT('Ctrl Pts',(-7.60997071902825,0.582693712975518,
25.6436385855965));
#34235=CARTESIAN_POINT('Ctrl Pts',(-7.71741931415822,0.72059111448488,25.6513565592129));
#34236=CARTESIAN_POINT('Ctrl Pts',(-7.85081426070553,0.825495498730995,
25.6590745328292));
#34237=CARTESIAN_POINT('Ctrl Pts',(-7.98420920725284,0.930399882977112,
25.6667925064456));
#34238=CARTESIAN_POINT('Ctrl Pts',(-8.14355050521749,1.00231124995999,25.6745104800619));
#34239=CARTESIAN_POINT('Ctrl Pts',(-8.31046697048996,1.03293861059286,25.6822284536783));
#34240=CARTESIAN_POINT('Ctrl Pts',(-8.47738343576243,1.06356597122573,25.6899464272947));
#34241=CARTESIAN_POINT('Ctrl Pts',(-8.65187506834272,1.05290932550861,25.697664400911));
#34242=CARTESIAN_POINT('Ctrl Pts',(-8.81382393302662,1.00219732667193,25.7053823745274));
#34243=CARTESIAN_POINT('Ctrl Pts',(-8.97577279771052,0.951485327835256,
25.7131003481437));
#34244=CARTESIAN_POINT('Ctrl Pts',(-9.12517889449803,0.860717975879029,
25.7208183217601));
#34245=CARTESIAN_POINT('Ctrl Pts',(-9.2448165138821,0.740360252294236,25.7285362953765));
#34246=CARTESIAN_POINT('Ctrl Pts',(-9.36445413326617,0.620002528709445,
25.7362542689928));
#34247=CARTESIAN_POINT('Ctrl Pts',(-9.45432327524679,0.470054433496088,
25.7439722426092));
#34248=CARTESIAN_POINT('Ctrl Pts',(-9.5040625170527,0.307804165628874,25.7516902162256));
#34249=CARTESIAN_POINT('Ctrl Pts',(-9.53457300099597,0.208278438801921,
25.7564244884329));
#34250=CARTESIAN_POINT('Ctrl Pts',(-9.54998379775559,0.104123770513768,
25.7611587606403));
#34251=CARTESIAN_POINT('Ctrl Pts',(-9.55003919466624,-1.48519393190782E-5,
25.7658930328476));
#34252=CARTESIAN_POINT('Ctrl Pts',(-8.8147888955044,1.17604951161383,25.2));
#34253=CARTESIAN_POINT('Ctrl Pts',(-8.86280020341074,1.15963879009472,25.2));
#34254=CARTESIAN_POINT('Ctrl Pts',(-8.90960731244362,1.14022121906871,25.2));
#34255=CARTESIAN_POINT('Ctrl Pts',(-8.95497238860795,1.11798779738799,25.2));
#34256=CARTESIAN_POINT('Ctrl Pts',(-9.00031600398345,1.09576489363885,25.2));
#34257=CARTESIAN_POINT('Ctrl Pts',(-9.04421984864658,1.07072810229581,25.2));
#34258=CARTESIAN_POINT('Ctrl Pts',(-9.08641918731652,1.04302391286584,25.2));
#34259=CARTESIAN_POINT('Ctrl Pts',(-9.12519792826817,1.01756537206777,25.2));
#34260=CARTESIAN_POINT('Ctrl Pts',(-9.1625375171365,0.989853465475151,25.2));
#34261=CARTESIAN_POINT('Ctrl Pts',(-9.19820248282102,0.959976338255365,
25.2));
#34262=CARTESIAN_POINT('Ctrl Pts',(-9.2052982498248,0.954032097754221,25.2));
#34263=CARTESIAN_POINT('Ctrl Pts',(-9.21232927057154,0.948000630658807,
25.2));
#34264=CARTESIAN_POINT('Ctrl Pts',(-9.21928818410342,0.94188724537333,25.2));
#34265=CARTESIAN_POINT('Ctrl Pts',(-9.24730637906229,0.917273342642342,
25.2));
#34266=CARTESIAN_POINT('Ctrl Pts',(-9.27408704155894,0.891394738150684,
25.2));
#34267=CARTESIAN_POINT('Ctrl Pts',(-9.29952872082846,0.864315792473915,
25.2));
#34268=CARTESIAN_POINT('Ctrl Pts',(-9.33347315480174,0.828186908297136,
25.2));
#34269=CARTESIAN_POINT('Ctrl Pts',(-9.36503600501172,0.789921886846104,
25.2));
#34270=CARTESIAN_POINT('Ctrl Pts',(-9.39406748567017,0.749786961749021,
25.2));
#34271=CARTESIAN_POINT('Ctrl Pts',(-9.41426272810871,0.72186780212627,25.2));
#34272=CARTESIAN_POINT('Ctrl Pts',(-9.4332321752929,0.693043058821335,25.2));
#34273=CARTESIAN_POINT('Ctrl Pts',(-9.4509116976612,0.663396605844021,25.2));
#34274=CARTESIAN_POINT('Ctrl Pts',(-9.46034256416092,0.647582166155294,
25.2));
#34275=CARTESIAN_POINT('Ctrl Pts',(-9.4694061787729,0.631533848303631,25.2));
#34276=CARTESIAN_POINT('Ctrl Pts',(-9.47809135764204,0.615264128747603,
25.2));
#34277=CARTESIAN_POINT('Ctrl Pts',(-9.48251070130078,0.606985487278882,
25.2));
#34278=CARTESIAN_POINT('Ctrl Pts',(-9.48683204540646,0.598649519784842,
25.2));
#34279=CARTESIAN_POINT('Ctrl Pts',(-9.4910538103519,0.590257864458163,25.2));
#34280=CARTESIAN_POINT('Ctrl Pts',(-9.49557618446465,0.581268684505481,
25.2));
#34281=CARTESIAN_POINT('Ctrl Pts',(-9.4999809236823,0.572222148823553,25.2));
#34282=CARTESIAN_POINT('Ctrl Pts',(-9.50426329374563,0.563127845164782,
25.2));
#34283=CARTESIAN_POINT('Ctrl Pts',(-9.52493457020396,0.519229054928066,
25.2));
#34284=CARTESIAN_POINT('Ctrl Pts',(-9.54278509116266,0.474165957397592,
25.2));
#34285=CARTESIAN_POINT('Ctrl Pts',(-9.55766734967247,0.42818600198001,25.2));
#34286=CARTESIAN_POINT('Ctrl Pts',(-9.5629783230983,0.411777315006687,25.2));
#34287=CARTESIAN_POINT('Ctrl Pts',(-9.56791082232496,0.395251712842571,
25.2));
#34288=CARTESIAN_POINT('Ctrl Pts',(-9.57245656795131,0.378620075217546,
25.2));
#34289=CARTESIAN_POINT('Ctrl Pts',(-9.58437744649104,0.335004847190819,
25.2));
#34290=CARTESIAN_POINT('Ctrl Pts',(-9.59364135084807,0.290660092434833,
25.2));
#34291=CARTESIAN_POINT('Ctrl Pts',(-9.60021807317259,0.245833089310576,
25.2));
#34292=CARTESIAN_POINT('Ctrl Pts',(-9.60298169195186,0.226996236918194,
25.2));
#34293=CARTESIAN_POINT('Ctrl Pts',(-9.60527033726867,0.208074278886572,
25.2));
#34294=CARTESIAN_POINT('Ctrl Pts',(-9.60707970804988,0.189086003575891,
25.2));
#34295=CARTESIAN_POINT('Ctrl Pts',(-9.60796960254794,0.179747087582501,
25.2));
#34296=CARTESIAN_POINT('Ctrl Pts',(-9.60874368108558,0.170390165094709,
25.2));
#34297=CARTESIAN_POINT('Ctrl Pts',(-9.60940089380497,0.161023774009816,
25.2));
#34298=CARTESIAN_POINT('Ctrl Pts',(-9.61273692395369,0.11347971084424,25.2));
#34299=CARTESIAN_POINT('Ctrl Pts',(-9.61305418040214,0.0658793756383451,
25.2));
#34300=CARTESIAN_POINT('Ctrl Pts',(-9.61035533089854,0.0185116756316162,
25.2));
#34301=CARTESIAN_POINT('Ctrl Pts',(-9.60768706096201,-0.0283193202137848,
25.2));
#34302=CARTESIAN_POINT('Ctrl Pts',(-9.602070465873,-0.0749239959345515,
25.2));
#34303=CARTESIAN_POINT('Ctrl Pts',(-9.59345865066658,-0.121014087532771,
25.2));
#34304=CARTESIAN_POINT('Ctrl Pts',(-9.59107676135001,-0.133761864179878,
25.2));
#34305=CARTESIAN_POINT('Ctrl Pts',(-9.58846545612991,-0.146470169922223,
25.2));
#34306=CARTESIAN_POINT('Ctrl Pts',(-9.5856230906601,-0.159132614503963,
25.2));
#34307=CARTESIAN_POINT('Ctrl Pts',(-9.58068437982785,-0.181134061145071,
25.2));
#34308=CARTESIAN_POINT('Ctrl Pts',(-9.57504819570294,-0.20299714950449,
25.2));
#34309=CARTESIAN_POINT('Ctrl Pts',(-9.56872448240039,-0.224690074400913,
25.2));
#34310=CARTESIAN_POINT('Ctrl Pts',(-9.56551448953387,-0.235701663769357,
25.2));
#34311=CARTESIAN_POINT('Ctrl Pts',(-9.56212730755587,-0.246669380680947,
25.2));
#34312=CARTESIAN_POINT('Ctrl Pts',(-9.55856403963841,-0.257588884414899,
25.2));
#34313=CARTESIAN_POINT('Ctrl Pts',(-9.55533547929827,-0.267482689064466,
25.2));
#34314=CARTESIAN_POINT('Ctrl Pts',(-9.55196496076087,-0.277328804982544,
25.2));
#34315=CARTESIAN_POINT('Ctrl Pts',(-9.5484554570926,-0.287120191330713,
25.2));
#34316=CARTESIAN_POINT('Ctrl Pts',(-9.5326807598597,-0.331131017285632,
25.2));
#34317=CARTESIAN_POINT('Ctrl Pts',(-9.5140926598038,-0.374065502137421,
25.2));
#34318=CARTESIAN_POINT('Ctrl Pts',(-9.49280985332475,-0.415649037346325,
25.2));
#34319=CARTESIAN_POINT('Ctrl Pts',(-9.48095747832615,-0.438806869164606,
25.2));
#34320=CARTESIAN_POINT('Ctrl Pts',(-9.46826858540731,-0.461545246835699,
25.2));
#34321=CARTESIAN_POINT('Ctrl Pts',(-9.45475837707871,-0.483812065291647,
25.2));
#34322=CARTESIAN_POINT('Ctrl Pts',(-9.44902464840965,-0.493262096871042,
25.2));
#34323=CARTESIAN_POINT('Ctrl Pts',(-9.44314352445654,-0.502625949871307,
25.2));
#34324=CARTESIAN_POINT('Ctrl Pts',(-9.43712301779533,-0.511889514393272,
25.2));
#34325=CARTESIAN_POINT('Ctrl Pts',(-9.41182994658654,-0.550807168718137,
25.2));
#34326=CARTESIAN_POINT('Ctrl Pts',(-9.38404978263737,-0.588008170344988,
25.2));
#34327=CARTESIAN_POINT('Ctrl Pts',(-9.35388387934858,-0.623205306360306,
25.2));
#34328=CARTESIAN_POINT('Ctrl Pts',(-9.33467724557846,-0.645615326532135,
25.2));
#34329=CARTESIAN_POINT('Ctrl Pts',(-9.3145025679876,-0.667212233621307,
25.2));
#34330=CARTESIAN_POINT('Ctrl Pts',(-9.29341958724169,-0.68794182840578,
25.2));
#34331=CARTESIAN_POINT('Origin',(-8.5,0.,26.4));
#34332=CARTESIAN_POINT('',(-7.46076951545867,-1.8,26.4));
#34333=CARTESIAN_POINT('',(-6.42153903091735,0.,26.4));
#34334=CARTESIAN_POINT('',(-7.46076951545867,-1.8,26.4));
#34335=CARTESIAN_POINT('',(-7.46076951545867,1.8,26.4));
#34336=CARTESIAN_POINT('',(-6.42153903091735,0.,26.4));
#34337=CARTESIAN_POINT('',(-9.53923048454133,1.8,26.4));
#34338=CARTESIAN_POINT('',(-7.46076951545867,1.8,26.4));
#34339=CARTESIAN_POINT('',(-10.5784609690827,2.22044604925031E-16,26.4));
#34340=CARTESIAN_POINT('',(-9.53923048454133,1.8,26.4));
#34341=CARTESIAN_POINT('',(-9.53923048454133,-1.8,26.4));
#34342=CARTESIAN_POINT('',(-10.5784609690827,2.54538057293978E-16,26.4));
#34343=CARTESIAN_POINT('',(-9.53923048454133,-1.8,26.4));
#34344=CARTESIAN_POINT('Origin',(-8.5,0.,25.1));
#34345=CARTESIAN_POINT('Origin',(-9.53923048454133,-1.8,25.2));
#34346=CARTESIAN_POINT('',(-9.53923048454133,-1.8,25.2));
#34347=CARTESIAN_POINT('',(-7.46076951545867,-1.8,25.2));
#34348=CARTESIAN_POINT('',(-9.53923048454133,-1.8,25.2));
#34349=CARTESIAN_POINT('',(-7.46076951545867,-1.8,25.2));
#34350=CARTESIAN_POINT('',(-9.53923048454133,-1.8,25.2));
#34351=CARTESIAN_POINT('Origin',(-10.5784609690827,2.54538057293978E-16,
25.2));
#34352=CARTESIAN_POINT('',(-10.5784609690827,2.54538057293978E-16,25.2));
#34353=CARTESIAN_POINT('',(-10.5784609690827,2.54538057293978E-16,25.2));
#34354=CARTESIAN_POINT('',(-10.5784609690827,2.54538057293978E-16,25.2));
#34355=CARTESIAN_POINT('Origin',(-9.53923048454133,1.8,25.2));
#34356=CARTESIAN_POINT('',(-9.53923048454133,1.8,25.2));
#34357=CARTESIAN_POINT('',(-9.53923048454133,1.8,25.2));
#34358=CARTESIAN_POINT('',(-9.53923048454133,1.8,25.2));
#34359=CARTESIAN_POINT('Origin',(-7.46076951545867,1.8,25.2));
#34360=CARTESIAN_POINT('',(-7.46076951545867,1.8,25.2));
#34361=CARTESIAN_POINT('',(-7.46076951545867,1.8,25.2));
#34362=CARTESIAN_POINT('',(-7.46076951545867,1.8,25.2));
#34363=CARTESIAN_POINT('Origin',(-6.42153903091735,0.,25.2));
#34364=CARTESIAN_POINT('',(-6.42153903091735,0.,25.2));
#34365=CARTESIAN_POINT('',(-6.42153903091735,0.,25.2));
#34366=CARTESIAN_POINT('',(-6.42153903091735,0.,25.2));
#34367=CARTESIAN_POINT('Origin',(-7.46076951545867,-1.8,25.2));
#34368=CARTESIAN_POINT('',(-7.46076951545867,-1.8,25.2));
#34369=CARTESIAN_POINT('Origin',(-8.5,0.,25.2));
#34370=CARTESIAN_POINT('',(0.,0.,0.));
#34371=CARTESIAN_POINT('',(0.,0.,0.));
#34372=CARTESIAN_POINT('',(0.,0.,0.));
#34373=CARTESIAN_POINT('',(0.,0.,0.));
#34374=CARTESIAN_POINT('',(0.,0.,0.));
#34375=CARTESIAN_POINT('',(0.,0.,0.));
#34376=UNCERTAINTY_MEASURE_WITH_UNIT(LENGTH_MEASURE(0.001),#34434,
'DISTANCE_ACCURACY_VALUE',
'Maximum model space distance between geometric entities at asserted c
onnectivities');
#34377=UNCERTAINTY_MEASURE_WITH_UNIT(LENGTH_MEASURE(0.001),#34434,
'DISTANCE_ACCURACY_VALUE',
'Maximum model space distance between geometric entities at asserted c
onnectivities');
#34378=UNCERTAINTY_MEASURE_WITH_UNIT(LENGTH_MEASURE(0.001),#34434,
'DISTANCE_ACCURACY_VALUE',
'Maximum model space distance between geometric entities at asserted c
onnectivities');
#34379=UNCERTAINTY_MEASURE_WITH_UNIT(LENGTH_MEASURE(0.001),#34434,
'DISTANCE_ACCURACY_VALUE',
'Maximum model space distance between geometric entities at asserted c
onnectivities');
#34380=UNCERTAINTY_MEASURE_WITH_UNIT(LENGTH_MEASURE(0.001),#34434,
'DISTANCE_ACCURACY_VALUE',
'Maximum model space distance between geometric entities at asserted c
onnectivities');
#34381=UNCERTAINTY_MEASURE_WITH_UNIT(LENGTH_MEASURE(0.001),#34434,
'DISTANCE_ACCURACY_VALUE',
'Maximum model space distance between geometric entities at asserted c
onnectivities');
#34382=UNCERTAINTY_MEASURE_WITH_UNIT(LENGTH_MEASURE(0.001),#34434,
'DISTANCE_ACCURACY_VALUE',
'Maximum model space distance between geometric entities at asserted c
onnectivities');
#34383=UNCERTAINTY_MEASURE_WITH_UNIT(LENGTH_MEASURE(0.001),#34434,
'DISTANCE_ACCURACY_VALUE',
'Maximum model space distance between geometric entities at asserted c
onnectivities');
#34384=UNCERTAINTY_MEASURE_WITH_UNIT(LENGTH_MEASURE(0.001),#34434,
'DISTANCE_ACCURACY_VALUE',
'Maximum model space distance between geometric entities at asserted c
onnectivities');
#34385=UNCERTAINTY_MEASURE_WITH_UNIT(LENGTH_MEASURE(0.001),#34434,
'DISTANCE_ACCURACY_VALUE',
'Maximum model space distance between geometric entities at asserted c
onnectivities');
#34386=UNCERTAINTY_MEASURE_WITH_UNIT(LENGTH_MEASURE(0.001),#34434,
'DISTANCE_ACCURACY_VALUE',
'Maximum model space distance between geometric entities at asserted c
onnectivities');
#34387=UNCERTAINTY_MEASURE_WITH_UNIT(LENGTH_MEASURE(0.001),#34434,
'DISTANCE_ACCURACY_VALUE',
'Maximum model space distance between geometric entities at asserted c
onnectivities');
#34388=UNCERTAINTY_MEASURE_WITH_UNIT(LENGTH_MEASURE(0.001),#34434,
'DISTANCE_ACCURACY_VALUE',
'Maximum model space distance between geometric entities at asserted c
onnectivities');
#34389=UNCERTAINTY_MEASURE_WITH_UNIT(LENGTH_MEASURE(0.001),#34434,
'DISTANCE_ACCURACY_VALUE',
'Maximum model space distance between geometric entities at asserted c
onnectivities');
#34390=UNCERTAINTY_MEASURE_WITH_UNIT(LENGTH_MEASURE(0.001),#34434,
'DISTANCE_ACCURACY_VALUE',
'Maximum model space distance between geometric entities at asserted c
onnectivities');
#34391=UNCERTAINTY_MEASURE_WITH_UNIT(LENGTH_MEASURE(0.001),#34434,
'DISTANCE_ACCURACY_VALUE',
'Maximum model space distance between geometric entities at asserted c
onnectivities');
#34392=UNCERTAINTY_MEASURE_WITH_UNIT(LENGTH_MEASURE(0.001),#34434,
'DISTANCE_ACCURACY_VALUE',
'Maximum model space distance between geometric entities at asserted c
onnectivities');
#34393=UNCERTAINTY_MEASURE_WITH_UNIT(LENGTH_MEASURE(0.001),#34434,
'DISTANCE_ACCURACY_VALUE',
'Maximum model space distance between geometric entities at asserted c
onnectivities');
#34394=UNCERTAINTY_MEASURE_WITH_UNIT(LENGTH_MEASURE(0.001),#34434,
'DISTANCE_ACCURACY_VALUE',
'Maximum model space distance between geometric entities at asserted c
onnectivities');
#34395=UNCERTAINTY_MEASURE_WITH_UNIT(LENGTH_MEASURE(0.001),#34434,
'DISTANCE_ACCURACY_VALUE',
'Maximum model space distance between geometric entities at asserted c
onnectivities');
#34396=UNCERTAINTY_MEASURE_WITH_UNIT(LENGTH_MEASURE(0.001),#34434,
'DISTANCE_ACCURACY_VALUE',
'Maximum model space distance between geometric entities at asserted c
onnectivities');
#34397=UNCERTAINTY_MEASURE_WITH_UNIT(LENGTH_MEASURE(0.001),#34434,
'DISTANCE_ACCURACY_VALUE',
'Maximum model space distance between geometric entities at asserted c
onnectivities');
#34398=UNCERTAINTY_MEASURE_WITH_UNIT(LENGTH_MEASURE(0.001),#34434,
'DISTANCE_ACCURACY_VALUE',
'Maximum model space distance between geometric entities at asserted c
onnectivities');
#34399=UNCERTAINTY_MEASURE_WITH_UNIT(LENGTH_MEASURE(0.001),#34434,
'DISTANCE_ACCURACY_VALUE',
'Maximum model space distance between geometric entities at asserted c
onnectivities');
#34400=UNCERTAINTY_MEASURE_WITH_UNIT(LENGTH_MEASURE(0.001),#34434,
'DISTANCE_ACCURACY_VALUE',
'Maximum model space distance between geometric entities at asserted c
onnectivities');
#34401=UNCERTAINTY_MEASURE_WITH_UNIT(LENGTH_MEASURE(0.001),#34434,
'DISTANCE_ACCURACY_VALUE',
'Maximum model space distance between geometric entities at asserted c
onnectivities');
#34402=UNCERTAINTY_MEASURE_WITH_UNIT(LENGTH_MEASURE(0.001),#34434,
'DISTANCE_ACCURACY_VALUE',
'Maximum model space distance between geometric entities at asserted c
onnectivities');
#34403=UNCERTAINTY_MEASURE_WITH_UNIT(LENGTH_MEASURE(0.001),#34434,
'DISTANCE_ACCURACY_VALUE',
'Maximum model space distance between geometric entities at asserted c
onnectivities');
#34404=UNCERTAINTY_MEASURE_WITH_UNIT(LENGTH_MEASURE(0.001),#34434,
'DISTANCE_ACCURACY_VALUE',
'Maximum model space distance between geometric entities at asserted c
onnectivities');
#34405=(
GEOMETRIC_REPRESENTATION_CONTEXT(3)
GLOBAL_UNCERTAINTY_ASSIGNED_CONTEXT((#34376))
GLOBAL_UNIT_ASSIGNED_CONTEXT((#34434,#34436,#34437))
REPRESENTATION_CONTEXT('','3D')
);
#34406=(
GEOMETRIC_REPRESENTATION_CONTEXT(3)
GLOBAL_UNCERTAINTY_ASSIGNED_CONTEXT((#34377))
GLOBAL_UNIT_ASSIGNED_CONTEXT((#34434,#34436,#34437))
REPRESENTATION_CONTEXT('','3D')
);
#34407=(
GEOMETRIC_REPRESENTATION_CONTEXT(3)
GLOBAL_UNCERTAINTY_ASSIGNED_CONTEXT((#34378))
GLOBAL_UNIT_ASSIGNED_CONTEXT((#34434,#34436,#34437))
REPRESENTATION_CONTEXT('','3D')
);
#34408=(
GEOMETRIC_REPRESENTATION_CONTEXT(3)
GLOBAL_UNCERTAINTY_ASSIGNED_CONTEXT((#34379))
GLOBAL_UNIT_ASSIGNED_CONTEXT((#34434,#34436,#34437))
REPRESENTATION_CONTEXT('','3D')
);
#34409=(
GEOMETRIC_REPRESENTATION_CONTEXT(3)
GLOBAL_UNCERTAINTY_ASSIGNED_CONTEXT((#34380))
GLOBAL_UNIT_ASSIGNED_CONTEXT((#34434,#34436,#34437))
REPRESENTATION_CONTEXT('','3D')
);
#34410=(
GEOMETRIC_REPRESENTATION_CONTEXT(3)
GLOBAL_UNCERTAINTY_ASSIGNED_CONTEXT((#34381))
GLOBAL_UNIT_ASSIGNED_CONTEXT((#34434,#34436,#34437))
REPRESENTATION_CONTEXT('','3D')
);
#34411=(
GEOMETRIC_REPRESENTATION_CONTEXT(3)
GLOBAL_UNCERTAINTY_ASSIGNED_CONTEXT((#34382))
GLOBAL_UNIT_ASSIGNED_CONTEXT((#34434,#34436,#34437))
REPRESENTATION_CONTEXT('','3D')
);
#34412=(
GEOMETRIC_REPRESENTATION_CONTEXT(3)
GLOBAL_UNCERTAINTY_ASSIGNED_CONTEXT((#34383))
GLOBAL_UNIT_ASSIGNED_CONTEXT((#34434,#34436,#34437))
REPRESENTATION_CONTEXT('','3D')
);
#34413=(
GEOMETRIC_REPRESENTATION_CONTEXT(3)
GLOBAL_UNCERTAINTY_ASSIGNED_CONTEXT((#34384))
GLOBAL_UNIT_ASSIGNED_CONTEXT((#34434,#34436,#34437))
REPRESENTATION_CONTEXT('','3D')
);
#34414=(
GEOMETRIC_REPRESENTATION_CONTEXT(3)
GLOBAL_UNCERTAINTY_ASSIGNED_CONTEXT((#34385))
GLOBAL_UNIT_ASSIGNED_CONTEXT((#34434,#34436,#34437))
REPRESENTATION_CONTEXT('','3D')
);
#34415=(
GEOMETRIC_REPRESENTATION_CONTEXT(3)
GLOBAL_UNCERTAINTY_ASSIGNED_CONTEXT((#34386))
GLOBAL_UNIT_ASSIGNED_CONTEXT((#34434,#34436,#34437))
REPRESENTATION_CONTEXT('','3D')
);
#34416=(
GEOMETRIC_REPRESENTATION_CONTEXT(3)
GLOBAL_UNCERTAINTY_ASSIGNED_CONTEXT((#34387))
GLOBAL_UNIT_ASSIGNED_CONTEXT((#34434,#34436,#34437))
REPRESENTATION_CONTEXT('','3D')
);
#34417=(
GEOMETRIC_REPRESENTATION_CONTEXT(3)
GLOBAL_UNCERTAINTY_ASSIGNED_CONTEXT((#34388))
GLOBAL_UNIT_ASSIGNED_CONTEXT((#34434,#34436,#34437))
REPRESENTATION_CONTEXT('','3D')
);
#34418=(
GEOMETRIC_REPRESENTATION_CONTEXT(3)
GLOBAL_UNCERTAINTY_ASSIGNED_CONTEXT((#34389))
GLOBAL_UNIT_ASSIGNED_CONTEXT((#34434,#34436,#34437))
REPRESENTATION_CONTEXT('','3D')
);
#34419=(
GEOMETRIC_REPRESENTATION_CONTEXT(3)
GLOBAL_UNCERTAINTY_ASSIGNED_CONTEXT((#34390))
GLOBAL_UNIT_ASSIGNED_CONTEXT((#34434,#34436,#34437))
REPRESENTATION_CONTEXT('','3D')
);
#34420=(
GEOMETRIC_REPRESENTATION_CONTEXT(3)
GLOBAL_UNCERTAINTY_ASSIGNED_CONTEXT((#34391))
GLOBAL_UNIT_ASSIGNED_CONTEXT((#34434,#34436,#34437))
REPRESENTATION_CONTEXT('','3D')
);
#34421=(
GEOMETRIC_REPRESENTATION_CONTEXT(3)
GLOBAL_UNCERTAINTY_ASSIGNED_CONTEXT((#34392))
GLOBAL_UNIT_ASSIGNED_CONTEXT((#34434,#34436,#34437))
REPRESENTATION_CONTEXT('','3D')
);
#34422=(
GEOMETRIC_REPRESENTATION_CONTEXT(3)
GLOBAL_UNCERTAINTY_ASSIGNED_CONTEXT((#34393))
GLOBAL_UNIT_ASSIGNED_CONTEXT((#34434,#34436,#34437))
REPRESENTATION_CONTEXT('','3D')
);
#34423=(
GEOMETRIC_REPRESENTATION_CONTEXT(3)
GLOBAL_UNCERTAINTY_ASSIGNED_CONTEXT((#34394))
GLOBAL_UNIT_ASSIGNED_CONTEXT((#34434,#34436,#34437))
REPRESENTATION_CONTEXT('','3D')
);
#34424=(
GEOMETRIC_REPRESENTATION_CONTEXT(3)
GLOBAL_UNCERTAINTY_ASSIGNED_CONTEXT((#34395))
GLOBAL_UNIT_ASSIGNED_CONTEXT((#34434,#34436,#34437))
REPRESENTATION_CONTEXT('','3D')
);
#34425=(
GEOMETRIC_REPRESENTATION_CONTEXT(3)
GLOBAL_UNCERTAINTY_ASSIGNED_CONTEXT((#34396))
GLOBAL_UNIT_ASSIGNED_CONTEXT((#34434,#34436,#34437))
REPRESENTATION_CONTEXT('','3D')
);
#34426=(
GEOMETRIC_REPRESENTATION_CONTEXT(3)
GLOBAL_UNCERTAINTY_ASSIGNED_CONTEXT((#34397))
GLOBAL_UNIT_ASSIGNED_CONTEXT((#34434,#34436,#34437))
REPRESENTATION_CONTEXT('','3D')
);
#34427=(
GEOMETRIC_REPRESENTATION_CONTEXT(3)
GLOBAL_UNCERTAINTY_ASSIGNED_CONTEXT((#34398))
GLOBAL_UNIT_ASSIGNED_CONTEXT((#34434,#34436,#34437))
REPRESENTATION_CONTEXT('','3D')
);
#34428=(
GEOMETRIC_REPRESENTATION_CONTEXT(3)
GLOBAL_UNCERTAINTY_ASSIGNED_CONTEXT((#34399))
GLOBAL_UNIT_ASSIGNED_CONTEXT((#34434,#34436,#34437))
REPRESENTATION_CONTEXT('','3D')
);
#34429=(
GEOMETRIC_REPRESENTATION_CONTEXT(3)
GLOBAL_UNCERTAINTY_ASSIGNED_CONTEXT((#34400))
GLOBAL_UNIT_ASSIGNED_CONTEXT((#34434,#34436,#34437))
REPRESENTATION_CONTEXT('','3D')
);
#34430=(
GEOMETRIC_REPRESENTATION_CONTEXT(3)
GLOBAL_UNCERTAINTY_ASSIGNED_CONTEXT((#34401))
GLOBAL_UNIT_ASSIGNED_CONTEXT((#34434,#34436,#34437))
REPRESENTATION_CONTEXT('','3D')
);
#34431=(
GEOMETRIC_REPRESENTATION_CONTEXT(3)
GLOBAL_UNCERTAINTY_ASSIGNED_CONTEXT((#34402))
GLOBAL_UNIT_ASSIGNED_CONTEXT((#34434,#34436,#34437))
REPRESENTATION_CONTEXT('','3D')
);
#34432=(
GEOMETRIC_REPRESENTATION_CONTEXT(3)
GLOBAL_UNCERTAINTY_ASSIGNED_CONTEXT((#34403))
GLOBAL_UNIT_ASSIGNED_CONTEXT((#34434,#34436,#34437))
REPRESENTATION_CONTEXT('','3D')
);
#34433=(
GEOMETRIC_REPRESENTATION_CONTEXT(3)
GLOBAL_UNCERTAINTY_ASSIGNED_CONTEXT((#34404))
GLOBAL_UNIT_ASSIGNED_CONTEXT((#34434,#34436,#34437))
REPRESENTATION_CONTEXT('','3D')
);
#34434=(
LENGTH_UNIT()
NAMED_UNIT(*)
SI_UNIT(.CENTI.,.METRE.)
);
#34435=(
LENGTH_UNIT()
NAMED_UNIT(*)
SI_UNIT($,.METRE.)
);
#34436=(
NAMED_UNIT(*)
PLANE_ANGLE_UNIT()
SI_UNIT($,.RADIAN.)
);
#34437=(
NAMED_UNIT(*)
SI_UNIT($,.STERADIAN.)
SOLID_ANGLE_UNIT()
);
#34438=SHAPE_DEFINITION_REPRESENTATION(#34466,#34537);
#34439=SHAPE_DEFINITION_REPRESENTATION(#34467,#34538);
#34440=SHAPE_DEFINITION_REPRESENTATION(#34468,#34539);
#34441=SHAPE_DEFINITION_REPRESENTATION(#34469,#34540);
#34442=SHAPE_DEFINITION_REPRESENTATION(#34470,#34541);
#34443=SHAPE_DEFINITION_REPRESENTATION(#34471,#34542);
#34444=SHAPE_DEFINITION_REPRESENTATION(#34472,#34543);
#34445=SHAPE_DEFINITION_REPRESENTATION(#34473,#34544);
#34446=SHAPE_DEFINITION_REPRESENTATION(#34474,#34545);
#34447=SHAPE_DEFINITION_REPRESENTATION(#34475,#34546);
#34448=SHAPE_DEFINITION_REPRESENTATION(#34476,#34547);
#34449=SHAPE_DEFINITION_REPRESENTATION(#34477,#34548);
#34450=SHAPE_DEFINITION_REPRESENTATION(#34478,#34549);
#34451=SHAPE_DEFINITION_REPRESENTATION(#34479,#34550);
#34452=SHAPE_DEFINITION_REPRESENTATION(#34480,#34551);
#34453=SHAPE_DEFINITION_REPRESENTATION(#34481,#34552);
#34454=SHAPE_DEFINITION_REPRESENTATION(#34482,#34553);
#34455=SHAPE_DEFINITION_REPRESENTATION(#34483,#34554);
#34456=SHAPE_DEFINITION_REPRESENTATION(#34484,#34555);
#34457=SHAPE_DEFINITION_REPRESENTATION(#34485,#34556);
#34458=SHAPE_DEFINITION_REPRESENTATION(#34520,#34557);
#34459=SHAPE_DEFINITION_REPRESENTATION(#34521,#34558);
#34460=SHAPE_DEFINITION_REPRESENTATION(#34523,#34559);
#34461=SHAPE_DEFINITION_REPRESENTATION(#34524,#34560);
#34462=SHAPE_DEFINITION_REPRESENTATION(#34526,#34561);
#34463=SHAPE_DEFINITION_REPRESENTATION(#34527,#34562);
#34464=SHAPE_DEFINITION_REPRESENTATION(#34529,#34563);
#34465=SHAPE_DEFINITION_REPRESENTATION(#34530,#34564);
#34466=PRODUCT_DEFINITION_SHAPE('',$,#34566);
#34467=PRODUCT_DEFINITION_SHAPE('',$,#34567);
#34468=PRODUCT_DEFINITION_SHAPE('',$,#34568);
#34469=PRODUCT_DEFINITION_SHAPE('',$,#34569);
#34470=PRODUCT_DEFINITION_SHAPE('',$,#34570);
#34471=PRODUCT_DEFINITION_SHAPE('',$,#34571);
#34472=PRODUCT_DEFINITION_SHAPE('',$,#34572);
#34473=PRODUCT_DEFINITION_SHAPE('',$,#34573);
#34474=PRODUCT_DEFINITION_SHAPE('',$,#34574);
#34475=PRODUCT_DEFINITION_SHAPE('',$,#34575);
#34476=PRODUCT_DEFINITION_SHAPE('',$,#34576);
#34477=PRODUCT_DEFINITION_SHAPE('',$,#34577);
#34478=PRODUCT_DEFINITION_SHAPE('',$,#34578);
#34479=PRODUCT_DEFINITION_SHAPE('',$,#34579);
#34480=PRODUCT_DEFINITION_SHAPE('',$,#34580);
#34481=PRODUCT_DEFINITION_SHAPE('',$,#34581);
#34482=PRODUCT_DEFINITION_SHAPE('',$,#34582);
#34483=PRODUCT_DEFINITION_SHAPE('',$,#34583);
#34484=PRODUCT_DEFINITION_SHAPE('',$,#34584);
#34485=PRODUCT_DEFINITION_SHAPE('',$,#34585);
#34486=PRODUCT_DEFINITION_SHAPE($,$,#140);
#34487=PRODUCT_DEFINITION_SHAPE($,$,#141);
#34488=PRODUCT_DEFINITION_SHAPE($,$,#142);
#34489=PRODUCT_DEFINITION_SHAPE($,$,#143);
#34490=PRODUCT_DEFINITION_SHAPE($,$,#144);
#34491=PRODUCT_DEFINITION_SHAPE($,$,#145);
#34492=PRODUCT_DEFINITION_SHAPE($,$,#146);
#34493=PRODUCT_DEFINITION_SHAPE($,$,#147);
#34494=PRODUCT_DEFINITION_SHAPE($,$,#148);
#34495=PRODUCT_DEFINITION_SHAPE($,$,#149);
#34496=PRODUCT_DEFINITION_SHAPE($,$,#150);
#34497=PRODUCT_DEFINITION_SHAPE($,$,#151);
#34498=PRODUCT_DEFINITION_SHAPE($,$,#152);
#34499=PRODUCT_DEFINITION_SHAPE($,$,#153);
#34500=PRODUCT_DEFINITION_SHAPE($,$,#154);
#34501=PRODUCT_DEFINITION_SHAPE($,$,#155);
#34502=PRODUCT_DEFINITION_SHAPE($,$,#156);
#34503=PRODUCT_DEFINITION_SHAPE($,$,#157);
#34504=PRODUCT_DEFINITION_SHAPE($,$,#158);
#34505=PRODUCT_DEFINITION_SHAPE($,$,#159);
#34506=PRODUCT_DEFINITION_SHAPE($,$,#160);
#34507=PRODUCT_DEFINITION_SHAPE($,$,#161);
#34508=PRODUCT_DEFINITION_SHAPE($,$,#162);
#34509=PRODUCT_DEFINITION_SHAPE($,$,#163);
#34510=PRODUCT_DEFINITION_SHAPE($,$,#164);
#34511=PRODUCT_DEFINITION_SHAPE($,$,#165);
#34512=PRODUCT_DEFINITION_SHAPE($,$,#166);
#34513=PRODUCT_DEFINITION_SHAPE($,$,#167);
#34514=PRODUCT_DEFINITION_SHAPE($,$,#168);
#34515=PRODUCT_DEFINITION_SHAPE($,$,#169);
#34516=PRODUCT_DEFINITION_SHAPE($,$,#170);
#34517=PRODUCT_DEFINITION_SHAPE($,$,#171);
#34518=PRODUCT_DEFINITION_SHAPE($,$,#172);
#34519=PRODUCT_DEFINITION_SHAPE($,$,#173);
#34520=PRODUCT_DEFINITION_SHAPE('',$,#34586);
#34521=PRODUCT_DEFINITION_SHAPE('',$,#34587);
#34522=PRODUCT_DEFINITION_SHAPE($,$,#174);
#34523=PRODUCT_DEFINITION_SHAPE('',$,#34588);
#34524=PRODUCT_DEFINITION_SHAPE('',$,#34589);
#34525=PRODUCT_DEFINITION_SHAPE($,$,#175);
#34526=PRODUCT_DEFINITION_SHAPE('',$,#34590);
#34527=PRODUCT_DEFINITION_SHAPE('',$,#34591);
#34528=PRODUCT_DEFINITION_SHAPE($,$,#176);
#34529=PRODUCT_DEFINITION_SHAPE('',$,#34592);
#34530=PRODUCT_DEFINITION_SHAPE('',$,#34593);
#34531=PRODUCT_DEFINITION_SHAPE($,$,#177);
#34532=PRODUCT_DEFINITION_SHAPE($,$,#178);
#34533=PRODUCT_DEFINITION_SHAPE($,$,#179);
#34534=PRODUCT_DEFINITION_SHAPE($,$,#180);
#34535=PRODUCT_DEFINITION_SHAPE($,$,#181);
#34536=PRODUCT_DEFINITION_SHAPE($,$,#182);
#34537=SHAPE_REPRESENTATION('',(#9043,#9720,#9721,#9722,#9723,#9724),#34405);
#34538=SHAPE_REPRESENTATION('',(#9044,#9586,#9587,#9588,#9589,#9590,#9591,
#9592,#9593,#9594,#9595,#9596,#9597,#9598,#9599,#9600,#9601,#9602,#9603,
#9604,#9605,#9606,#9607,#9608,#9609,#9610,#9611,#9612,#9613,#9614,#9615,
#9616,#9617,#9618,#9619),#34406);
#34539=SHAPE_REPRESENTATION('',(#9045),#34407);
#34540=SHAPE_REPRESENTATION('',(#9072),#34408);
#34541=SHAPE_REPRESENTATION('',(#9291),#34409);
#34542=SHAPE_REPRESENTATION('',(#9297),#34410);
#34543=SHAPE_REPRESENTATION('',(#9303),#34411);
#34544=SHAPE_REPRESENTATION('',(#9348),#34412);
#34545=SHAPE_REPRESENTATION('',(#9377),#34413);
#34546=SHAPE_REPRESENTATION('',(#9388),#34414);
#34547=SHAPE_REPRESENTATION('',(#9399),#34415);
#34548=SHAPE_REPRESENTATION('',(#9444),#34416);
#34549=SHAPE_REPRESENTATION('',(#9473),#34417);
#34550=SHAPE_REPRESENTATION('',(#9484),#34418);
#34551=SHAPE_REPRESENTATION('',(#9495),#34419);
#34552=SHAPE_REPRESENTATION('',(#9502),#34420);
#34553=SHAPE_REPRESENTATION('',(#9509),#34421);
#34554=SHAPE_REPRESENTATION('',(#9533),#34422);
#34555=SHAPE_REPRESENTATION('',(#9561),#34423);
#34556=SHAPE_REPRESENTATION('',(#9570),#34424);
#34557=SHAPE_REPRESENTATION('',(#9620,#9644),#34425);
#34558=SHAPE_REPRESENTATION('',(#9621),#34426);
#34559=SHAPE_REPRESENTATION('',(#9645,#9669),#34427);
#34560=SHAPE_REPRESENTATION('',(#9646),#34428);
#34561=SHAPE_REPRESENTATION('',(#9670,#9694),#34429);
#34562=SHAPE_REPRESENTATION('',(#9671),#34430);
#34563=SHAPE_REPRESENTATION('',(#9695,#9719),#34431);
#34564=SHAPE_REPRESENTATION('',(#9696),#34432);
#34565=PRODUCT_DEFINITION_CONTEXT('part definition',#34651,'design');
#34566=PRODUCT_DEFINITION('PAT-079',
'PAT-079',#34594,#34565);
#34567=PRODUCT_DEFINITION('Column and clamp arms',
'Column and clamp arms',#34595,#34565);
#34568=PRODUCT_DEFINITION('Base','Base',#34596,#34565);
#34569=PRODUCT_DEFINITION('Threaded column','Threaded column',#34597,#34565);
#34570=PRODUCT_DEFINITION('Flange locating dowel',
'Flange locating dowel',#34598,#34565);
#34571=PRODUCT_DEFINITION('Flange locating dowel (1)',
'Flange locating dowel (1)',#34599,#34565);
#34572=PRODUCT_DEFINITION('Lower 20 mm clamp','Lower 20 mm clamp',#34600,
#34565);
#34573=PRODUCT_DEFINITION('Upper 20 mm clamp','Upper 20 mm clamp',#34601,
#34565);
#34574=PRODUCT_DEFINITION('mm liner half','mm liner half',#34602,#34565);
#34575=PRODUCT_DEFINITION('mm liner half (1)','mm liner half (1)',#34603,
#34565);
#34576=PRODUCT_DEFINITION('Lower 60 mm clamp','Lower 60 mm clamp',#34604,
#34565);
#34577=PRODUCT_DEFINITION('Upper 60 mm clamp','Upper 60 mm clamp',#34605,
#34565);
#34578=PRODUCT_DEFINITION('mm liner half (2)','mm liner half (2)',#34606,
#34565);
#34579=PRODUCT_DEFINITION('mm liner half (3)','mm liner half (3)',#34607,
#34565);
#34580=PRODUCT_DEFINITION('Foot pad','Foot pad',#34608,#34565);
#34581=PRODUCT_DEFINITION('Foot pad (1)','Foot pad (1)',#34609,#34565);
#34582=PRODUCT_DEFINITION('M6x18 mounting screw','M6x18 mounting screw',
#34610,#34565);
#34583=PRODUCT_DEFINITION('M8x40 clamp bolt','M8x40 clamp bolt',#34611,
#34565);
#34584=PRODUCT_DEFINITION('Flat Washer - M8','Flat Washer - M8',#34612,
#34565);
#34585=PRODUCT_DEFINITION('Hex Nut - M8','Hex Nut - M8',#34613,#34565);
#34586=PRODUCT_DEFINITION('Column nut 1','Column nut 1',#34614,#34565);
#34587=PRODUCT_DEFINITION('M24 adjustment nut','M24 adjustment nut',#34615,
#34565);
#34588=PRODUCT_DEFINITION('Column nut 2','Column nut 2',#34616,#34565);
#34589=PRODUCT_DEFINITION('M24 adjustment nut (1)',
'M24 adjustment nut (1)',#34617,#34565);
#34590=PRODUCT_DEFINITION('Column nut 3','Column nut 3',#34618,#34565);
#34591=PRODUCT_DEFINITION('M24 adjustment nut (2)',
'M24 adjustment nut (2)',#34619,#34565);
#34592=PRODUCT_DEFINITION('Column nut 4','Column nut 4',#34620,#34565);
#34593=PRODUCT_DEFINITION('M24 adjustment nut (3)',
'M24 adjustment nut (3)',#34621,#34565);
#34594=PRODUCT_DEFINITION_FORMATION('',$,#34653);
#34595=PRODUCT_DEFINITION_FORMATION('',$,#34654);
#34596=PRODUCT_DEFINITION_FORMATION('',$,#34655);
#34597=PRODUCT_DEFINITION_FORMATION('',$,#34656);
#34598=PRODUCT_DEFINITION_FORMATION('',$,#34657);
#34599=PRODUCT_DEFINITION_FORMATION('',$,#34658);
#34600=PRODUCT_DEFINITION_FORMATION('',$,#34659);
#34601=PRODUCT_DEFINITION_FORMATION('',$,#34660);
#34602=PRODUCT_DEFINITION_FORMATION('',$,#34661);
#34603=PRODUCT_DEFINITION_FORMATION('',$,#34662);
#34604=PRODUCT_DEFINITION_FORMATION('',$,#34663);
#34605=PRODUCT_DEFINITION_FORMATION('',$,#34664);
#34606=PRODUCT_DEFINITION_FORMATION('',$,#34665);
#34607=PRODUCT_DEFINITION_FORMATION('',$,#34666);
#34608=PRODUCT_DEFINITION_FORMATION('',$,#34667);
#34609=PRODUCT_DEFINITION_FORMATION('',$,#34668);
#34610=PRODUCT_DEFINITION_FORMATION('',$,#34669);
#34611=PRODUCT_DEFINITION_FORMATION('',$,#34670);
#34612=PRODUCT_DEFINITION_FORMATION('',$,#34671);
#34613=PRODUCT_DEFINITION_FORMATION('',$,#34672);
#34614=PRODUCT_DEFINITION_FORMATION('',$,#34673);
#34615=PRODUCT_DEFINITION_FORMATION('',$,#34674);
#34616=PRODUCT_DEFINITION_FORMATION('',$,#34675);
#34617=PRODUCT_DEFINITION_FORMATION('',$,#34676);
#34618=PRODUCT_DEFINITION_FORMATION('',$,#34677);
#34619=PRODUCT_DEFINITION_FORMATION('',$,#34678);
#34620=PRODUCT_DEFINITION_FORMATION('',$,#34679);
#34621=PRODUCT_DEFINITION_FORMATION('',$,#34680);
#34622=PRODUCT_RELATED_PRODUCT_CATEGORY('PAT-079','PAT-079',(#34653));
#34623=PRODUCT_RELATED_PRODUCT_CATEGORY('Column and clamp arms',
'Column and clamp arms',(#34654));
#34624=PRODUCT_RELATED_PRODUCT_CATEGORY('Base','Base',(#34655));
#34625=PRODUCT_RELATED_PRODUCT_CATEGORY('Threaded column',
'Threaded column',(#34656));
#34626=PRODUCT_RELATED_PRODUCT_CATEGORY('Flange locating dowel',
'Flange locating dowel',(#34657));
#34627=PRODUCT_RELATED_PRODUCT_CATEGORY('Flange locating dowel (1)',
'Flange locating dowel (1)',(#34658));
#34628=PRODUCT_RELATED_PRODUCT_CATEGORY('Lower 20 mm clamp',
'Lower 20 mm clamp',(#34659));
#34629=PRODUCT_RELATED_PRODUCT_CATEGORY('Upper 20 mm clamp',
'Upper 20 mm clamp',(#34660));
#34630=PRODUCT_RELATED_PRODUCT_CATEGORY('mm liner half','mm liner half',
(#34661));
#34631=PRODUCT_RELATED_PRODUCT_CATEGORY('mm liner half (1)',
'mm liner half (1)',(#34662));
#34632=PRODUCT_RELATED_PRODUCT_CATEGORY('Lower 60 mm clamp',
'Lower 60 mm clamp',(#34663));
#34633=PRODUCT_RELATED_PRODUCT_CATEGORY('Upper 60 mm clamp',
'Upper 60 mm clamp',(#34664));
#34634=PRODUCT_RELATED_PRODUCT_CATEGORY('mm liner half (2)',
'mm liner half (2)',(#34665));
#34635=PRODUCT_RELATED_PRODUCT_CATEGORY('mm liner half (3)',
'mm liner half (3)',(#34666));
#34636=PRODUCT_RELATED_PRODUCT_CATEGORY('Foot pad','Foot pad',(#34667));
#34637=PRODUCT_RELATED_PRODUCT_CATEGORY('Foot pad (1)','Foot pad (1)',(#34668));
#34638=PRODUCT_RELATED_PRODUCT_CATEGORY('M6x18 mounting screw',
'M6x18 mounting screw',(#34669));
#34639=PRODUCT_RELATED_PRODUCT_CATEGORY('M8x40 clamp bolt',
'M8x40 clamp bolt',(#34670));
#34640=PRODUCT_RELATED_PRODUCT_CATEGORY('Flat Washer - M8',
'Flat Washer - M8',(#34671));
#34641=PRODUCT_RELATED_PRODUCT_CATEGORY('Hex Nut - M8','Hex Nut - M8',(#34672));
#34642=PRODUCT_RELATED_PRODUCT_CATEGORY('Column nut 1','Column nut 1',(#34673));
#34643=PRODUCT_RELATED_PRODUCT_CATEGORY('M24 adjustment nut',
'M24 adjustment nut',(#34674));
#34644=PRODUCT_RELATED_PRODUCT_CATEGORY('Column nut 2','Column nut 2',(#34675));
#34645=PRODUCT_RELATED_PRODUCT_CATEGORY('M24 adjustment nut (1)',
'M24 adjustment nut (1)',(#34676));
#34646=PRODUCT_RELATED_PRODUCT_CATEGORY('Column nut 3','Column nut 3',(#34677));
#34647=PRODUCT_RELATED_PRODUCT_CATEGORY('M24 adjustment nut (2)',
'M24 adjustment nut (2)',(#34678));
#34648=PRODUCT_RELATED_PRODUCT_CATEGORY('Column nut 4','Column nut 4',(#34679));
#34649=PRODUCT_RELATED_PRODUCT_CATEGORY('M24 adjustment nut (3)',
'M24 adjustment nut (3)',(#34680));
#34650=APPLICATION_PROTOCOL_DEFINITION('international standard',
'automotive_design',2009,#34651);
#34651=APPLICATION_CONTEXT(
'Core Data for Automotive Mechanical Design Process');
#34652=PRODUCT_CONTEXT('part definition',#34651,'mechanical');
#34653=PRODUCT('PAT-079','PAT-079',
'PAT-079',(#34652));
#34654=PRODUCT('Column and clamp arms','Column and clamp arms',
'Column and clamp arms',(#34652));
#34655=PRODUCT('Base','Base','Base',(#34652));
#34656=PRODUCT('Threaded column','Threaded column','Threaded column',(#34652));
#34657=PRODUCT('Flange locating dowel','Flange locating dowel',
'Flange locating dowel',(#34652));
#34658=PRODUCT('Flange locating dowel (1)','Flange locating dowel (1)',
'Flange locating dowel (1)',(#34652));
#34659=PRODUCT('Lower 20 mm clamp','Lower 20 mm clamp',
'Lower 20 mm clamp',(#34652));
#34660=PRODUCT('Upper 20 mm clamp','Upper 20 mm clamp',
'Upper 20 mm clamp',(#34652));
#34661=PRODUCT('mm liner half','mm liner half','mm liner half',(#34652));
#34662=PRODUCT('mm liner half (1)','mm liner half (1)','mm liner half (1)',(#34652));
#34663=PRODUCT('Lower 60 mm clamp','Lower 60 mm clamp',
'Lower 60 mm clamp',(#34652));
#34664=PRODUCT('Upper 60 mm clamp','Upper 60 mm clamp',
'Upper 60 mm clamp',(#34652));
#34665=PRODUCT('mm liner half (2)','mm liner half (2)','mm liner half (2)',(#34652));
#34666=PRODUCT('mm liner half (3)','mm liner half (3)','mm liner half (3)',(#34652));
#34667=PRODUCT('Foot pad','Foot pad','Foot pad',(#34652));
#34668=PRODUCT('Foot pad (1)','Foot pad (1)','Foot pad (1)',(#34652));
#34669=PRODUCT('M6x18 mounting screw','M6x18 mounting screw',
'M6x18 mounting screw',(#34652));
#34670=PRODUCT('M8x40 clamp bolt','M8x40 clamp bolt','M8x40 clamp bolt',
(#34652));
#34671=PRODUCT('Flat Washer - M8','Flat Washer - M8','Flat Washer - M8',
(#34652));
#34672=PRODUCT('Hex Nut - M8','Hex Nut - M8','Hex Nut - M8',(#34652));
#34673=PRODUCT('Column nut 1','Column nut 1','Column nut 1',(#34652));
#34674=PRODUCT('M24 adjustment nut','M24 adjustment nut',
'M24 adjustment nut',(#34652));
#34675=PRODUCT('Column nut 2','Column nut 2','Column nut 2',(#34652));
#34676=PRODUCT('M24 adjustment nut (1)','M24 adjustment nut (1)',
'M24 adjustment nut (1)',(#34652));
#34677=PRODUCT('Column nut 3','Column nut 3','Column nut 3',(#34652));
#34678=PRODUCT('M24 adjustment nut (2)','M24 adjustment nut (2)',
'M24 adjustment nut (2)',(#34652));
#34679=PRODUCT('Column nut 4','Column nut 4','Column nut 4',(#34652));
#34680=PRODUCT('M24 adjustment nut (3)','M24 adjustment nut (3)',
'M24 adjustment nut (3)',(#34652));
#34681=PRESENTATION_STYLE_ASSIGNMENT((#34686));
#34682=PRESENTATION_STYLE_ASSIGNMENT((#34687));
#34683=PRESENTATION_STYLE_ASSIGNMENT((#34688));
#34684=PRESENTATION_STYLE_ASSIGNMENT((#34689));
#34685=PRESENTATION_STYLE_ASSIGNMENT((#34690));
#34686=SURFACE_STYLE_USAGE(.BOTH.,#34691);
#34687=SURFACE_STYLE_USAGE(.BOTH.,#34692);
#34688=SURFACE_STYLE_USAGE(.BOTH.,#34693);
#34689=SURFACE_STYLE_USAGE(.BOTH.,#34694);
#34690=SURFACE_STYLE_USAGE(.BOTH.,#34695);
#34691=SURFACE_SIDE_STYLE('',(#34696));
#34692=SURFACE_SIDE_STYLE('',(#34697));
#34693=SURFACE_SIDE_STYLE('',(#34698));
#34694=SURFACE_SIDE_STYLE('',(#34699));
#34695=SURFACE_SIDE_STYLE('',(#34700));
#34696=SURFACE_STYLE_FILL_AREA(#34701);
#34697=SURFACE_STYLE_FILL_AREA(#34702);
#34698=SURFACE_STYLE_FILL_AREA(#34703);
#34699=SURFACE_STYLE_FILL_AREA(#34704);
#34700=SURFACE_STYLE_FILL_AREA(#34705);
#34701=FILL_AREA_STYLE('Steel - Satin',(#34706));
#34702=FILL_AREA_STYLE('CAD Library Painted - Deep blue',(#34707));
#34703=FILL_AREA_STYLE('CAD Library Painted - Engineering blue',(#34708));
#34704=FILL_AREA_STYLE('CAD Library Painted - Graphite',(#34709));
#34705=FILL_AREA_STYLE('CAD Library Painted - Steel gray',(#34710));
#34706=FILL_AREA_STYLE_COLOUR('Steel - Satin',#34711);
#34707=FILL_AREA_STYLE_COLOUR('CAD Library Painted - Deep blue',#34712);
#34708=FILL_AREA_STYLE_COLOUR('CAD Library Painted - Engineering blue',
#34713);
#34709=FILL_AREA_STYLE_COLOUR('CAD Library Painted - Graphite',#34714);
#34710=FILL_AREA_STYLE_COLOUR('CAD Library Painted - Steel gray',#34715);
#34711=COLOUR_RGB('Steel - Satin',0.627450980392157,0.627450980392157,0.627450980392157);
#34712=COLOUR_RGB('CAD Library Painted - Deep blue',0.0784313725490196,
0.203921568627451,0.349019607843137);
#34713=COLOUR_RGB('CAD Library Painted - Engineering blue',0.12156862745098,
0.356862745098039,0.6);
#34714=COLOUR_RGB('CAD Library Painted - Graphite',0.168627450980392,0.192156862745098,
0.231372549019608);
#34715=COLOUR_RGB('CAD Library Painted - Steel gray',0.592156862745098,
0.631372549019608,0.67843137254902);
#34716=COLOUR_RGB('Dark Blue',0.08,0.2,0.34);
#34717=FILL_AREA_STYLE_COLOUR('',#34716);
#34718=FILL_AREA_STYLE('',(#34717));
#34719=SURFACE_STYLE_FILL_AREA(#34718);
#34720=SURFACE_SIDE_STYLE('',(#34719));
#34721=SURFACE_STYLE_USAGE(.BOTH.,#34720);
#34722=PRESENTATION_STYLE_ASSIGNMENT((#34721));
#34723=COLOUR_RGB('Light Blue',0.38,0.62,0.78);
#34724=FILL_AREA_STYLE_COLOUR('',#34723);
#34725=FILL_AREA_STYLE('',(#34724));
#34726=SURFACE_STYLE_FILL_AREA(#34725);
#34727=SURFACE_SIDE_STYLE('',(#34726));
#34728=SURFACE_STYLE_USAGE(.BOTH.,#34727);
#34729=PRESENTATION_STYLE_ASSIGNMENT((#34728));
#34730=COLOUR_RGB('Sky Blue',0.24,0.69,0.87);
#34731=FILL_AREA_STYLE_COLOUR('',#34730);
#34732=FILL_AREA_STYLE('',(#34731));
#34733=SURFACE_STYLE_FILL_AREA(#34732);
#34734=SURFACE_SIDE_STYLE('',(#34733));
#34735=SURFACE_STYLE_USAGE(.BOTH.,#34734);
#34736=PRESENTATION_STYLE_ASSIGNMENT((#34735));
#34737=COLOUR_RGB('Grey',0.48,0.52,0.57);
#34738=FILL_AREA_STYLE_COLOUR('',#34737);
#34739=FILL_AREA_STYLE('',(#34738));
#34740=SURFACE_STYLE_FILL_AREA(#34739);
#34741=SURFACE_SIDE_STYLE('',(#34740));
#34742=SURFACE_STYLE_USAGE(.BOTH.,#34741);
#34743=PRESENTATION_STYLE_ASSIGNMENT((#34742));
#34744=COLOUR_RGB('Black',0.12,0.14,0.17);
#34745=FILL_AREA_STYLE_COLOUR('',#34744);
#34746=FILL_AREA_STYLE('',(#34745));
#34747=SURFACE_STYLE_FILL_AREA(#34746);
#34748=SURFACE_SIDE_STYLE('',(#34747));
#34749=SURFACE_STYLE_USAGE(.BOTH.,#34748);
#34750=PRESENTATION_STYLE_ASSIGNMENT((#34749));
#34751=COLOUR_RGB('Off White',0.89,0.88,0.83);
#34752=FILL_AREA_STYLE_COLOUR('',#34751);
#34753=FILL_AREA_STYLE('',(#34752));
#34754=SURFACE_STYLE_FILL_AREA(#34753);
#34755=SURFACE_SIDE_STYLE('',(#34754));
#34756=SURFACE_STYLE_USAGE(.BOTH.,#34755);
#34757=PRESENTATION_STYLE_ASSIGNMENT((#34756));
ENDSEC;
END-ISO-10303-21;
